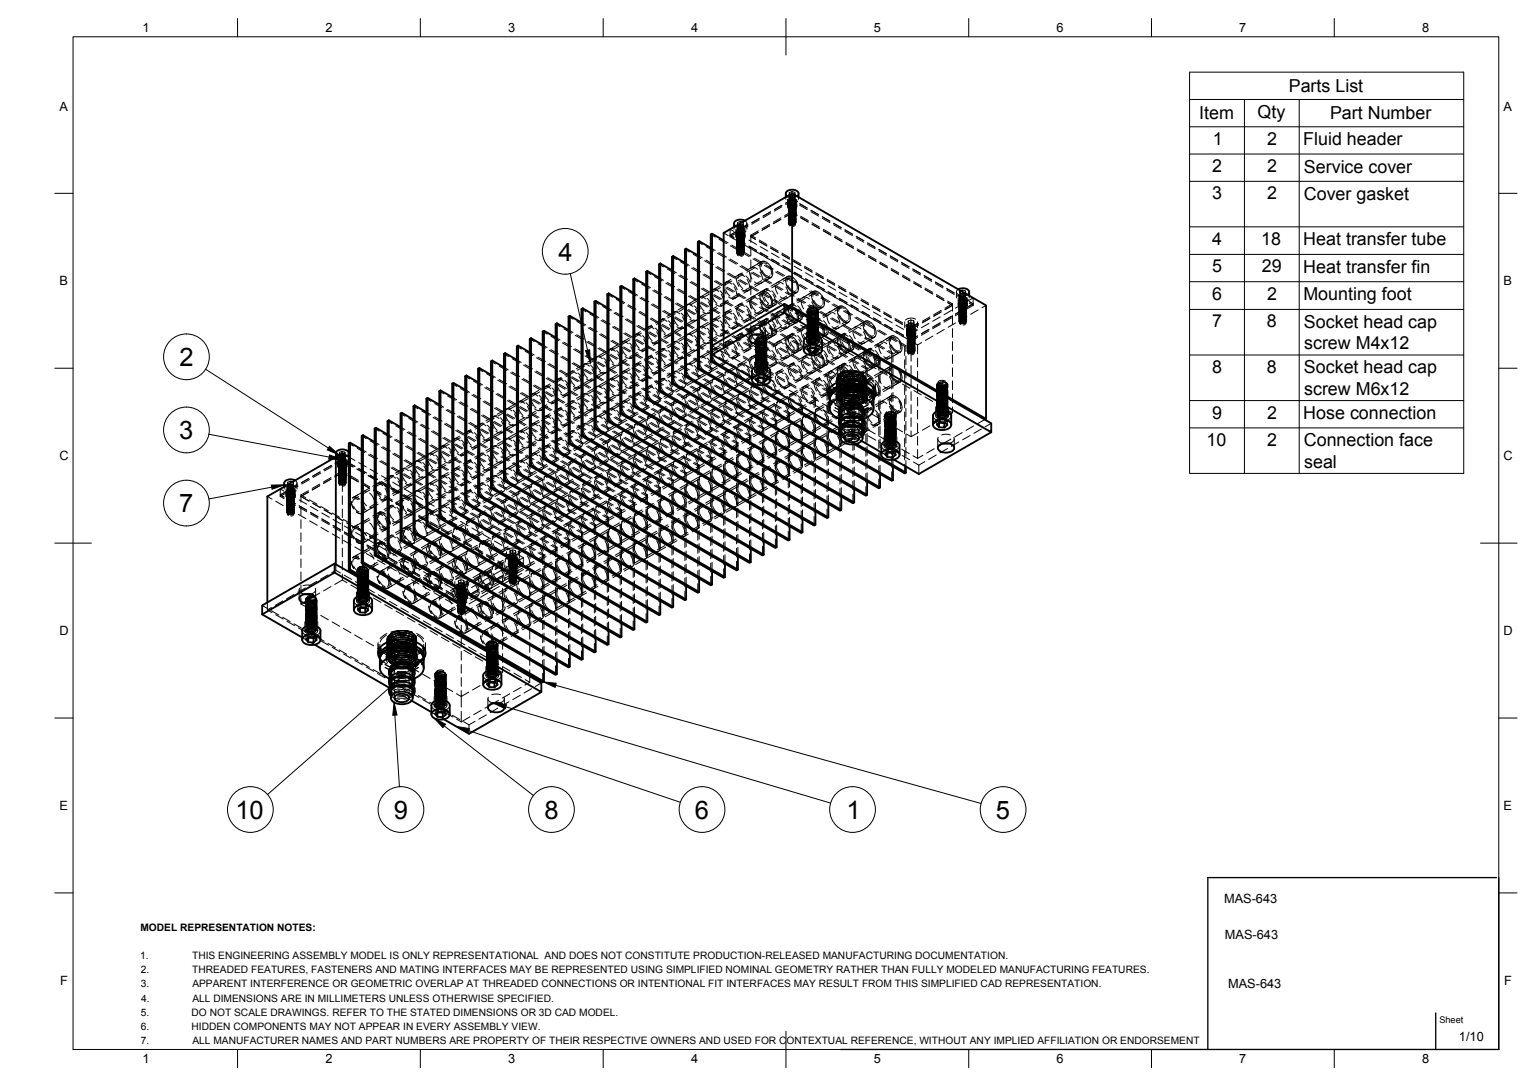
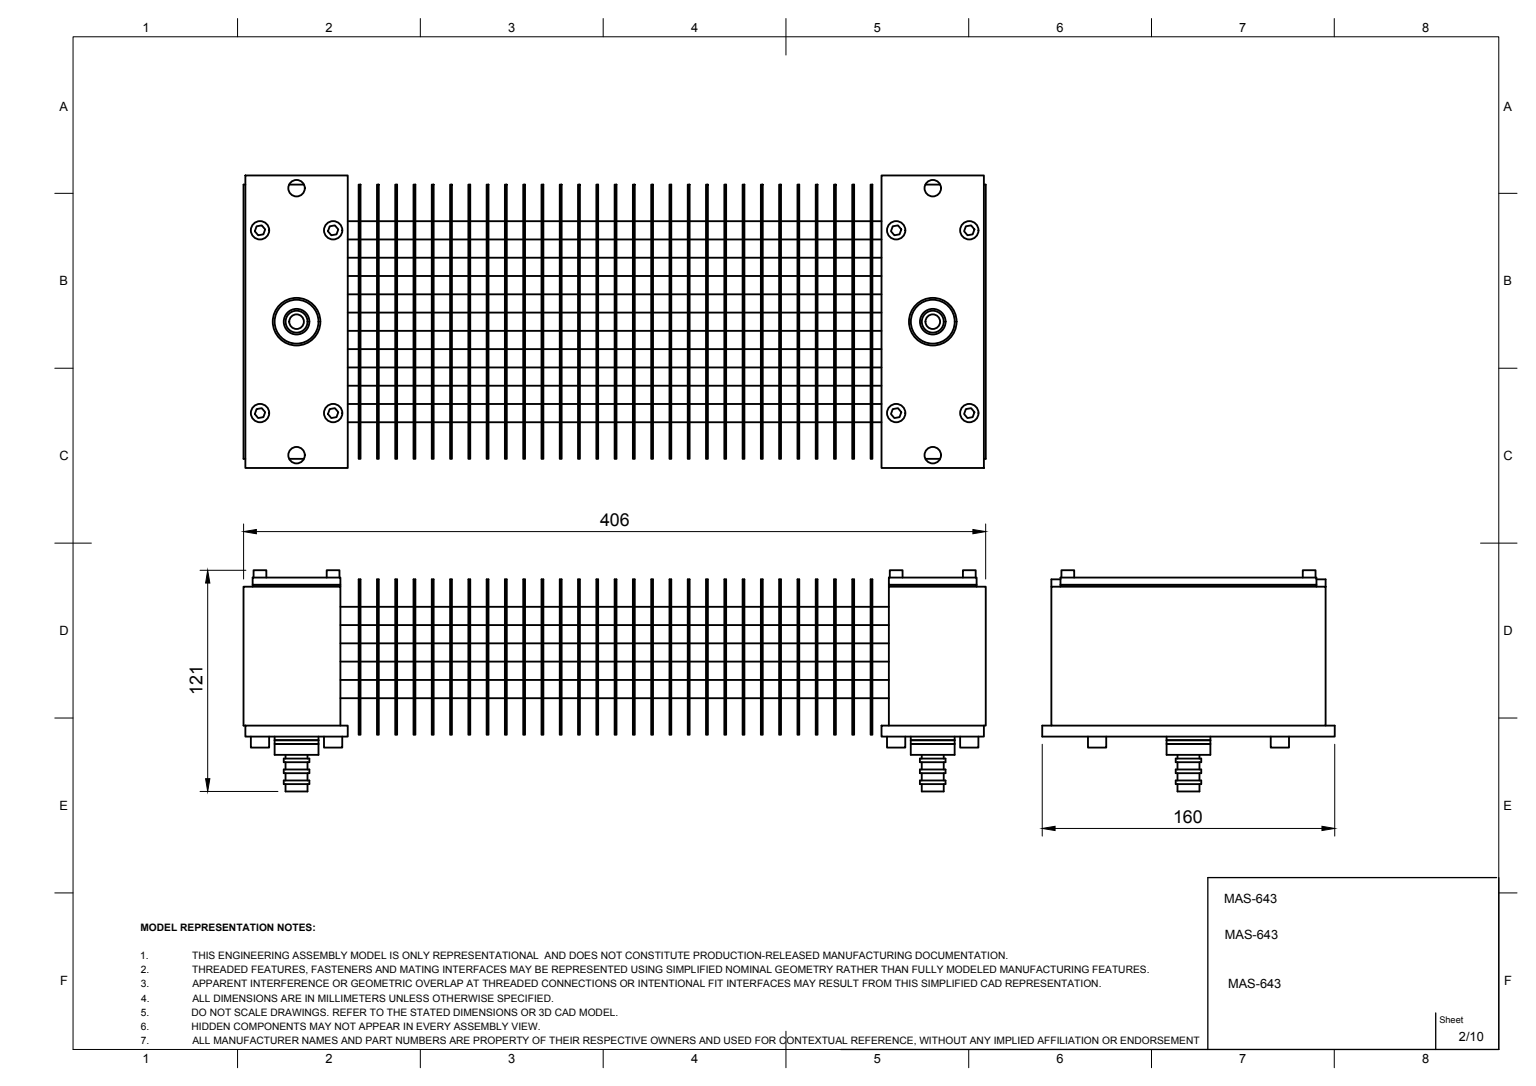
ISO-10303-21;
HEADER;
/* Generated by software containing ST-Developer
 * from STEP Tools, Inc. (www.steptools.com) 
 */

FILE_DESCRIPTION(
/* description */ ('Independent eighteen-tube parallel-flow evaporator geometry. Repeated
 machined headers and gasketed service covers, eighteen copper tubes, 
twenty-nine punched fins, threaded hose connections and bolted mountin
g feet. Native editable features and instanced parts. Braze details, w
orking fluid, pressure and thermal ratings require engineering selecti
on.'),
/* implementation_level */ '2;1');

FILE_NAME(
/* name */ 'MAS-643.step',
/* time_stamp */ '2026-11-08T20:53:59-08:00',
/* author */ (''),
/* organization */ (''),
/* preprocessor_version */ 'ST-DEVELOPER v20.2',
/* originating_system */ 'Autodesk Translation Framework v15.17.0.0',
/* authorisation */ '');

FILE_SCHEMA (('AUTOMOTIVE_DESIGN { 1 0 10303 214 3 1 1 }'));
ENDSEC;

DATA;
#10=MECHANICAL_DESIGN_GEOMETRIC_PRESENTATION_REPRESENTATION('',(#333,#334,
#335,#336,#337,#338,#339,#340,#341,#342),#42620);
#11=ITEM_DEFINED_TRANSFORMATION($,$,#10505,#11231);
#12=ITEM_DEFINED_TRANSFORMATION($,$,#10921,#11232);
#13=ITEM_DEFINED_TRANSFORMATION($,$,#10940,#11233);
#14=ITEM_DEFINED_TRANSFORMATION($,$,#10963,#11234);
#15=ITEM_DEFINED_TRANSFORMATION($,$,#10972,#11235);
#16=ITEM_DEFINED_TRANSFORMATION($,$,#11033,#11236);
#17=ITEM_DEFINED_TRANSFORMATION($,$,#11061,#11237);
#18=ITEM_DEFINED_TRANSFORMATION($,$,#11115,#11238);
#19=ITEM_DEFINED_TRANSFORMATION($,$,#11159,#11239);
#20=ITEM_DEFINED_TRANSFORMATION($,$,#11222,#11240);
#21=ITEM_DEFINED_TRANSFORMATION($,$,#10505,#11241);
#22=ITEM_DEFINED_TRANSFORMATION($,$,#10921,#11242);
#23=ITEM_DEFINED_TRANSFORMATION($,$,#10940,#11243);
#24=ITEM_DEFINED_TRANSFORMATION($,$,#10963,#11244);
#25=ITEM_DEFINED_TRANSFORMATION($,$,#10963,#11245);
#26=ITEM_DEFINED_TRANSFORMATION($,$,#10963,#11246);
#27=ITEM_DEFINED_TRANSFORMATION($,$,#10963,#11247);
#28=ITEM_DEFINED_TRANSFORMATION($,$,#10963,#11248);
#29=ITEM_DEFINED_TRANSFORMATION($,$,#10963,#11249);
#30=ITEM_DEFINED_TRANSFORMATION($,$,#10963,#11250);
#31=ITEM_DEFINED_TRANSFORMATION($,$,#10963,#11251);
#32=ITEM_DEFINED_TRANSFORMATION($,$,#10963,#11252);
#33=ITEM_DEFINED_TRANSFORMATION($,$,#10963,#11253);
#34=ITEM_DEFINED_TRANSFORMATION($,$,#10963,#11254);
#35=ITEM_DEFINED_TRANSFORMATION($,$,#10963,#11255);
#36=ITEM_DEFINED_TRANSFORMATION($,$,#10963,#11256);
#37=ITEM_DEFINED_TRANSFORMATION($,$,#10963,#11257);
#38=ITEM_DEFINED_TRANSFORMATION($,$,#10963,#11258);
#39=ITEM_DEFINED_TRANSFORMATION($,$,#10963,#11259);
#40=ITEM_DEFINED_TRANSFORMATION($,$,#10963,#11260);
#41=ITEM_DEFINED_TRANSFORMATION($,$,#10972,#11261);
#42=ITEM_DEFINED_TRANSFORMATION($,$,#10972,#11262);
#43=ITEM_DEFINED_TRANSFORMATION($,$,#10972,#11263);
#44=ITEM_DEFINED_TRANSFORMATION($,$,#10972,#11264);
#45=ITEM_DEFINED_TRANSFORMATION($,$,#10972,#11265);
#46=ITEM_DEFINED_TRANSFORMATION($,$,#10972,#11266);
#47=ITEM_DEFINED_TRANSFORMATION($,$,#10972,#11267);
#48=ITEM_DEFINED_TRANSFORMATION($,$,#10972,#11268);
#49=ITEM_DEFINED_TRANSFORMATION($,$,#10972,#11269);
#50=ITEM_DEFINED_TRANSFORMATION($,$,#10972,#11270);
#51=ITEM_DEFINED_TRANSFORMATION($,$,#10972,#11271);
#52=ITEM_DEFINED_TRANSFORMATION($,$,#10972,#11272);
#53=ITEM_DEFINED_TRANSFORMATION($,$,#10972,#11273);
#54=ITEM_DEFINED_TRANSFORMATION($,$,#10972,#11274);
#55=ITEM_DEFINED_TRANSFORMATION($,$,#10972,#11275);
#56=ITEM_DEFINED_TRANSFORMATION($,$,#10972,#11276);
#57=ITEM_DEFINED_TRANSFORMATION($,$,#10972,#11277);
#58=ITEM_DEFINED_TRANSFORMATION($,$,#10972,#11278);
#59=ITEM_DEFINED_TRANSFORMATION($,$,#10972,#11279);
#60=ITEM_DEFINED_TRANSFORMATION($,$,#10972,#11280);
#61=ITEM_DEFINED_TRANSFORMATION($,$,#10972,#11281);
#62=ITEM_DEFINED_TRANSFORMATION($,$,#10972,#11282);
#63=ITEM_DEFINED_TRANSFORMATION($,$,#10972,#11283);
#64=ITEM_DEFINED_TRANSFORMATION($,$,#10972,#11284);
#65=ITEM_DEFINED_TRANSFORMATION($,$,#10972,#11285);
#66=ITEM_DEFINED_TRANSFORMATION($,$,#10972,#11286);
#67=ITEM_DEFINED_TRANSFORMATION($,$,#10972,#11287);
#68=ITEM_DEFINED_TRANSFORMATION($,$,#10972,#11288);
#69=ITEM_DEFINED_TRANSFORMATION($,$,#11033,#11289);
#70=ITEM_DEFINED_TRANSFORMATION($,$,#11061,#11290);
#71=ITEM_DEFINED_TRANSFORMATION($,$,#11061,#11291);
#72=ITEM_DEFINED_TRANSFORMATION($,$,#11061,#11292);
#73=ITEM_DEFINED_TRANSFORMATION($,$,#11061,#11293);
#74=ITEM_DEFINED_TRANSFORMATION($,$,#11061,#11294);
#75=ITEM_DEFINED_TRANSFORMATION($,$,#11061,#11295);
#76=ITEM_DEFINED_TRANSFORMATION($,$,#11061,#11296);
#77=ITEM_DEFINED_TRANSFORMATION($,$,#11115,#11297);
#78=ITEM_DEFINED_TRANSFORMATION($,$,#11115,#11298);
#79=ITEM_DEFINED_TRANSFORMATION($,$,#11115,#11299);
#80=ITEM_DEFINED_TRANSFORMATION($,$,#11115,#11300);
#81=ITEM_DEFINED_TRANSFORMATION($,$,#11115,#11301);
#82=ITEM_DEFINED_TRANSFORMATION($,$,#11115,#11302);
#83=ITEM_DEFINED_TRANSFORMATION($,$,#11115,#11303);
#84=ITEM_DEFINED_TRANSFORMATION($,$,#11159,#11304);
#85=ITEM_DEFINED_TRANSFORMATION($,$,#11222,#11305);
#86=(
REPRESENTATION_RELATIONSHIP($,$,#42723,#42722)
REPRESENTATION_RELATIONSHIP_WITH_TRANSFORMATION(#11)
SHAPE_REPRESENTATION_RELATIONSHIP()
);
#87=(
REPRESENTATION_RELATIONSHIP($,$,#42724,#42722)
REPRESENTATION_RELATIONSHIP_WITH_TRANSFORMATION(#12)
SHAPE_REPRESENTATION_RELATIONSHIP()
);
#88=(
REPRESENTATION_RELATIONSHIP($,$,#42725,#42722)
REPRESENTATION_RELATIONSHIP_WITH_TRANSFORMATION(#13)
SHAPE_REPRESENTATION_RELATIONSHIP()
);
#89=(
REPRESENTATION_RELATIONSHIP($,$,#42726,#42722)
REPRESENTATION_RELATIONSHIP_WITH_TRANSFORMATION(#14)
SHAPE_REPRESENTATION_RELATIONSHIP()
);
#90=(
REPRESENTATION_RELATIONSHIP($,$,#42727,#42722)
REPRESENTATION_RELATIONSHIP_WITH_TRANSFORMATION(#15)
SHAPE_REPRESENTATION_RELATIONSHIP()
);
#91=(
REPRESENTATION_RELATIONSHIP($,$,#42728,#42722)
REPRESENTATION_RELATIONSHIP_WITH_TRANSFORMATION(#16)
SHAPE_REPRESENTATION_RELATIONSHIP()
);
#92=(
REPRESENTATION_RELATIONSHIP($,$,#42729,#42722)
REPRESENTATION_RELATIONSHIP_WITH_TRANSFORMATION(#17)
SHAPE_REPRESENTATION_RELATIONSHIP()
);
#93=(
REPRESENTATION_RELATIONSHIP($,$,#42730,#42722)
REPRESENTATION_RELATIONSHIP_WITH_TRANSFORMATION(#18)
SHAPE_REPRESENTATION_RELATIONSHIP()
);
#94=(
REPRESENTATION_RELATIONSHIP($,$,#42731,#42722)
REPRESENTATION_RELATIONSHIP_WITH_TRANSFORMATION(#19)
SHAPE_REPRESENTATION_RELATIONSHIP()
);
#95=(
REPRESENTATION_RELATIONSHIP($,$,#42732,#42722)
REPRESENTATION_RELATIONSHIP_WITH_TRANSFORMATION(#20)
SHAPE_REPRESENTATION_RELATIONSHIP()
);
#96=(
REPRESENTATION_RELATIONSHIP($,$,#42723,#42722)
REPRESENTATION_RELATIONSHIP_WITH_TRANSFORMATION(#21)
SHAPE_REPRESENTATION_RELATIONSHIP()
);
#97=(
REPRESENTATION_RELATIONSHIP($,$,#42724,#42722)
REPRESENTATION_RELATIONSHIP_WITH_TRANSFORMATION(#22)
SHAPE_REPRESENTATION_RELATIONSHIP()
);
#98=(
REPRESENTATION_RELATIONSHIP($,$,#42725,#42722)
REPRESENTATION_RELATIONSHIP_WITH_TRANSFORMATION(#23)
SHAPE_REPRESENTATION_RELATIONSHIP()
);
#99=(
REPRESENTATION_RELATIONSHIP($,$,#42726,#42722)
REPRESENTATION_RELATIONSHIP_WITH_TRANSFORMATION(#24)
SHAPE_REPRESENTATION_RELATIONSHIP()
);
#100=(
REPRESENTATION_RELATIONSHIP($,$,#42726,#42722)
REPRESENTATION_RELATIONSHIP_WITH_TRANSFORMATION(#25)
SHAPE_REPRESENTATION_RELATIONSHIP()
);
#101=(
REPRESENTATION_RELATIONSHIP($,$,#42726,#42722)
REPRESENTATION_RELATIONSHIP_WITH_TRANSFORMATION(#26)
SHAPE_REPRESENTATION_RELATIONSHIP()
);
#102=(
REPRESENTATION_RELATIONSHIP($,$,#42726,#42722)
REPRESENTATION_RELATIONSHIP_WITH_TRANSFORMATION(#27)
SHAPE_REPRESENTATION_RELATIONSHIP()
);
#103=(
REPRESENTATION_RELATIONSHIP($,$,#42726,#42722)
REPRESENTATION_RELATIONSHIP_WITH_TRANSFORMATION(#28)
SHAPE_REPRESENTATION_RELATIONSHIP()
);
#104=(
REPRESENTATION_RELATIONSHIP($,$,#42726,#42722)
REPRESENTATION_RELATIONSHIP_WITH_TRANSFORMATION(#29)
SHAPE_REPRESENTATION_RELATIONSHIP()
);
#105=(
REPRESENTATION_RELATIONSHIP($,$,#42726,#42722)
REPRESENTATION_RELATIONSHIP_WITH_TRANSFORMATION(#30)
SHAPE_REPRESENTATION_RELATIONSHIP()
);
#106=(
REPRESENTATION_RELATIONSHIP($,$,#42726,#42722)
REPRESENTATION_RELATIONSHIP_WITH_TRANSFORMATION(#31)
SHAPE_REPRESENTATION_RELATIONSHIP()
);
#107=(
REPRESENTATION_RELATIONSHIP($,$,#42726,#42722)
REPRESENTATION_RELATIONSHIP_WITH_TRANSFORMATION(#32)
SHAPE_REPRESENTATION_RELATIONSHIP()
);
#108=(
REPRESENTATION_RELATIONSHIP($,$,#42726,#42722)
REPRESENTATION_RELATIONSHIP_WITH_TRANSFORMATION(#33)
SHAPE_REPRESENTATION_RELATIONSHIP()
);
#109=(
REPRESENTATION_RELATIONSHIP($,$,#42726,#42722)
REPRESENTATION_RELATIONSHIP_WITH_TRANSFORMATION(#34)
SHAPE_REPRESENTATION_RELATIONSHIP()
);
#110=(
REPRESENTATION_RELATIONSHIP($,$,#42726,#42722)
REPRESENTATION_RELATIONSHIP_WITH_TRANSFORMATION(#35)
SHAPE_REPRESENTATION_RELATIONSHIP()
);
#111=(
REPRESENTATION_RELATIONSHIP($,$,#42726,#42722)
REPRESENTATION_RELATIONSHIP_WITH_TRANSFORMATION(#36)
SHAPE_REPRESENTATION_RELATIONSHIP()
);
#112=(
REPRESENTATION_RELATIONSHIP($,$,#42726,#42722)
REPRESENTATION_RELATIONSHIP_WITH_TRANSFORMATION(#37)
SHAPE_REPRESENTATION_RELATIONSHIP()
);
#113=(
REPRESENTATION_RELATIONSHIP($,$,#42726,#42722)
REPRESENTATION_RELATIONSHIP_WITH_TRANSFORMATION(#38)
SHAPE_REPRESENTATION_RELATIONSHIP()
);
#114=(
REPRESENTATION_RELATIONSHIP($,$,#42726,#42722)
REPRESENTATION_RELATIONSHIP_WITH_TRANSFORMATION(#39)
SHAPE_REPRESENTATION_RELATIONSHIP()
);
#115=(
REPRESENTATION_RELATIONSHIP($,$,#42726,#42722)
REPRESENTATION_RELATIONSHIP_WITH_TRANSFORMATION(#40)
SHAPE_REPRESENTATION_RELATIONSHIP()
);
#116=(
REPRESENTATION_RELATIONSHIP($,$,#42727,#42722)
REPRESENTATION_RELATIONSHIP_WITH_TRANSFORMATION(#41)
SHAPE_REPRESENTATION_RELATIONSHIP()
);
#117=(
REPRESENTATION_RELATIONSHIP($,$,#42727,#42722)
REPRESENTATION_RELATIONSHIP_WITH_TRANSFORMATION(#42)
SHAPE_REPRESENTATION_RELATIONSHIP()
);
#118=(
REPRESENTATION_RELATIONSHIP($,$,#42727,#42722)
REPRESENTATION_RELATIONSHIP_WITH_TRANSFORMATION(#43)
SHAPE_REPRESENTATION_RELATIONSHIP()
);
#119=(
REPRESENTATION_RELATIONSHIP($,$,#42727,#42722)
REPRESENTATION_RELATIONSHIP_WITH_TRANSFORMATION(#44)
SHAPE_REPRESENTATION_RELATIONSHIP()
);
#120=(
REPRESENTATION_RELATIONSHIP($,$,#42727,#42722)
REPRESENTATION_RELATIONSHIP_WITH_TRANSFORMATION(#45)
SHAPE_REPRESENTATION_RELATIONSHIP()
);
#121=(
REPRESENTATION_RELATIONSHIP($,$,#42727,#42722)
REPRESENTATION_RELATIONSHIP_WITH_TRANSFORMATION(#46)
SHAPE_REPRESENTATION_RELATIONSHIP()
);
#122=(
REPRESENTATION_RELATIONSHIP($,$,#42727,#42722)
REPRESENTATION_RELATIONSHIP_WITH_TRANSFORMATION(#47)
SHAPE_REPRESENTATION_RELATIONSHIP()
);
#123=(
REPRESENTATION_RELATIONSHIP($,$,#42727,#42722)
REPRESENTATION_RELATIONSHIP_WITH_TRANSFORMATION(#48)
SHAPE_REPRESENTATION_RELATIONSHIP()
);
#124=(
REPRESENTATION_RELATIONSHIP($,$,#42727,#42722)
REPRESENTATION_RELATIONSHIP_WITH_TRANSFORMATION(#49)
SHAPE_REPRESENTATION_RELATIONSHIP()
);
#125=(
REPRESENTATION_RELATIONSHIP($,$,#42727,#42722)
REPRESENTATION_RELATIONSHIP_WITH_TRANSFORMATION(#50)
SHAPE_REPRESENTATION_RELATIONSHIP()
);
#126=(
REPRESENTATION_RELATIONSHIP($,$,#42727,#42722)
REPRESENTATION_RELATIONSHIP_WITH_TRANSFORMATION(#51)
SHAPE_REPRESENTATION_RELATIONSHIP()
);
#127=(
REPRESENTATION_RELATIONSHIP($,$,#42727,#42722)
REPRESENTATION_RELATIONSHIP_WITH_TRANSFORMATION(#52)
SHAPE_REPRESENTATION_RELATIONSHIP()
);
#128=(
REPRESENTATION_RELATIONSHIP($,$,#42727,#42722)
REPRESENTATION_RELATIONSHIP_WITH_TRANSFORMATION(#53)
SHAPE_REPRESENTATION_RELATIONSHIP()
);
#129=(
REPRESENTATION_RELATIONSHIP($,$,#42727,#42722)
REPRESENTATION_RELATIONSHIP_WITH_TRANSFORMATION(#54)
SHAPE_REPRESENTATION_RELATIONSHIP()
);
#130=(
REPRESENTATION_RELATIONSHIP($,$,#42727,#42722)
REPRESENTATION_RELATIONSHIP_WITH_TRANSFORMATION(#55)
SHAPE_REPRESENTATION_RELATIONSHIP()
);
#131=(
REPRESENTATION_RELATIONSHIP($,$,#42727,#42722)
REPRESENTATION_RELATIONSHIP_WITH_TRANSFORMATION(#56)
SHAPE_REPRESENTATION_RELATIONSHIP()
);
#132=(
REPRESENTATION_RELATIONSHIP($,$,#42727,#42722)
REPRESENTATION_RELATIONSHIP_WITH_TRANSFORMATION(#57)
SHAPE_REPRESENTATION_RELATIONSHIP()
);
#133=(
REPRESENTATION_RELATIONSHIP($,$,#42727,#42722)
REPRESENTATION_RELATIONSHIP_WITH_TRANSFORMATION(#58)
SHAPE_REPRESENTATION_RELATIONSHIP()
);
#134=(
REPRESENTATION_RELATIONSHIP($,$,#42727,#42722)
REPRESENTATION_RELATIONSHIP_WITH_TRANSFORMATION(#59)
SHAPE_REPRESENTATION_RELATIONSHIP()
);
#135=(
REPRESENTATION_RELATIONSHIP($,$,#42727,#42722)
REPRESENTATION_RELATIONSHIP_WITH_TRANSFORMATION(#60)
SHAPE_REPRESENTATION_RELATIONSHIP()
);
#136=(
REPRESENTATION_RELATIONSHIP($,$,#42727,#42722)
REPRESENTATION_RELATIONSHIP_WITH_TRANSFORMATION(#61)
SHAPE_REPRESENTATION_RELATIONSHIP()
);
#137=(
REPRESENTATION_RELATIONSHIP($,$,#42727,#42722)
REPRESENTATION_RELATIONSHIP_WITH_TRANSFORMATION(#62)
SHAPE_REPRESENTATION_RELATIONSHIP()
);
#138=(
REPRESENTATION_RELATIONSHIP($,$,#42727,#42722)
REPRESENTATION_RELATIONSHIP_WITH_TRANSFORMATION(#63)
SHAPE_REPRESENTATION_RELATIONSHIP()
);
#139=(
REPRESENTATION_RELATIONSHIP($,$,#42727,#42722)
REPRESENTATION_RELATIONSHIP_WITH_TRANSFORMATION(#64)
SHAPE_REPRESENTATION_RELATIONSHIP()
);
#140=(
REPRESENTATION_RELATIONSHIP($,$,#42727,#42722)
REPRESENTATION_RELATIONSHIP_WITH_TRANSFORMATION(#65)
SHAPE_REPRESENTATION_RELATIONSHIP()
);
#141=(
REPRESENTATION_RELATIONSHIP($,$,#42727,#42722)
REPRESENTATION_RELATIONSHIP_WITH_TRANSFORMATION(#66)
SHAPE_REPRESENTATION_RELATIONSHIP()
);
#142=(
REPRESENTATION_RELATIONSHIP($,$,#42727,#42722)
REPRESENTATION_RELATIONSHIP_WITH_TRANSFORMATION(#67)
SHAPE_REPRESENTATION_RELATIONSHIP()
);
#143=(
REPRESENTATION_RELATIONSHIP($,$,#42727,#42722)
REPRESENTATION_RELATIONSHIP_WITH_TRANSFORMATION(#68)
SHAPE_REPRESENTATION_RELATIONSHIP()
);
#144=(
REPRESENTATION_RELATIONSHIP($,$,#42728,#42722)
REPRESENTATION_RELATIONSHIP_WITH_TRANSFORMATION(#69)
SHAPE_REPRESENTATION_RELATIONSHIP()
);
#145=(
REPRESENTATION_RELATIONSHIP($,$,#42729,#42722)
REPRESENTATION_RELATIONSHIP_WITH_TRANSFORMATION(#70)
SHAPE_REPRESENTATION_RELATIONSHIP()
);
#146=(
REPRESENTATION_RELATIONSHIP($,$,#42729,#42722)
REPRESENTATION_RELATIONSHIP_WITH_TRANSFORMATION(#71)
SHAPE_REPRESENTATION_RELATIONSHIP()
);
#147=(
REPRESENTATION_RELATIONSHIP($,$,#42729,#42722)
REPRESENTATION_RELATIONSHIP_WITH_TRANSFORMATION(#72)
SHAPE_REPRESENTATION_RELATIONSHIP()
);
#148=(
REPRESENTATION_RELATIONSHIP($,$,#42729,#42722)
REPRESENTATION_RELATIONSHIP_WITH_TRANSFORMATION(#73)
SHAPE_REPRESENTATION_RELATIONSHIP()
);
#149=(
REPRESENTATION_RELATIONSHIP($,$,#42729,#42722)
REPRESENTATION_RELATIONSHIP_WITH_TRANSFORMATION(#74)
SHAPE_REPRESENTATION_RELATIONSHIP()
);
#150=(
REPRESENTATION_RELATIONSHIP($,$,#42729,#42722)
REPRESENTATION_RELATIONSHIP_WITH_TRANSFORMATION(#75)
SHAPE_REPRESENTATION_RELATIONSHIP()
);
#151=(
REPRESENTATION_RELATIONSHIP($,$,#42729,#42722)
REPRESENTATION_RELATIONSHIP_WITH_TRANSFORMATION(#76)
SHAPE_REPRESENTATION_RELATIONSHIP()
);
#152=(
REPRESENTATION_RELATIONSHIP($,$,#42730,#42722)
REPRESENTATION_RELATIONSHIP_WITH_TRANSFORMATION(#77)
SHAPE_REPRESENTATION_RELATIONSHIP()
);
#153=(
REPRESENTATION_RELATIONSHIP($,$,#42730,#42722)
REPRESENTATION_RELATIONSHIP_WITH_TRANSFORMATION(#78)
SHAPE_REPRESENTATION_RELATIONSHIP()
);
#154=(
REPRESENTATION_RELATIONSHIP($,$,#42730,#42722)
REPRESENTATION_RELATIONSHIP_WITH_TRANSFORMATION(#79)
SHAPE_REPRESENTATION_RELATIONSHIP()
);
#155=(
REPRESENTATION_RELATIONSHIP($,$,#42730,#42722)
REPRESENTATION_RELATIONSHIP_WITH_TRANSFORMATION(#80)
SHAPE_REPRESENTATION_RELATIONSHIP()
);
#156=(
REPRESENTATION_RELATIONSHIP($,$,#42730,#42722)
REPRESENTATION_RELATIONSHIP_WITH_TRANSFORMATION(#81)
SHAPE_REPRESENTATION_RELATIONSHIP()
);
#157=(
REPRESENTATION_RELATIONSHIP($,$,#42730,#42722)
REPRESENTATION_RELATIONSHIP_WITH_TRANSFORMATION(#82)
SHAPE_REPRESENTATION_RELATIONSHIP()
);
#158=(
REPRESENTATION_RELATIONSHIP($,$,#42730,#42722)
REPRESENTATION_RELATIONSHIP_WITH_TRANSFORMATION(#83)
SHAPE_REPRESENTATION_RELATIONSHIP()
);
#159=(
REPRESENTATION_RELATIONSHIP($,$,#42731,#42722)
REPRESENTATION_RELATIONSHIP_WITH_TRANSFORMATION(#84)
SHAPE_REPRESENTATION_RELATIONSHIP()
);
#160=(
REPRESENTATION_RELATIONSHIP($,$,#42732,#42722)
REPRESENTATION_RELATIONSHIP_WITH_TRANSFORMATION(#85)
SHAPE_REPRESENTATION_RELATIONSHIP()
);
#161=CONTEXT_DEPENDENT_SHAPE_REPRESENTATION(#86,#42647);
#162=CONTEXT_DEPENDENT_SHAPE_REPRESENTATION(#87,#42648);
#163=CONTEXT_DEPENDENT_SHAPE_REPRESENTATION(#88,#42649);
#164=CONTEXT_DEPENDENT_SHAPE_REPRESENTATION(#89,#42650);
#165=CONTEXT_DEPENDENT_SHAPE_REPRESENTATION(#90,#42651);
#166=CONTEXT_DEPENDENT_SHAPE_REPRESENTATION(#91,#42652);
#167=CONTEXT_DEPENDENT_SHAPE_REPRESENTATION(#92,#42653);
#168=CONTEXT_DEPENDENT_SHAPE_REPRESENTATION(#93,#42654);
#169=CONTEXT_DEPENDENT_SHAPE_REPRESENTATION(#94,#42655);
#170=CONTEXT_DEPENDENT_SHAPE_REPRESENTATION(#95,#42656);
#171=CONTEXT_DEPENDENT_SHAPE_REPRESENTATION(#96,#42657);
#172=CONTEXT_DEPENDENT_SHAPE_REPRESENTATION(#97,#42658);
#173=CONTEXT_DEPENDENT_SHAPE_REPRESENTATION(#98,#42659);
#174=CONTEXT_DEPENDENT_SHAPE_REPRESENTATION(#99,#42660);
#175=CONTEXT_DEPENDENT_SHAPE_REPRESENTATION(#100,#42661);
#176=CONTEXT_DEPENDENT_SHAPE_REPRESENTATION(#101,#42662);
#177=CONTEXT_DEPENDENT_SHAPE_REPRESENTATION(#102,#42663);
#178=CONTEXT_DEPENDENT_SHAPE_REPRESENTATION(#103,#42664);
#179=CONTEXT_DEPENDENT_SHAPE_REPRESENTATION(#104,#42665);
#180=CONTEXT_DEPENDENT_SHAPE_REPRESENTATION(#105,#42666);
#181=CONTEXT_DEPENDENT_SHAPE_REPRESENTATION(#106,#42667);
#182=CONTEXT_DEPENDENT_SHAPE_REPRESENTATION(#107,#42668);
#183=CONTEXT_DEPENDENT_SHAPE_REPRESENTATION(#108,#42669);
#184=CONTEXT_DEPENDENT_SHAPE_REPRESENTATION(#109,#42670);
#185=CONTEXT_DEPENDENT_SHAPE_REPRESENTATION(#110,#42671);
#186=CONTEXT_DEPENDENT_SHAPE_REPRESENTATION(#111,#42672);
#187=CONTEXT_DEPENDENT_SHAPE_REPRESENTATION(#112,#42673);
#188=CONTEXT_DEPENDENT_SHAPE_REPRESENTATION(#113,#42674);
#189=CONTEXT_DEPENDENT_SHAPE_REPRESENTATION(#114,#42675);
#190=CONTEXT_DEPENDENT_SHAPE_REPRESENTATION(#115,#42676);
#191=CONTEXT_DEPENDENT_SHAPE_REPRESENTATION(#116,#42677);
#192=CONTEXT_DEPENDENT_SHAPE_REPRESENTATION(#117,#42678);
#193=CONTEXT_DEPENDENT_SHAPE_REPRESENTATION(#118,#42679);
#194=CONTEXT_DEPENDENT_SHAPE_REPRESENTATION(#119,#42680);
#195=CONTEXT_DEPENDENT_SHAPE_REPRESENTATION(#120,#42681);
#196=CONTEXT_DEPENDENT_SHAPE_REPRESENTATION(#121,#42682);
#197=CONTEXT_DEPENDENT_SHAPE_REPRESENTATION(#122,#42683);
#198=CONTEXT_DEPENDENT_SHAPE_REPRESENTATION(#123,#42684);
#199=CONTEXT_DEPENDENT_SHAPE_REPRESENTATION(#124,#42685);
#200=CONTEXT_DEPENDENT_SHAPE_REPRESENTATION(#125,#42686);
#201=CONTEXT_DEPENDENT_SHAPE_REPRESENTATION(#126,#42687);
#202=CONTEXT_DEPENDENT_SHAPE_REPRESENTATION(#127,#42688);
#203=CONTEXT_DEPENDENT_SHAPE_REPRESENTATION(#128,#42689);
#204=CONTEXT_DEPENDENT_SHAPE_REPRESENTATION(#129,#42690);
#205=CONTEXT_DEPENDENT_SHAPE_REPRESENTATION(#130,#42691);
#206=CONTEXT_DEPENDENT_SHAPE_REPRESENTATION(#131,#42692);
#207=CONTEXT_DEPENDENT_SHAPE_REPRESENTATION(#132,#42693);
#208=CONTEXT_DEPENDENT_SHAPE_REPRESENTATION(#133,#42694);
#209=CONTEXT_DEPENDENT_SHAPE_REPRESENTATION(#134,#42695);
#210=CONTEXT_DEPENDENT_SHAPE_REPRESENTATION(#135,#42696);
#211=CONTEXT_DEPENDENT_SHAPE_REPRESENTATION(#136,#42697);
#212=CONTEXT_DEPENDENT_SHAPE_REPRESENTATION(#137,#42698);
#213=CONTEXT_DEPENDENT_SHAPE_REPRESENTATION(#138,#42699);
#214=CONTEXT_DEPENDENT_SHAPE_REPRESENTATION(#139,#42700);
#215=CONTEXT_DEPENDENT_SHAPE_REPRESENTATION(#140,#42701);
#216=CONTEXT_DEPENDENT_SHAPE_REPRESENTATION(#141,#42702);
#217=CONTEXT_DEPENDENT_SHAPE_REPRESENTATION(#142,#42703);
#218=CONTEXT_DEPENDENT_SHAPE_REPRESENTATION(#143,#42704);
#219=CONTEXT_DEPENDENT_SHAPE_REPRESENTATION(#144,#42705);
#220=CONTEXT_DEPENDENT_SHAPE_REPRESENTATION(#145,#42706);
#221=CONTEXT_DEPENDENT_SHAPE_REPRESENTATION(#146,#42707);
#222=CONTEXT_DEPENDENT_SHAPE_REPRESENTATION(#147,#42708);
#223=CONTEXT_DEPENDENT_SHAPE_REPRESENTATION(#148,#42709);
#224=CONTEXT_DEPENDENT_SHAPE_REPRESENTATION(#149,#42710);
#225=CONTEXT_DEPENDENT_SHAPE_REPRESENTATION(#150,#42711);
#226=CONTEXT_DEPENDENT_SHAPE_REPRESENTATION(#151,#42712);
#227=CONTEXT_DEPENDENT_SHAPE_REPRESENTATION(#152,#42713);
#228=CONTEXT_DEPENDENT_SHAPE_REPRESENTATION(#153,#42714);
#229=CONTEXT_DEPENDENT_SHAPE_REPRESENTATION(#154,#42715);
#230=CONTEXT_DEPENDENT_SHAPE_REPRESENTATION(#155,#42716);
#231=CONTEXT_DEPENDENT_SHAPE_REPRESENTATION(#156,#42717);
#232=CONTEXT_DEPENDENT_SHAPE_REPRESENTATION(#157,#42718);
#233=CONTEXT_DEPENDENT_SHAPE_REPRESENTATION(#158,#42719);
#234=CONTEXT_DEPENDENT_SHAPE_REPRESENTATION(#159,#42720);
#235=CONTEXT_DEPENDENT_SHAPE_REPRESENTATION(#160,#42721);
#236=NEXT_ASSEMBLY_USAGE_OCCURRENCE('Fluid header:1','Fluid header:1',
'Fluid header:1',#42734,#42735,'Fluid header:1');
#237=NEXT_ASSEMBLY_USAGE_OCCURRENCE('Service cover:1','Service cover:1',
'Service cover:1',#42734,#42736,'Service cover:1');
#238=NEXT_ASSEMBLY_USAGE_OCCURRENCE('Cover gasket:1','Cover gasket:1',
'Cover gasket:1',#42734,#42737,'Cover gasket:1');
#239=NEXT_ASSEMBLY_USAGE_OCCURRENCE('Heat transfer tube:1',
'Heat transfer tube:1','Heat transfer tube:1',#42734,#42738,
'Heat transfer tube:1');
#240=NEXT_ASSEMBLY_USAGE_OCCURRENCE('Heat transfer fin:1',
'Heat transfer fin:1','Heat transfer fin:1',#42734,#42739,
'Heat transfer fin:1');
#241=NEXT_ASSEMBLY_USAGE_OCCURRENCE('Mounting foot:1','Mounting foot:1',
'Mounting foot:1',#42734,#42740,'Mounting foot:1');
#242=NEXT_ASSEMBLY_USAGE_OCCURRENCE('Socket head cap screw M4x12:1',
'Socket head cap screw M4x12:1','Socket head cap screw M4x12:1',#42734,
#42741,'Socket head cap screw M4x12:1');
#243=NEXT_ASSEMBLY_USAGE_OCCURRENCE('Socket head cap screw M6x12:1',
'Socket head cap screw M6x12:1','Socket head cap screw M6x12:1',#42734,
#42742,'Socket head cap screw M6x12:1');
#244=NEXT_ASSEMBLY_USAGE_OCCURRENCE('Hose connection:1',
'Hose connection:1','Hose connection:1',#42734,#42743,
'Hose connection:1');
#245=NEXT_ASSEMBLY_USAGE_OCCURRENCE('Connection face seal:1',
'Connection face seal:1','Connection face seal:1',#42734,#42744,
'Connection face seal:1');
#246=NEXT_ASSEMBLY_USAGE_OCCURRENCE('Fluid header:2','Fluid header:2',
'Fluid header:2',#42734,#42735,'Fluid header:2');
#247=NEXT_ASSEMBLY_USAGE_OCCURRENCE('Service cover:2','Service cover:2',
'Service cover:2',#42734,#42736,'Service cover:2');
#248=NEXT_ASSEMBLY_USAGE_OCCURRENCE('Cover gasket:2','Cover gasket:2',
'Cover gasket:2',#42734,#42737,'Cover gasket:2');
#249=NEXT_ASSEMBLY_USAGE_OCCURRENCE('Heat transfer tube:2',
'Heat transfer tube:2','Heat transfer tube:2',#42734,#42738,
'Heat transfer tube:2');
#250=NEXT_ASSEMBLY_USAGE_OCCURRENCE('Heat transfer tube:3',
'Heat transfer tube:3','Heat transfer tube:3',#42734,#42738,
'Heat transfer tube:3');
#251=NEXT_ASSEMBLY_USAGE_OCCURRENCE('Heat transfer tube:4',
'Heat transfer tube:4','Heat transfer tube:4',#42734,#42738,
'Heat transfer tube:4');
#252=NEXT_ASSEMBLY_USAGE_OCCURRENCE('Heat transfer tube:5',
'Heat transfer tube:5','Heat transfer tube:5',#42734,#42738,
'Heat transfer tube:5');
#253=NEXT_ASSEMBLY_USAGE_OCCURRENCE('Heat transfer tube:6',
'Heat transfer tube:6','Heat transfer tube:6',#42734,#42738,
'Heat transfer tube:6');
#254=NEXT_ASSEMBLY_USAGE_OCCURRENCE('Heat transfer tube:7',
'Heat transfer tube:7','Heat transfer tube:7',#42734,#42738,
'Heat transfer tube:7');
#255=NEXT_ASSEMBLY_USAGE_OCCURRENCE('Heat transfer tube:8',
'Heat transfer tube:8','Heat transfer tube:8',#42734,#42738,
'Heat transfer tube:8');
#256=NEXT_ASSEMBLY_USAGE_OCCURRENCE('Heat transfer tube:9',
'Heat transfer tube:9','Heat transfer tube:9',#42734,#42738,
'Heat transfer tube:9');
#257=NEXT_ASSEMBLY_USAGE_OCCURRENCE('Heat transfer tube:10',
'Heat transfer tube:10','Heat transfer tube:10',#42734,#42738,
'Heat transfer tube:10');
#258=NEXT_ASSEMBLY_USAGE_OCCURRENCE('Heat transfer tube:11',
'Heat transfer tube:11','Heat transfer tube:11',#42734,#42738,
'Heat transfer tube:11');
#259=NEXT_ASSEMBLY_USAGE_OCCURRENCE('Heat transfer tube:12',
'Heat transfer tube:12','Heat transfer tube:12',#42734,#42738,
'Heat transfer tube:12');
#260=NEXT_ASSEMBLY_USAGE_OCCURRENCE('Heat transfer tube:13',
'Heat transfer tube:13','Heat transfer tube:13',#42734,#42738,
'Heat transfer tube:13');
#261=NEXT_ASSEMBLY_USAGE_OCCURRENCE('Heat transfer tube:14',
'Heat transfer tube:14','Heat transfer tube:14',#42734,#42738,
'Heat transfer tube:14');
#262=NEXT_ASSEMBLY_USAGE_OCCURRENCE('Heat transfer tube:15',
'Heat transfer tube:15','Heat transfer tube:15',#42734,#42738,
'Heat transfer tube:15');
#263=NEXT_ASSEMBLY_USAGE_OCCURRENCE('Heat transfer tube:16',
'Heat transfer tube:16','Heat transfer tube:16',#42734,#42738,
'Heat transfer tube:16');
#264=NEXT_ASSEMBLY_USAGE_OCCURRENCE('Heat transfer tube:17',
'Heat transfer tube:17','Heat transfer tube:17',#42734,#42738,
'Heat transfer tube:17');
#265=NEXT_ASSEMBLY_USAGE_OCCURRENCE('Heat transfer tube:18',
'Heat transfer tube:18','Heat transfer tube:18',#42734,#42738,
'Heat transfer tube:18');
#266=NEXT_ASSEMBLY_USAGE_OCCURRENCE('Heat transfer fin:2',
'Heat transfer fin:2','Heat transfer fin:2',#42734,#42739,
'Heat transfer fin:2');
#267=NEXT_ASSEMBLY_USAGE_OCCURRENCE('Heat transfer fin:3',
'Heat transfer fin:3','Heat transfer fin:3',#42734,#42739,
'Heat transfer fin:3');
#268=NEXT_ASSEMBLY_USAGE_OCCURRENCE('Heat transfer fin:4',
'Heat transfer fin:4','Heat transfer fin:4',#42734,#42739,
'Heat transfer fin:4');
#269=NEXT_ASSEMBLY_USAGE_OCCURRENCE('Heat transfer fin:5',
'Heat transfer fin:5','Heat transfer fin:5',#42734,#42739,
'Heat transfer fin:5');
#270=NEXT_ASSEMBLY_USAGE_OCCURRENCE('Heat transfer fin:6',
'Heat transfer fin:6','Heat transfer fin:6',#42734,#42739,
'Heat transfer fin:6');
#271=NEXT_ASSEMBLY_USAGE_OCCURRENCE('Heat transfer fin:7',
'Heat transfer fin:7','Heat transfer fin:7',#42734,#42739,
'Heat transfer fin:7');
#272=NEXT_ASSEMBLY_USAGE_OCCURRENCE('Heat transfer fin:8',
'Heat transfer fin:8','Heat transfer fin:8',#42734,#42739,
'Heat transfer fin:8');
#273=NEXT_ASSEMBLY_USAGE_OCCURRENCE('Heat transfer fin:9',
'Heat transfer fin:9','Heat transfer fin:9',#42734,#42739,
'Heat transfer fin:9');
#274=NEXT_ASSEMBLY_USAGE_OCCURRENCE('Heat transfer fin:10',
'Heat transfer fin:10','Heat transfer fin:10',#42734,#42739,
'Heat transfer fin:10');
#275=NEXT_ASSEMBLY_USAGE_OCCURRENCE('Heat transfer fin:11',
'Heat transfer fin:11','Heat transfer fin:11',#42734,#42739,
'Heat transfer fin:11');
#276=NEXT_ASSEMBLY_USAGE_OCCURRENCE('Heat transfer fin:12',
'Heat transfer fin:12','Heat transfer fin:12',#42734,#42739,
'Heat transfer fin:12');
#277=NEXT_ASSEMBLY_USAGE_OCCURRENCE('Heat transfer fin:13',
'Heat transfer fin:13','Heat transfer fin:13',#42734,#42739,
'Heat transfer fin:13');
#278=NEXT_ASSEMBLY_USAGE_OCCURRENCE('Heat transfer fin:14',
'Heat transfer fin:14','Heat transfer fin:14',#42734,#42739,
'Heat transfer fin:14');
#279=NEXT_ASSEMBLY_USAGE_OCCURRENCE('Heat transfer fin:15',
'Heat transfer fin:15','Heat transfer fin:15',#42734,#42739,
'Heat transfer fin:15');
#280=NEXT_ASSEMBLY_USAGE_OCCURRENCE('Heat transfer fin:16',
'Heat transfer fin:16','Heat transfer fin:16',#42734,#42739,
'Heat transfer fin:16');
#281=NEXT_ASSEMBLY_USAGE_OCCURRENCE('Heat transfer fin:17',
'Heat transfer fin:17','Heat transfer fin:17',#42734,#42739,
'Heat transfer fin:17');
#282=NEXT_ASSEMBLY_USAGE_OCCURRENCE('Heat transfer fin:18',
'Heat transfer fin:18','Heat transfer fin:18',#42734,#42739,
'Heat transfer fin:18');
#283=NEXT_ASSEMBLY_USAGE_OCCURRENCE('Heat transfer fin:19',
'Heat transfer fin:19','Heat transfer fin:19',#42734,#42739,
'Heat transfer fin:19');
#284=NEXT_ASSEMBLY_USAGE_OCCURRENCE('Heat transfer fin:20',
'Heat transfer fin:20','Heat transfer fin:20',#42734,#42739,
'Heat transfer fin:20');
#285=NEXT_ASSEMBLY_USAGE_OCCURRENCE('Heat transfer fin:21',
'Heat transfer fin:21','Heat transfer fin:21',#42734,#42739,
'Heat transfer fin:21');
#286=NEXT_ASSEMBLY_USAGE_OCCURRENCE('Heat transfer fin:22',
'Heat transfer fin:22','Heat transfer fin:22',#42734,#42739,
'Heat transfer fin:22');
#287=NEXT_ASSEMBLY_USAGE_OCCURRENCE('Heat transfer fin:23',
'Heat transfer fin:23','Heat transfer fin:23',#42734,#42739,
'Heat transfer fin:23');
#288=NEXT_ASSEMBLY_USAGE_OCCURRENCE('Heat transfer fin:24',
'Heat transfer fin:24','Heat transfer fin:24',#42734,#42739,
'Heat transfer fin:24');
#289=NEXT_ASSEMBLY_USAGE_OCCURRENCE('Heat transfer fin:25',
'Heat transfer fin:25','Heat transfer fin:25',#42734,#42739,
'Heat transfer fin:25');
#290=NEXT_ASSEMBLY_USAGE_OCCURRENCE('Heat transfer fin:26',
'Heat transfer fin:26','Heat transfer fin:26',#42734,#42739,
'Heat transfer fin:26');
#291=NEXT_ASSEMBLY_USAGE_OCCURRENCE('Heat transfer fin:27',
'Heat transfer fin:27','Heat transfer fin:27',#42734,#42739,
'Heat transfer fin:27');
#292=NEXT_ASSEMBLY_USAGE_OCCURRENCE('Heat transfer fin:28',
'Heat transfer fin:28','Heat transfer fin:28',#42734,#42739,
'Heat transfer fin:28');
#293=NEXT_ASSEMBLY_USAGE_OCCURRENCE('Heat transfer fin:29',
'Heat transfer fin:29','Heat transfer fin:29',#42734,#42739,
'Heat transfer fin:29');
#294=NEXT_ASSEMBLY_USAGE_OCCURRENCE('Mounting foot:2','Mounting foot:2',
'Mounting foot:2',#42734,#42740,'Mounting foot:2');
#295=NEXT_ASSEMBLY_USAGE_OCCURRENCE('Socket head cap screw M4x12:2',
'Socket head cap screw M4x12:2','Socket head cap screw M4x12:2',#42734,
#42741,'Socket head cap screw M4x12:2');
#296=NEXT_ASSEMBLY_USAGE_OCCURRENCE('Socket head cap screw M4x12:3',
'Socket head cap screw M4x12:3','Socket head cap screw M4x12:3',#42734,
#42741,'Socket head cap screw M4x12:3');
#297=NEXT_ASSEMBLY_USAGE_OCCURRENCE('Socket head cap screw M4x12:4',
'Socket head cap screw M4x12:4','Socket head cap screw M4x12:4',#42734,
#42741,'Socket head cap screw M4x12:4');
#298=NEXT_ASSEMBLY_USAGE_OCCURRENCE('Socket head cap screw M4x12:5',
'Socket head cap screw M4x12:5','Socket head cap screw M4x12:5',#42734,
#42741,'Socket head cap screw M4x12:5');
#299=NEXT_ASSEMBLY_USAGE_OCCURRENCE('Socket head cap screw M4x12:6',
'Socket head cap screw M4x12:6','Socket head cap screw M4x12:6',#42734,
#42741,'Socket head cap screw M4x12:6');
#300=NEXT_ASSEMBLY_USAGE_OCCURRENCE('Socket head cap screw M4x12:7',
'Socket head cap screw M4x12:7','Socket head cap screw M4x12:7',#42734,
#42741,'Socket head cap screw M4x12:7');
#301=NEXT_ASSEMBLY_USAGE_OCCURRENCE('Socket head cap screw M4x12:8',
'Socket head cap screw M4x12:8','Socket head cap screw M4x12:8',#42734,
#42741,'Socket head cap screw M4x12:8');
#302=NEXT_ASSEMBLY_USAGE_OCCURRENCE('Socket head cap screw M6x12:2',
'Socket head cap screw M6x12:2','Socket head cap screw M6x12:2',#42734,
#42742,'Socket head cap screw M6x12:2');
#303=NEXT_ASSEMBLY_USAGE_OCCURRENCE('Socket head cap screw M6x12:3',
'Socket head cap screw M6x12:3','Socket head cap screw M6x12:3',#42734,
#42742,'Socket head cap screw M6x12:3');
#304=NEXT_ASSEMBLY_USAGE_OCCURRENCE('Socket head cap screw M6x12:4',
'Socket head cap screw M6x12:4','Socket head cap screw M6x12:4',#42734,
#42742,'Socket head cap screw M6x12:4');
#305=NEXT_ASSEMBLY_USAGE_OCCURRENCE('Socket head cap screw M6x12:5',
'Socket head cap screw M6x12:5','Socket head cap screw M6x12:5',#42734,
#42742,'Socket head cap screw M6x12:5');
#306=NEXT_ASSEMBLY_USAGE_OCCURRENCE('Socket head cap screw M6x12:6',
'Socket head cap screw M6x12:6','Socket head cap screw M6x12:6',#42734,
#42742,'Socket head cap screw M6x12:6');
#307=NEXT_ASSEMBLY_USAGE_OCCURRENCE('Socket head cap screw M6x12:7',
'Socket head cap screw M6x12:7','Socket head cap screw M6x12:7',#42734,
#42742,'Socket head cap screw M6x12:7');
#308=NEXT_ASSEMBLY_USAGE_OCCURRENCE('Socket head cap screw M6x12:8',
'Socket head cap screw M6x12:8','Socket head cap screw M6x12:8',#42734,
#42742,'Socket head cap screw M6x12:8');
#309=NEXT_ASSEMBLY_USAGE_OCCURRENCE('Hose connection:2',
'Hose connection:2','Hose connection:2',#42734,#42743,
'Hose connection:2');
#310=NEXT_ASSEMBLY_USAGE_OCCURRENCE('Connection face seal:2',
'Connection face seal:2','Connection face seal:2',#42734,#42744,
'Connection face seal:2');
#311=CONICAL_SURFACE('',#11096,1.5,0.785398163397449);
#312=CONICAL_SURFACE('',#11140,2.5,0.785398163397449);
#313=SHAPE_REPRESENTATION_RELATIONSHIP('SRR','None',#42723,#323);
#314=SHAPE_REPRESENTATION_RELATIONSHIP('SRR','None',#42724,#324);
#315=SHAPE_REPRESENTATION_RELATIONSHIP('SRR','None',#42725,#325);
#316=SHAPE_REPRESENTATION_RELATIONSHIP('SRR','None',#42726,#326);
#317=SHAPE_REPRESENTATION_RELATIONSHIP('SRR','None',#42727,#327);
#318=SHAPE_REPRESENTATION_RELATIONSHIP('SRR','None',#42728,#328);
#319=SHAPE_REPRESENTATION_RELATIONSHIP('SRR','None',#42729,#329);
#320=SHAPE_REPRESENTATION_RELATIONSHIP('SRR','None',#42730,#330);
#321=SHAPE_REPRESENTATION_RELATIONSHIP('SRR','None',#42731,#331);
#322=SHAPE_REPRESENTATION_RELATIONSHIP('SRR','None',#42732,#332);
#323=ADVANCED_BREP_SHAPE_REPRESENTATION('',(#343),#42610);
#324=ADVANCED_BREP_SHAPE_REPRESENTATION('',(#344),#42611);
#325=ADVANCED_BREP_SHAPE_REPRESENTATION('',(#345),#42612);
#326=ADVANCED_BREP_SHAPE_REPRESENTATION('',(#346),#42613);
#327=ADVANCED_BREP_SHAPE_REPRESENTATION('',(#347),#42614);
#328=ADVANCED_BREP_SHAPE_REPRESENTATION('',(#348),#42615);
#329=ADVANCED_BREP_SHAPE_REPRESENTATION('',(#349),#42616);
#330=ADVANCED_BREP_SHAPE_REPRESENTATION('',(#350),#42617);
#331=ADVANCED_BREP_SHAPE_REPRESENTATION('',(#351),#42618);
#332=ADVANCED_BREP_SHAPE_REPRESENTATION('',(#352),#42619);
#333=STYLED_ITEM('',(#42782),#343);
#334=STYLED_ITEM('',(#42783),#344);
#335=STYLED_ITEM('',(#42784),#345);
#336=STYLED_ITEM('',(#42785),#346);
#337=STYLED_ITEM('',(#42786),#347);
#338=STYLED_ITEM('',(#42787),#348);
#339=STYLED_ITEM('',(#42784),#349);
#340=STYLED_ITEM('',(#42784),#350);
#341=STYLED_ITEM('',(#42787),#351);
#342=STYLED_ITEM('',(#42788),#352);
#343=MANIFOLD_SOLID_BREP('Body1',#10383);
#344=MANIFOLD_SOLID_BREP('Body1',#10384);
#345=MANIFOLD_SOLID_BREP('Body1',#10385);
#346=MANIFOLD_SOLID_BREP('Body1',#10386);
#347=MANIFOLD_SOLID_BREP('Body1',#10387);
#348=MANIFOLD_SOLID_BREP('Body1',#10388);
#349=MANIFOLD_SOLID_BREP('Body1',#10389);
#350=MANIFOLD_SOLID_BREP('Body1',#10390);
#351=MANIFOLD_SOLID_BREP('Body1',#10391);
#352=MANIFOLD_SOLID_BREP('Body1',#10392);
#353=FACE_BOUND('',#1411,.T.);
#354=FACE_BOUND('',#1415,.T.);
#355=FACE_BOUND('',#1416,.T.);
#356=FACE_BOUND('',#1417,.T.);
#357=FACE_BOUND('',#1418,.T.);
#358=FACE_BOUND('',#1419,.T.);
#359=FACE_BOUND('',#1492,.T.);
#360=FACE_BOUND('',#1493,.T.);
#361=FACE_BOUND('',#1494,.T.);
#362=FACE_BOUND('',#1495,.T.);
#363=FACE_BOUND('',#1496,.T.);
#364=FACE_BOUND('',#1497,.T.);
#365=FACE_BOUND('',#1498,.T.);
#366=FACE_BOUND('',#1499,.T.);
#367=FACE_BOUND('',#1500,.T.);
#368=FACE_BOUND('',#1501,.T.);
#369=FACE_BOUND('',#1502,.T.);
#370=FACE_BOUND('',#1503,.T.);
#371=FACE_BOUND('',#1504,.T.);
#372=FACE_BOUND('',#1505,.T.);
#373=FACE_BOUND('',#1506,.T.);
#374=FACE_BOUND('',#1507,.T.);
#375=FACE_BOUND('',#1508,.T.);
#376=FACE_BOUND('',#1509,.T.);
#377=FACE_BOUND('',#1513,.T.);
#378=FACE_BOUND('',#1516,.T.);
#379=FACE_BOUND('',#1517,.T.);
#380=FACE_BOUND('',#1518,.T.);
#381=FACE_BOUND('',#1519,.T.);
#382=FACE_BOUND('',#1520,.T.);
#383=FACE_BOUND('',#1521,.T.);
#384=FACE_BOUND('',#1522,.T.);
#385=FACE_BOUND('',#1523,.T.);
#386=FACE_BOUND('',#1524,.T.);
#387=FACE_BOUND('',#1525,.T.);
#388=FACE_BOUND('',#1526,.T.);
#389=FACE_BOUND('',#1527,.T.);
#390=FACE_BOUND('',#1528,.T.);
#391=FACE_BOUND('',#1529,.T.);
#392=FACE_BOUND('',#1530,.T.);
#393=FACE_BOUND('',#1531,.T.);
#394=FACE_BOUND('',#1532,.T.);
#395=FACE_BOUND('',#1533,.T.);
#396=FACE_BOUND('',#1537,.T.);
#397=FACE_BOUND('',#1538,.T.);
#398=FACE_BOUND('',#1539,.T.);
#399=FACE_BOUND('',#1540,.T.);
#400=FACE_BOUND('',#1541,.T.);
#401=FACE_BOUND('',#1551,.T.);
#402=FACE_BOUND('',#1552,.T.);
#403=FACE_BOUND('',#1553,.T.);
#404=FACE_BOUND('',#1554,.T.);
#405=FACE_BOUND('',#1556,.T.);
#406=FACE_BOUND('',#1557,.T.);
#407=FACE_BOUND('',#1558,.T.);
#408=FACE_BOUND('',#1559,.T.);
#409=FACE_BOUND('',#1573,.T.);
#410=FACE_BOUND('',#1574,.T.);
#411=FACE_BOUND('',#1575,.T.);
#412=FACE_BOUND('',#1576,.T.);
#413=FACE_BOUND('',#1577,.T.);
#414=FACE_BOUND('',#1579,.T.);
#415=FACE_BOUND('',#1580,.T.);
#416=FACE_BOUND('',#1581,.T.);
#417=FACE_BOUND('',#1582,.T.);
#418=FACE_BOUND('',#1583,.T.);
#419=FACE_BOUND('',#1587,.T.);
#420=FACE_BOUND('',#1589,.T.);
#421=FACE_BOUND('',#1613,.T.);
#422=FACE_BOUND('',#1614,.T.);
#423=FACE_BOUND('',#1615,.T.);
#424=FACE_BOUND('',#1616,.T.);
#425=FACE_BOUND('',#1617,.T.);
#426=FACE_BOUND('',#1618,.T.);
#427=FACE_BOUND('',#1619,.T.);
#428=FACE_BOUND('',#1620,.T.);
#429=FACE_BOUND('',#1621,.T.);
#430=FACE_BOUND('',#1622,.T.);
#431=FACE_BOUND('',#1623,.T.);
#432=FACE_BOUND('',#1624,.T.);
#433=FACE_BOUND('',#1625,.T.);
#434=FACE_BOUND('',#1626,.T.);
#435=FACE_BOUND('',#1627,.T.);
#436=FACE_BOUND('',#1628,.T.);
#437=FACE_BOUND('',#1629,.T.);
#438=FACE_BOUND('',#1630,.T.);
#439=FACE_BOUND('',#1632,.T.);
#440=FACE_BOUND('',#1633,.T.);
#441=FACE_BOUND('',#1634,.T.);
#442=FACE_BOUND('',#1635,.T.);
#443=FACE_BOUND('',#1636,.T.);
#444=FACE_BOUND('',#1637,.T.);
#445=FACE_BOUND('',#1638,.T.);
#446=FACE_BOUND('',#1639,.T.);
#447=FACE_BOUND('',#1640,.T.);
#448=FACE_BOUND('',#1641,.T.);
#449=FACE_BOUND('',#1642,.T.);
#450=FACE_BOUND('',#1643,.T.);
#451=FACE_BOUND('',#1644,.T.);
#452=FACE_BOUND('',#1645,.T.);
#453=FACE_BOUND('',#1646,.T.);
#454=FACE_BOUND('',#1647,.T.);
#455=FACE_BOUND('',#1648,.T.);
#456=FACE_BOUND('',#1649,.T.);
#457=FACE_BOUND('',#1662,.T.);
#458=FACE_BOUND('',#1663,.T.);
#459=FACE_BOUND('',#1664,.T.);
#460=FACE_BOUND('',#1665,.T.);
#461=FACE_BOUND('',#1666,.T.);
#462=FACE_BOUND('',#1667,.T.);
#463=FACE_BOUND('',#1668,.T.);
#464=FACE_BOUND('',#1670,.T.);
#465=FACE_BOUND('',#1671,.T.);
#466=FACE_BOUND('',#1672,.T.);
#467=FACE_BOUND('',#1673,.T.);
#468=FACE_BOUND('',#1674,.T.);
#469=FACE_BOUND('',#1675,.T.);
#470=FACE_BOUND('',#1676,.T.);
#471=FACE_BOUND('',#1722,.T.);
#472=FACE_BOUND('',#1725,.T.);
#473=FACE_BOUND('',#1762,.T.);
#474=FACE_BOUND('',#1765,.T.);
#475=FACE_BOUND('',#1791,.T.);
#476=FACE_BOUND('',#1793,.T.);
#477=FACE_BOUND('',#1797,.T.);
#478=FACE_BOUND('',#1799,.T.);
#479=FACE_BOUND('',#1803,.T.);
#480=FACE_BOUND('',#1805,.T.);
#481=FACE_BOUND('',#1810,.T.);
#482=FACE_BOUND('',#1812,.T.);
#483=FACE_BOUND('',#1815,.T.);
#484=FACE_BOUND('',#1818,.T.);
#485=FACE_BOUND('',#1822,.T.);
#486=FACE_BOUND('',#1824,.T.);
#487=PLANE('',#10813);
#488=PLANE('',#10818);
#489=PLANE('',#10819);
#490=PLANE('',#10822);
#491=PLANE('',#10825);
#492=PLANE('',#10826);
#493=PLANE('',#10828);
#494=PLANE('',#10831);
#495=PLANE('',#10832);
#496=PLANE('',#10834);
#497=PLANE('',#10838);
#498=PLANE('',#10839);
#499=PLANE('',#10841);
#500=PLANE('',#10844);
#501=PLANE('',#10847);
#502=PLANE('',#10850);
#503=PLANE('',#10853);
#504=PLANE('',#10854);
#505=PLANE('',#10855);
#506=PLANE('',#10856);
#507=PLANE('',#10911);
#508=PLANE('',#10912);
#509=PLANE('',#10913);
#510=PLANE('',#10914);
#511=PLANE('',#10915);
#512=PLANE('',#10916);
#513=PLANE('',#10917);
#514=PLANE('',#10918);
#515=PLANE('',#10919);
#516=PLANE('',#10920);
#517=PLANE('',#10934);
#518=PLANE('',#10935);
#519=PLANE('',#10936);
#520=PLANE('',#10937);
#521=PLANE('',#10938);
#522=PLANE('',#10939);
#523=PLANE('',#10953);
#524=PLANE('',#10954);
#525=PLANE('',#10955);
#526=PLANE('',#10956);
#527=PLANE('',#10957);
#528=PLANE('',#10958);
#529=PLANE('',#10959);
#530=PLANE('',#10960);
#531=PLANE('',#10961);
#532=PLANE('',#10962);
#533=PLANE('',#10970);
#534=PLANE('',#10971);
#535=PLANE('',#11027);
#536=PLANE('',#11028);
#537=PLANE('',#11029);
#538=PLANE('',#11030);
#539=PLANE('',#11031);
#540=PLANE('',#11032);
#541=PLANE('',#11055);
#542=PLANE('',#11056);
#543=PLANE('',#11057);
#544=PLANE('',#11058);
#545=PLANE('',#11059);
#546=PLANE('',#11060);
#547=PLANE('',#11102);
#548=PLANE('',#11103);
#549=PLANE('',#11104);
#550=PLANE('',#11105);
#551=PLANE('',#11106);
#552=PLANE('',#11107);
#553=PLANE('',#11108);
#554=PLANE('',#11109);
#555=PLANE('',#11113);
#556=PLANE('',#11114);
#557=PLANE('',#11146);
#558=PLANE('',#11147);
#559=PLANE('',#11148);
#560=PLANE('',#11149);
#561=PLANE('',#11150);
#562=PLANE('',#11151);
#563=PLANE('',#11152);
#564=PLANE('',#11153);
#565=PLANE('',#11157);
#566=PLANE('',#11158);
#567=PLANE('',#11185);
#568=PLANE('',#11188);
#569=PLANE('',#11194);
#570=PLANE('',#11196);
#571=PLANE('',#11202);
#572=PLANE('',#11204);
#573=PLANE('',#11212);
#574=PLANE('',#11214);
#575=PLANE('',#11218);
#576=PLANE('',#11221);
#577=PLANE('',#11229);
#578=PLANE('',#11230);
#579=B_SPLINE_SURFACE_WITH_KNOTS('',3,3,((#23222,#23223,#23224,#23225,#23226,
#23227,#23228,#23229,#23230,#23231,#23232,#23233,#23234,#23235,#23236,#23237,
#23238,#23239,#23240,#23241,#23242,#23243,#23244,#23245,#23246,#23247,#23248,
#23249,#23250,#23251,#23252,#23253,#23254,#23255,#23256,#23257,#23258,#23259,
#23260,#23261,#23262,#23263,#23264,#23265,#23266,#23267,#23268,#23269,#23270,
#23271,#23272,#23273,#23274,#23275,#23276,#23277,#23278,#23279,#23280,#23281,
#23282,#23283,#23284,#23285,#23286,#23287,#23288,#23289,#23290,#23291,#23292,
#23293,#23294,#23295,#23296,#23297,#23298,#23299,#23300,#23301,#23302,#23303,
#23304,#23305,#23306,#23307,#23308,#23309,#23310,#23311,#23312,#23313,#23314,
#23315,#23316,#23317,#23318,#23319,#23320,#23321,#23322,#23323,#23324,#23325,
#23326,#23327,#23328,#23329,#23330),(#23331,#23332,#23333,#23334,#23335,
#23336,#23337,#23338,#23339,#23340,#23341,#23342,#23343,#23344,#23345,#23346,
#23347,#23348,#23349,#23350,#23351,#23352,#23353,#23354,#23355,#23356,#23357,
#23358,#23359,#23360,#23361,#23362,#23363,#23364,#23365,#23366,#23367,#23368,
#23369,#23370,#23371,#23372,#23373,#23374,#23375,#23376,#23377,#23378,#23379,
#23380,#23381,#23382,#23383,#23384,#23385,#23386,#23387,#23388,#23389,#23390,
#23391,#23392,#23393,#23394,#23395,#23396,#23397,#23398,#23399,#23400,#23401,
#23402,#23403,#23404,#23405,#23406,#23407,#23408,#23409,#23410,#23411,#23412,
#23413,#23414,#23415,#23416,#23417,#23418,#23419,#23420,#23421,#23422,#23423,
#23424,#23425,#23426,#23427,#23428,#23429,#23430,#23431,#23432,#23433,#23434,
#23435,#23436,#23437,#23438,#23439),(#23440,#23441,#23442,#23443,#23444,
#23445,#23446,#23447,#23448,#23449,#23450,#23451,#23452,#23453,#23454,#23455,
#23456,#23457,#23458,#23459,#23460,#23461,#23462,#23463,#23464,#23465,#23466,
#23467,#23468,#23469,#23470,#23471,#23472,#23473,#23474,#23475,#23476,#23477,
#23478,#23479,#23480,#23481,#23482,#23483,#23484,#23485,#23486,#23487,#23488,
#23489,#23490,#23491,#23492,#23493,#23494,#23495,#23496,#23497,#23498,#23499,
#23500,#23501,#23502,#23503,#23504,#23505,#23506,#23507,#23508,#23509,#23510,
#23511,#23512,#23513,#23514,#23515,#23516,#23517,#23518,#23519,#23520,#23521,
#23522,#23523,#23524,#23525,#23526,#23527,#23528,#23529,#23530,#23531,#23532,
#23533,#23534,#23535,#23536,#23537,#23538,#23539,#23540,#23541,#23542,#23543,
#23544,#23545,#23546,#23547,#23548),(#23549,#23550,#23551,#23552,#23553,
#23554,#23555,#23556,#23557,#23558,#23559,#23560,#23561,#23562,#23563,#23564,
#23565,#23566,#23567,#23568,#23569,#23570,#23571,#23572,#23573,#23574,#23575,
#23576,#23577,#23578,#23579,#23580,#23581,#23582,#23583,#23584,#23585,#23586,
#23587,#23588,#23589,#23590,#23591,#23592,#23593,#23594,#23595,#23596,#23597,
#23598,#23599,#23600,#23601,#23602,#23603,#23604,#23605,#23606,#23607,#23608,
#23609,#23610,#23611,#23612,#23613,#23614,#23615,#23616,#23617,#23618,#23619,
#23620,#23621,#23622,#23623,#23624,#23625,#23626,#23627,#23628,#23629,#23630,
#23631,#23632,#23633,#23634,#23635,#23636,#23637,#23638,#23639,#23640,#23641,
#23642,#23643,#23644,#23645,#23646,#23647,#23648,#23649,#23650,#23651,#23652,
#23653,#23654,#23655,#23656,#23657)),.UNSPECIFIED.,.F.,.F.,.F.,(4,4),(4,
1,1,1,1,1,1,1,1,1,1,1,1,1,1,1,1,1,1,1,1,1,1,1,1,1,1,1,1,1,1,1,1,1,1,1,1,
1,1,1,1,1,1,1,1,1,1,1,1,1,1,1,1,1,1,1,1,1,1,1,1,1,1,1,1,1,1,1,1,1,1,1,1,
1,1,1,1,1,1,1,1,1,1,1,1,1,1,1,1,1,1,1,1,1,1,1,1,1,1,1,1,1,1,1,1,1,4),(0.,
0.0968216401431001),(11.8468968665462,12.3402299811373,12.8335630957283,
13.3268962103193,13.8202293249104,14.3135624395014,14.8068955540925,15.3002286686835,
15.7935617832746,16.2868948978656,16.7802280124566,17.2735611270477,17.7668942416387,
18.2602273562298,18.7535604708208,19.2468935854119,19.7402267000029,20.2335598145939,
20.726892929185,21.220226043776,21.7135591583671,22.2068922729581,22.7002253875492,
23.1935585021402,23.6868916167312,24.1802247313223,24.6735578459133,25.1668909605044,
25.6602240750954,26.1535571896865,26.6468903042775,27.1402234188686,27.6335565334596,
28.1268896480506,28.6202227626417,29.1135558772327,29.6068889918238,30.1002221064148,
30.5935552210059,31.0868883355969,31.5802214501879,32.073554564779,32.56688767937,
33.0602207939611,33.5535539085521,34.0468870231432,34.5402201377342,35.0335532523252,
35.5268863669163,36.0202194815073,36.5135525960984,37.0068857106894,37.5002188252805,
37.9935519398715,38.4868850544625,38.9802181690536,39.4735512836446,39.9668843982357,
40.4602175128267,40.9535506274178,41.4468837420088,41.9402168565998,42.4335499711909,
42.9268830857819,43.420216200373,43.913549314964,44.4068824295551,44.9002155441461,
45.3935486587371,45.8868817733282,46.3802148879192,46.8735480025103,47.3668811171013,
47.8602142316924,48.3535473462834,48.8468804608745,49.3402135754655,49.8335466900565,
50.3268798046476,50.8202129192386,51.3135460338297,51.8068791484207,52.3002122630117,
52.7935453776028,53.2868784921938,53.7802116067849,54.2735447213759,54.766877835967,
55.260210950558,55.7535440651491,56.2468771797401,56.7402102943311,57.2335434089222,
57.7268765235132,58.2202096381043,58.7135427526953,59.2068758672864,59.7002089818774,
60.1935420964684,60.6868752110595,61.1802083256505,61.6735414402416,62.1668745548326,
62.6602076694237,63.1535407840147,63.6468738986057,64.1402070131968),
 .UNSPECIFIED.);
#580=B_SPLINE_SURFACE_WITH_KNOTS('',3,3,((#23931,#23932,#23933,#23934,#23935,
#23936,#23937,#23938,#23939,#23940,#23941,#23942,#23943,#23944,#23945,#23946,
#23947,#23948,#23949,#23950,#23951,#23952,#23953,#23954,#23955,#23956,#23957,
#23958,#23959,#23960,#23961,#23962,#23963,#23964,#23965,#23966,#23967,#23968,
#23969,#23970,#23971,#23972,#23973,#23974,#23975,#23976,#23977,#23978,#23979,
#23980,#23981,#23982,#23983,#23984,#23985,#23986,#23987,#23988,#23989,#23990,
#23991,#23992,#23993,#23994,#23995,#23996,#23997,#23998,#23999,#24000,#24001,
#24002,#24003,#24004,#24005,#24006,#24007,#24008,#24009,#24010,#24011,#24012,
#24013,#24014,#24015,#24016,#24017,#24018,#24019,#24020,#24021,#24022,#24023,
#24024,#24025,#24026,#24027,#24028,#24029,#24030,#24031,#24032,#24033,#24034,
#24035,#24036,#24037,#24038,#24039),(#24040,#24041,#24042,#24043,#24044,
#24045,#24046,#24047,#24048,#24049,#24050,#24051,#24052,#24053,#24054,#24055,
#24056,#24057,#24058,#24059,#24060,#24061,#24062,#24063,#24064,#24065,#24066,
#24067,#24068,#24069,#24070,#24071,#24072,#24073,#24074,#24075,#24076,#24077,
#24078,#24079,#24080,#24081,#24082,#24083,#24084,#24085,#24086,#24087,#24088,
#24089,#24090,#24091,#24092,#24093,#24094,#24095,#24096,#24097,#24098,#24099,
#24100,#24101,#24102,#24103,#24104,#24105,#24106,#24107,#24108,#24109,#24110,
#24111,#24112,#24113,#24114,#24115,#24116,#24117,#24118,#24119,#24120,#24121,
#24122,#24123,#24124,#24125,#24126,#24127,#24128,#24129,#24130,#24131,#24132,
#24133,#24134,#24135,#24136,#24137,#24138,#24139,#24140,#24141,#24142,#24143,
#24144,#24145,#24146,#24147,#24148),(#24149,#24150,#24151,#24152,#24153,
#24154,#24155,#24156,#24157,#24158,#24159,#24160,#24161,#24162,#24163,#24164,
#24165,#24166,#24167,#24168,#24169,#24170,#24171,#24172,#24173,#24174,#24175,
#24176,#24177,#24178,#24179,#24180,#24181,#24182,#24183,#24184,#24185,#24186,
#24187,#24188,#24189,#24190,#24191,#24192,#24193,#24194,#24195,#24196,#24197,
#24198,#24199,#24200,#24201,#24202,#24203,#24204,#24205,#24206,#24207,#24208,
#24209,#24210,#24211,#24212,#24213,#24214,#24215,#24216,#24217,#24218,#24219,
#24220,#24221,#24222,#24223,#24224,#24225,#24226,#24227,#24228,#24229,#24230,
#24231,#24232,#24233,#24234,#24235,#24236,#24237,#24238,#24239,#24240,#24241,
#24242,#24243,#24244,#24245,#24246,#24247,#24248,#24249,#24250,#24251,#24252,
#24253,#24254,#24255,#24256,#24257),(#24258,#24259,#24260,#24261,#24262,
#24263,#24264,#24265,#24266,#24267,#24268,#24269,#24270,#24271,#24272,#24273,
#24274,#24275,#24276,#24277,#24278,#24279,#24280,#24281,#24282,#24283,#24284,
#24285,#24286,#24287,#24288,#24289,#24290,#24291,#24292,#24293,#24294,#24295,
#24296,#24297,#24298,#24299,#24300,#24301,#24302,#24303,#24304,#24305,#24306,
#24307,#24308,#24309,#24310,#24311,#24312,#24313,#24314,#24315,#24316,#24317,
#24318,#24319,#24320,#24321,#24322,#24323,#24324,#24325,#24326,#24327,#24328,
#24329,#24330,#24331,#24332,#24333,#24334,#24335,#24336,#24337,#24338,#24339,
#24340,#24341,#24342,#24343,#24344,#24345,#24346,#24347,#24348,#24349,#24350,
#24351,#24352,#24353,#24354,#24355,#24356,#24357,#24358,#24359,#24360,#24361,
#24362,#24363,#24364,#24365,#24366)),.UNSPECIFIED.,.F.,.F.,.F.,(4,4),(4,
1,1,1,1,1,1,1,1,1,1,1,1,1,1,1,1,1,1,1,1,1,1,1,1,1,1,1,1,1,1,1,1,1,1,1,1,
1,1,1,1,1,1,1,1,1,1,1,1,1,1,1,1,1,1,1,1,1,1,1,1,1,1,1,1,1,1,1,1,1,1,1,1,
1,1,1,1,1,1,1,1,1,1,1,1,1,1,1,1,1,1,1,1,1,1,1,1,1,1,1,1,1,1,1,1,1,4),(0.,
0.0968216401431001),(14.399609326548,14.892942441139,15.3862755557301,15.8796086703211,
16.3729417849122,16.8662748995032,17.3596080140942,17.8529411286853,18.3462742432763,
18.8396073578674,19.3329404724584,19.8262735870495,20.3196067016405,20.8129398162316,
21.3062729308226,21.7996060454136,22.2929391600047,22.7862722745957,23.2796053891868,
23.7729385037778,24.2662716183689,24.7596047329599,25.2529378475509,25.746270962142,
26.239604076733,26.7329371913241,27.2262703059151,27.7196034205062,28.2129365350972,
28.7062696496882,29.1996027642793,29.6929358788703,30.1862689934614,30.6796021080524,
31.1729352226435,31.6662683372345,32.1596014518255,32.6529345664166,33.1462676810076,
33.6396007955987,34.1329339101897,34.6262670247808,35.1196001393718,35.6129332539629,
36.1062663685539,36.5995994831449,37.092932597736,37.586265712327,38.0795988269181,
38.5729319415091,39.0662650561001,39.5595981706912,40.0529312852822,40.5462643998733,
41.0395975144643,41.5329306290554,42.0262637436464,42.5195968582374,43.0129299728285,
43.5062630874195,43.9995962020106,44.4929293166016,44.9862624311927,45.4795955457837,
45.9729286603748,46.4662617749658,46.9595948895568,47.4529280041479,47.9462611187389,
48.43959423333,48.932927347921,49.4262604625121,49.9195935771031,50.4129266916941,
50.9062598062852,51.3995929208762,51.8929260354673,52.3862591500583,52.8795922646494,
53.3729253792404,53.8662584938314,54.3595916084225,54.8529247230135,55.3462578376046,
55.8395909521956,56.3329240667867,56.8262571813777,57.3195902959688,57.8129234105598,
58.3062565251508,58.7995896397419,59.2929227543329,59.786255868924,60.279588983515,
60.7729220981061,61.2662552126971,61.7595883272881,62.2529214418792,62.7462545564702,
63.2395876710613,63.7329207856523,64.2262539002434,64.7195870148344,65.2129201294254,
65.7062532440165,66.1995863586075,66.6929194731986),.UNSPECIFIED.);
#581=B_SPLINE_SURFACE_WITH_KNOTS('',3,3,((#25611,#25612,#25613,#25614,#25615,
#25616,#25617,#25618,#25619,#25620,#25621,#25622,#25623,#25624,#25625,#25626,
#25627,#25628,#25629,#25630,#25631,#25632,#25633,#25634,#25635,#25636,#25637,
#25638,#25639,#25640,#25641,#25642,#25643,#25644,#25645,#25646,#25647,#25648,
#25649,#25650,#25651,#25652,#25653,#25654,#25655,#25656,#25657,#25658,#25659,
#25660,#25661,#25662,#25663,#25664,#25665,#25666,#25667,#25668,#25669,#25670,
#25671,#25672,#25673,#25674,#25675,#25676,#25677,#25678,#25679,#25680,#25681,
#25682,#25683,#25684,#25685,#25686,#25687,#25688,#25689,#25690,#25691,#25692,
#25693,#25694,#25695,#25696,#25697,#25698,#25699,#25700,#25701,#25702,#25703,
#25704,#25705,#25706,#25707,#25708,#25709,#25710),(#25711,#25712,#25713,
#25714,#25715,#25716,#25717,#25718,#25719,#25720,#25721,#25722,#25723,#25724,
#25725,#25726,#25727,#25728,#25729,#25730,#25731,#25732,#25733,#25734,#25735,
#25736,#25737,#25738,#25739,#25740,#25741,#25742,#25743,#25744,#25745,#25746,
#25747,#25748,#25749,#25750,#25751,#25752,#25753,#25754,#25755,#25756,#25757,
#25758,#25759,#25760,#25761,#25762,#25763,#25764,#25765,#25766,#25767,#25768,
#25769,#25770,#25771,#25772,#25773,#25774,#25775,#25776,#25777,#25778,#25779,
#25780,#25781,#25782,#25783,#25784,#25785,#25786,#25787,#25788,#25789,#25790,
#25791,#25792,#25793,#25794,#25795,#25796,#25797,#25798,#25799,#25800,#25801,
#25802,#25803,#25804,#25805,#25806,#25807,#25808,#25809,#25810),(#25811,
#25812,#25813,#25814,#25815,#25816,#25817,#25818,#25819,#25820,#25821,#25822,
#25823,#25824,#25825,#25826,#25827,#25828,#25829,#25830,#25831,#25832,#25833,
#25834,#25835,#25836,#25837,#25838,#25839,#25840,#25841,#25842,#25843,#25844,
#25845,#25846,#25847,#25848,#25849,#25850,#25851,#25852,#25853,#25854,#25855,
#25856,#25857,#25858,#25859,#25860,#25861,#25862,#25863,#25864,#25865,#25866,
#25867,#25868,#25869,#25870,#25871,#25872,#25873,#25874,#25875,#25876,#25877,
#25878,#25879,#25880,#25881,#25882,#25883,#25884,#25885,#25886,#25887,#25888,
#25889,#25890,#25891,#25892,#25893,#25894,#25895,#25896,#25897,#25898,#25899,
#25900,#25901,#25902,#25903,#25904,#25905,#25906,#25907,#25908,#25909,#25910),
(#25911,#25912,#25913,#25914,#25915,#25916,#25917,#25918,#25919,#25920,
#25921,#25922,#25923,#25924,#25925,#25926,#25927,#25928,#25929,#25930,#25931,
#25932,#25933,#25934,#25935,#25936,#25937,#25938,#25939,#25940,#25941,#25942,
#25943,#25944,#25945,#25946,#25947,#25948,#25949,#25950,#25951,#25952,#25953,
#25954,#25955,#25956,#25957,#25958,#25959,#25960,#25961,#25962,#25963,#25964,
#25965,#25966,#25967,#25968,#25969,#25970,#25971,#25972,#25973,#25974,#25975,
#25976,#25977,#25978,#25979,#25980,#25981,#25982,#25983,#25984,#25985,#25986,
#25987,#25988,#25989,#25990,#25991,#25992,#25993,#25994,#25995,#25996,#25997,
#25998,#25999,#26000,#26001,#26002,#26003,#26004,#26005,#26006,#26007,#26008,
#26009,#26010)),.UNSPECIFIED.,.F.,.F.,.F.,(4,4),(4,1,1,1,1,1,1,1,1,1,1,
1,1,1,1,1,1,1,1,1,1,1,1,1,1,1,1,1,1,1,1,1,1,1,1,1,1,1,1,1,1,1,1,1,1,1,1,
1,1,1,1,1,1,1,1,1,1,1,1,1,1,1,1,1,1,1,1,1,1,1,1,1,1,1,1,1,1,1,1,1,1,1,1,
1,1,1,1,1,1,1,1,1,1,1,1,1,1,4),(0.,0.0642013499338866),(11.8589888623077,
12.8514087025214,13.843828542735,14.8362483829486,15.8286682231623,16.8210880633759,
17.8135079035895,18.8059277438032,19.7983475840168,20.7907674242304,21.7831872644441,
22.7756071046577,23.7680269448713,24.7604467850849,25.7528666252986,26.7452864655122,
27.7377063057258,28.7301261459395,29.7225459861531,30.7149658263667,31.7073856665804,
32.699805506794,33.6922253470076,34.6846451872213,35.6770650274349,36.6694848676485,
37.6619047078622,38.6543245480758,39.6467443882894,40.639164228503,41.6315840687167,
42.6240039089303,43.6164237491439,44.6088435893576,45.6012634295712,46.5936832697848,
47.5861031099985,48.5785229502121,49.5709427904257,50.5633626306394,51.555782470853,
52.5482023110666,53.5406221512803,54.5330419914939,55.5254618317075,56.5178816719212,
57.5103015121348,58.5027213523484,59.4951411925621,60.4875610327757,61.4799808729893,
62.4724007132029,63.4648205534166,64.4572403936302,65.4496602338438,66.4420800740575,
67.4344999142711,68.4269197544847,69.4193395946984,70.411759434912,71.4041792751256,
72.3965991153393,73.3890189555529,74.3814387957665,75.3738586359802,76.3662784761938,
77.3586983164074,78.3511181566211,79.3435379968347,80.3359578370483,81.328377677262,
82.3207975174756,83.3132173576892,84.3056371979029,85.2980570381165,86.2904768783301,
87.2828967185437,88.2753165587574,89.267736398971,90.2601562391846,91.2525760793983,
92.2449959196119,93.2374157598255,94.2298356000392,95.2222554402528,96.2146752804664,
97.2070951206801,98.1995149608937,99.1919348011073,100.184354641321,101.176774481535,
102.169194321748,103.161614161962,104.154034002175,105.146453842389,106.138873682603,
107.131293522816,108.12371336303),.UNSPECIFIED.);
#582=B_SPLINE_SURFACE_WITH_KNOTS('',3,3,((#26036,#26037,#26038,#26039,#26040,
#26041,#26042,#26043,#26044,#26045,#26046,#26047,#26048,#26049,#26050,#26051,
#26052,#26053,#26054,#26055,#26056,#26057,#26058,#26059,#26060,#26061,#26062,
#26063,#26064,#26065,#26066,#26067,#26068,#26069,#26070,#26071,#26072,#26073,
#26074,#26075,#26076,#26077,#26078,#26079,#26080,#26081,#26082,#26083,#26084,
#26085,#26086,#26087,#26088,#26089,#26090,#26091,#26092,#26093,#26094,#26095,
#26096,#26097,#26098,#26099,#26100,#26101,#26102,#26103,#26104,#26105,#26106,
#26107,#26108,#26109,#26110,#26111,#26112,#26113,#26114,#26115,#26116,#26117,
#26118,#26119,#26120,#26121,#26122,#26123,#26124,#26125,#26126,#26127,#26128,
#26129,#26130,#26131,#26132,#26133,#26134,#26135),(#26136,#26137,#26138,
#26139,#26140,#26141,#26142,#26143,#26144,#26145,#26146,#26147,#26148,#26149,
#26150,#26151,#26152,#26153,#26154,#26155,#26156,#26157,#26158,#26159,#26160,
#26161,#26162,#26163,#26164,#26165,#26166,#26167,#26168,#26169,#26170,#26171,
#26172,#26173,#26174,#26175,#26176,#26177,#26178,#26179,#26180,#26181,#26182,
#26183,#26184,#26185,#26186,#26187,#26188,#26189,#26190,#26191,#26192,#26193,
#26194,#26195,#26196,#26197,#26198,#26199,#26200,#26201,#26202,#26203,#26204,
#26205,#26206,#26207,#26208,#26209,#26210,#26211,#26212,#26213,#26214,#26215,
#26216,#26217,#26218,#26219,#26220,#26221,#26222,#26223,#26224,#26225,#26226,
#26227,#26228,#26229,#26230,#26231,#26232,#26233,#26234,#26235),(#26236,
#26237,#26238,#26239,#26240,#26241,#26242,#26243,#26244,#26245,#26246,#26247,
#26248,#26249,#26250,#26251,#26252,#26253,#26254,#26255,#26256,#26257,#26258,
#26259,#26260,#26261,#26262,#26263,#26264,#26265,#26266,#26267,#26268,#26269,
#26270,#26271,#26272,#26273,#26274,#26275,#26276,#26277,#26278,#26279,#26280,
#26281,#26282,#26283,#26284,#26285,#26286,#26287,#26288,#26289,#26290,#26291,
#26292,#26293,#26294,#26295,#26296,#26297,#26298,#26299,#26300,#26301,#26302,
#26303,#26304,#26305,#26306,#26307,#26308,#26309,#26310,#26311,#26312,#26313,
#26314,#26315,#26316,#26317,#26318,#26319,#26320,#26321,#26322,#26323,#26324,
#26325,#26326,#26327,#26328,#26329,#26330,#26331,#26332,#26333,#26334,#26335),
(#26336,#26337,#26338,#26339,#26340,#26341,#26342,#26343,#26344,#26345,
#26346,#26347,#26348,#26349,#26350,#26351,#26352,#26353,#26354,#26355,#26356,
#26357,#26358,#26359,#26360,#26361,#26362,#26363,#26364,#26365,#26366,#26367,
#26368,#26369,#26370,#26371,#26372,#26373,#26374,#26375,#26376,#26377,#26378,
#26379,#26380,#26381,#26382,#26383,#26384,#26385,#26386,#26387,#26388,#26389,
#26390,#26391,#26392,#26393,#26394,#26395,#26396,#26397,#26398,#26399,#26400,
#26401,#26402,#26403,#26404,#26405,#26406,#26407,#26408,#26409,#26410,#26411,
#26412,#26413,#26414,#26415,#26416,#26417,#26418,#26419,#26420,#26421,#26422,
#26423,#26424,#26425,#26426,#26427,#26428,#26429,#26430,#26431,#26432,#26433,
#26434,#26435)),.UNSPECIFIED.,.F.,.F.,.F.,(4,4),(4,1,1,1,1,1,1,1,1,1,1,
1,1,1,1,1,1,1,1,1,1,1,1,1,1,1,1,1,1,1,1,1,1,1,1,1,1,1,1,1,1,1,1,1,1,1,1,
1,1,1,1,1,1,1,1,1,1,1,1,1,1,1,1,1,1,1,1,1,1,1,1,1,1,1,1,1,1,1,1,1,1,1,1,
1,1,1,1,1,1,1,1,1,1,1,1,1,1,4),(0.,0.0642013499338862),(14.3984001269718,
15.3908199671854,16.383239807399,17.3756596476127,18.3680794878263,19.3604993280399,
20.3529191682536,21.3453390084672,22.3377588486808,23.3301786888945,24.3225985291081,
25.3150183693217,26.3074382095353,27.299858049749,28.2922778899626,29.2846977301762,
30.2771175703899,31.2695374106035,32.2619572508171,33.2543770910308,34.2467969312444,
35.239216771458,36.2316366116717,37.2240564518853,38.2164762920989,39.2088961323126,
40.2013159725262,41.1937358127398,42.1861556529534,43.1785754931671,44.1709953333807,
45.1634151735943,46.155835013808,47.1482548540216,48.1406746942352,49.1330945344489,
50.1255143746625,51.1179342148761,52.1103540550898,53.1027738953034,54.095193735517,
55.0876135757306,56.0800334159443,57.0724532561579,58.0648730963715,59.0572929365852,
60.0497127767988,61.0421326170124,62.0345524572261,63.0269722974397,64.0193921376533,
65.011811977867,66.0042318180806,66.9966516582942,67.9890714985079,68.9814913387215,
69.9739111789351,70.9663310191488,71.9587508593624,72.951170699576,73.9435905397896,
74.9360103800033,75.9284302202169,76.9208500604305,77.9132699006442,78.9056897408578,
79.8981095810714,80.8905294212851,81.8829492614987,82.8753691017123,83.867788941926,
84.8602087821396,85.8526286223532,86.8450484625669,87.8374683027805,88.8298881429941,
89.8223079832078,90.8147278234214,91.807147663635,92.7995675038486,93.7919873440623,
94.7844071842759,95.7768270244895,96.7692468647032,97.7616667049168,98.7540865451304,
99.7465063853441,100.738926225558,101.731346065771,102.723765905985,103.716185746199,
104.708605586412,105.701025426626,106.693445266839,107.685865107053,108.678284947267,
109.67070478748,110.663124627694),.UNSPECIFIED.);
#583=B_SPLINE_SURFACE_WITH_KNOTS('',3,3,((#26670,#26671,#26672,#26673,#26674,
#26675,#26676,#26677,#26678,#26679,#26680,#26681,#26682,#26683,#26684,#26685,
#26686,#26687,#26688,#26689,#26690,#26691,#26692,#26693,#26694,#26695,#26696,
#26697,#26698,#26699,#26700,#26701,#26702,#26703,#26704,#26705,#26706,#26707,
#26708,#26709,#26710,#26711,#26712,#26713,#26714,#26715,#26716,#26717,#26718,
#26719,#26720,#26721,#26722,#26723,#26724,#26725,#26726,#26727,#26728,#26729,
#26730,#26731,#26732,#26733,#26734,#26735,#26736,#26737,#26738,#26739,#26740,
#26741,#26742,#26743,#26744,#26745,#26746,#26747,#26748,#26749,#26750,#26751,
#26752,#26753,#26754,#26755,#26756,#26757,#26758,#26759,#26760,#26761,#26762,
#26763,#26764,#26765,#26766,#26767,#26768,#26769),(#26770,#26771,#26772,
#26773,#26774,#26775,#26776,#26777,#26778,#26779,#26780,#26781,#26782,#26783,
#26784,#26785,#26786,#26787,#26788,#26789,#26790,#26791,#26792,#26793,#26794,
#26795,#26796,#26797,#26798,#26799,#26800,#26801,#26802,#26803,#26804,#26805,
#26806,#26807,#26808,#26809,#26810,#26811,#26812,#26813,#26814,#26815,#26816,
#26817,#26818,#26819,#26820,#26821,#26822,#26823,#26824,#26825,#26826,#26827,
#26828,#26829,#26830,#26831,#26832,#26833,#26834,#26835,#26836,#26837,#26838,
#26839,#26840,#26841,#26842,#26843,#26844,#26845,#26846,#26847,#26848,#26849,
#26850,#26851,#26852,#26853,#26854,#26855,#26856,#26857,#26858,#26859,#26860,
#26861,#26862,#26863,#26864,#26865,#26866,#26867,#26868,#26869),(#26870,
#26871,#26872,#26873,#26874,#26875,#26876,#26877,#26878,#26879,#26880,#26881,
#26882,#26883,#26884,#26885,#26886,#26887,#26888,#26889,#26890,#26891,#26892,
#26893,#26894,#26895,#26896,#26897,#26898,#26899,#26900,#26901,#26902,#26903,
#26904,#26905,#26906,#26907,#26908,#26909,#26910,#26911,#26912,#26913,#26914,
#26915,#26916,#26917,#26918,#26919,#26920,#26921,#26922,#26923,#26924,#26925,
#26926,#26927,#26928,#26929,#26930,#26931,#26932,#26933,#26934,#26935,#26936,
#26937,#26938,#26939,#26940,#26941,#26942,#26943,#26944,#26945,#26946,#26947,
#26948,#26949,#26950,#26951,#26952,#26953,#26954,#26955,#26956,#26957,#26958,
#26959,#26960,#26961,#26962,#26963,#26964,#26965,#26966,#26967,#26968,#26969),
(#26970,#26971,#26972,#26973,#26974,#26975,#26976,#26977,#26978,#26979,
#26980,#26981,#26982,#26983,#26984,#26985,#26986,#26987,#26988,#26989,#26990,
#26991,#26992,#26993,#26994,#26995,#26996,#26997,#26998,#26999,#27000,#27001,
#27002,#27003,#27004,#27005,#27006,#27007,#27008,#27009,#27010,#27011,#27012,
#27013,#27014,#27015,#27016,#27017,#27018,#27019,#27020,#27021,#27022,#27023,
#27024,#27025,#27026,#27027,#27028,#27029,#27030,#27031,#27032,#27033,#27034,
#27035,#27036,#27037,#27038,#27039,#27040,#27041,#27042,#27043,#27044,#27045,
#27046,#27047,#27048,#27049,#27050,#27051,#27052,#27053,#27054,#27055,#27056,
#27057,#27058,#27059,#27060,#27061,#27062,#27063,#27064,#27065,#27066,#27067,
#27068,#27069)),.UNSPECIFIED.,.F.,.F.,.F.,(4,4),(4,1,1,1,1,1,1,1,1,1,1,
1,1,1,1,1,1,1,1,1,1,1,1,1,1,1,1,1,1,1,1,1,1,1,1,1,1,1,1,1,1,1,1,1,1,1,1,
1,1,1,1,1,1,1,1,1,1,1,1,1,1,1,1,1,1,1,1,1,1,1,1,1,1,1,1,1,1,1,1,1,1,1,1,
1,1,1,1,1,1,1,1,1,1,1,1,1,1,4),(0.,0.0642013499338866),(11.8589888623077,
12.8514087025214,13.843828542735,14.8362483829486,15.8286682231623,16.8210880633759,
17.8135079035895,18.8059277438032,19.7983475840168,20.7907674242304,21.7831872644441,
22.7756071046577,23.7680269448713,24.7604467850849,25.7528666252986,26.7452864655122,
27.7377063057258,28.7301261459395,29.7225459861531,30.7149658263667,31.7073856665804,
32.699805506794,33.6922253470076,34.6846451872213,35.6770650274349,36.6694848676485,
37.6619047078622,38.6543245480758,39.6467443882894,40.639164228503,41.6315840687167,
42.6240039089303,43.6164237491439,44.6088435893576,45.6012634295712,46.5936832697848,
47.5861031099985,48.5785229502121,49.5709427904257,50.5633626306394,51.555782470853,
52.5482023110666,53.5406221512803,54.5330419914939,55.5254618317075,56.5178816719212,
57.5103015121348,58.5027213523484,59.4951411925621,60.4875610327757,61.4799808729893,
62.4724007132029,63.4648205534166,64.4572403936302,65.4496602338438,66.4420800740575,
67.4344999142711,68.4269197544847,69.4193395946984,70.411759434912,71.4041792751256,
72.3965991153393,73.3890189555529,74.3814387957665,75.3738586359802,76.3662784761938,
77.3586983164074,78.3511181566211,79.3435379968347,80.3359578370483,81.328377677262,
82.3207975174756,83.3132173576892,84.3056371979029,85.2980570381165,86.2904768783301,
87.2828967185437,88.2753165587574,89.267736398971,90.2601562391846,91.2525760793983,
92.2449959196119,93.2374157598255,94.2298356000392,95.2222554402528,96.2146752804664,
97.2070951206801,98.1995149608937,99.1919348011073,100.184354641321,101.176774481535,
102.169194321748,103.161614161962,104.154034002175,105.146453842389,106.138873682603,
107.131293522816,108.12371336303),.UNSPECIFIED.);
#584=B_SPLINE_SURFACE_WITH_KNOTS('',3,3,((#27095,#27096,#27097,#27098,#27099,
#27100,#27101,#27102,#27103,#27104,#27105,#27106,#27107,#27108,#27109,#27110,
#27111,#27112,#27113,#27114,#27115,#27116,#27117,#27118,#27119,#27120,#27121,
#27122,#27123,#27124,#27125,#27126,#27127,#27128,#27129,#27130,#27131,#27132,
#27133,#27134,#27135,#27136,#27137,#27138,#27139,#27140,#27141,#27142,#27143,
#27144,#27145,#27146,#27147,#27148,#27149,#27150,#27151,#27152,#27153,#27154,
#27155,#27156,#27157,#27158,#27159,#27160,#27161,#27162,#27163,#27164,#27165,
#27166,#27167,#27168,#27169,#27170,#27171,#27172,#27173,#27174,#27175,#27176,
#27177,#27178,#27179,#27180,#27181,#27182,#27183,#27184,#27185,#27186,#27187,
#27188,#27189,#27190,#27191,#27192,#27193,#27194),(#27195,#27196,#27197,
#27198,#27199,#27200,#27201,#27202,#27203,#27204,#27205,#27206,#27207,#27208,
#27209,#27210,#27211,#27212,#27213,#27214,#27215,#27216,#27217,#27218,#27219,
#27220,#27221,#27222,#27223,#27224,#27225,#27226,#27227,#27228,#27229,#27230,
#27231,#27232,#27233,#27234,#27235,#27236,#27237,#27238,#27239,#27240,#27241,
#27242,#27243,#27244,#27245,#27246,#27247,#27248,#27249,#27250,#27251,#27252,
#27253,#27254,#27255,#27256,#27257,#27258,#27259,#27260,#27261,#27262,#27263,
#27264,#27265,#27266,#27267,#27268,#27269,#27270,#27271,#27272,#27273,#27274,
#27275,#27276,#27277,#27278,#27279,#27280,#27281,#27282,#27283,#27284,#27285,
#27286,#27287,#27288,#27289,#27290,#27291,#27292,#27293,#27294),(#27295,
#27296,#27297,#27298,#27299,#27300,#27301,#27302,#27303,#27304,#27305,#27306,
#27307,#27308,#27309,#27310,#27311,#27312,#27313,#27314,#27315,#27316,#27317,
#27318,#27319,#27320,#27321,#27322,#27323,#27324,#27325,#27326,#27327,#27328,
#27329,#27330,#27331,#27332,#27333,#27334,#27335,#27336,#27337,#27338,#27339,
#27340,#27341,#27342,#27343,#27344,#27345,#27346,#27347,#27348,#27349,#27350,
#27351,#27352,#27353,#27354,#27355,#27356,#27357,#27358,#27359,#27360,#27361,
#27362,#27363,#27364,#27365,#27366,#27367,#27368,#27369,#27370,#27371,#27372,
#27373,#27374,#27375,#27376,#27377,#27378,#27379,#27380,#27381,#27382,#27383,
#27384,#27385,#27386,#27387,#27388,#27389,#27390,#27391,#27392,#27393,#27394),
(#27395,#27396,#27397,#27398,#27399,#27400,#27401,#27402,#27403,#27404,
#27405,#27406,#27407,#27408,#27409,#27410,#27411,#27412,#27413,#27414,#27415,
#27416,#27417,#27418,#27419,#27420,#27421,#27422,#27423,#27424,#27425,#27426,
#27427,#27428,#27429,#27430,#27431,#27432,#27433,#27434,#27435,#27436,#27437,
#27438,#27439,#27440,#27441,#27442,#27443,#27444,#27445,#27446,#27447,#27448,
#27449,#27450,#27451,#27452,#27453,#27454,#27455,#27456,#27457,#27458,#27459,
#27460,#27461,#27462,#27463,#27464,#27465,#27466,#27467,#27468,#27469,#27470,
#27471,#27472,#27473,#27474,#27475,#27476,#27477,#27478,#27479,#27480,#27481,
#27482,#27483,#27484,#27485,#27486,#27487,#27488,#27489,#27490,#27491,#27492,
#27493,#27494)),.UNSPECIFIED.,.F.,.F.,.F.,(4,4),(4,1,1,1,1,1,1,1,1,1,1,
1,1,1,1,1,1,1,1,1,1,1,1,1,1,1,1,1,1,1,1,1,1,1,1,1,1,1,1,1,1,1,1,1,1,1,1,
1,1,1,1,1,1,1,1,1,1,1,1,1,1,1,1,1,1,1,1,1,1,1,1,1,1,1,1,1,1,1,1,1,1,1,1,
1,1,1,1,1,1,1,1,1,1,1,1,1,1,4),(0.,0.0642013499338862),(14.3984001269718,
15.3908199671854,16.383239807399,17.3756596476127,18.3680794878263,19.3604993280399,
20.3529191682536,21.3453390084672,22.3377588486808,23.3301786888945,24.3225985291081,
25.3150183693217,26.3074382095353,27.299858049749,28.2922778899626,29.2846977301762,
30.2771175703899,31.2695374106035,32.2619572508171,33.2543770910308,34.2467969312444,
35.239216771458,36.2316366116717,37.2240564518853,38.2164762920989,39.2088961323126,
40.2013159725262,41.1937358127398,42.1861556529534,43.1785754931671,44.1709953333807,
45.1634151735943,46.155835013808,47.1482548540216,48.1406746942352,49.1330945344489,
50.1255143746625,51.1179342148761,52.1103540550898,53.1027738953034,54.095193735517,
55.0876135757306,56.0800334159443,57.0724532561579,58.0648730963715,59.0572929365852,
60.0497127767988,61.0421326170124,62.0345524572261,63.0269722974397,64.0193921376533,
65.011811977867,66.0042318180806,66.9966516582942,67.9890714985079,68.9814913387215,
69.9739111789351,70.9663310191488,71.9587508593624,72.951170699576,73.9435905397896,
74.9360103800033,75.9284302202169,76.9208500604305,77.9132699006442,78.9056897408578,
79.8981095810714,80.8905294212851,81.8829492614987,82.8753691017123,83.867788941926,
84.8602087821396,85.8526286223532,86.8450484625669,87.8374683027805,88.8298881429941,
89.8223079832078,90.8147278234214,91.807147663635,92.7995675038486,93.7919873440623,
94.7844071842759,95.7768270244895,96.7692468647032,97.7616667049168,98.7540865451304,
99.7465063853441,100.738926225558,101.731346065771,102.723765905985,103.716185746199,
104.708605586412,105.701025426626,106.693445266839,107.685865107053,108.678284947267,
109.67070478748,110.663124627694),.UNSPECIFIED.);
#585=B_SPLINE_SURFACE_WITH_KNOTS('',3,3,((#27743,#27744,#27745,#27746,#27747,
#27748,#27749,#27750,#27751,#27752,#27753,#27754,#27755,#27756,#27757,#27758,
#27759,#27760,#27761,#27762,#27763,#27764,#27765,#27766,#27767,#27768,#27769,
#27770,#27771,#27772,#27773,#27774,#27775,#27776,#27777,#27778,#27779,#27780,
#27781,#27782,#27783,#27784,#27785,#27786,#27787,#27788,#27789,#27790,#27791,
#27792,#27793,#27794,#27795,#27796,#27797,#27798,#27799,#27800,#27801,#27802,
#27803,#27804,#27805,#27806,#27807,#27808,#27809,#27810,#27811,#27812,#27813,
#27814,#27815,#27816,#27817,#27818,#27819,#27820,#27821,#27822,#27823,#27824,
#27825,#27826,#27827,#27828,#27829,#27830,#27831,#27832,#27833,#27834,#27835,
#27836,#27837,#27838,#27839,#27840,#27841,#27842),(#27843,#27844,#27845,
#27846,#27847,#27848,#27849,#27850,#27851,#27852,#27853,#27854,#27855,#27856,
#27857,#27858,#27859,#27860,#27861,#27862,#27863,#27864,#27865,#27866,#27867,
#27868,#27869,#27870,#27871,#27872,#27873,#27874,#27875,#27876,#27877,#27878,
#27879,#27880,#27881,#27882,#27883,#27884,#27885,#27886,#27887,#27888,#27889,
#27890,#27891,#27892,#27893,#27894,#27895,#27896,#27897,#27898,#27899,#27900,
#27901,#27902,#27903,#27904,#27905,#27906,#27907,#27908,#27909,#27910,#27911,
#27912,#27913,#27914,#27915,#27916,#27917,#27918,#27919,#27920,#27921,#27922,
#27923,#27924,#27925,#27926,#27927,#27928,#27929,#27930,#27931,#27932,#27933,
#27934,#27935,#27936,#27937,#27938,#27939,#27940,#27941,#27942),(#27943,
#27944,#27945,#27946,#27947,#27948,#27949,#27950,#27951,#27952,#27953,#27954,
#27955,#27956,#27957,#27958,#27959,#27960,#27961,#27962,#27963,#27964,#27965,
#27966,#27967,#27968,#27969,#27970,#27971,#27972,#27973,#27974,#27975,#27976,
#27977,#27978,#27979,#27980,#27981,#27982,#27983,#27984,#27985,#27986,#27987,
#27988,#27989,#27990,#27991,#27992,#27993,#27994,#27995,#27996,#27997,#27998,
#27999,#28000,#28001,#28002,#28003,#28004,#28005,#28006,#28007,#28008,#28009,
#28010,#28011,#28012,#28013,#28014,#28015,#28016,#28017,#28018,#28019,#28020,
#28021,#28022,#28023,#28024,#28025,#28026,#28027,#28028,#28029,#28030,#28031,
#28032,#28033,#28034,#28035,#28036,#28037,#28038,#28039,#28040,#28041,#28042),
(#28043,#28044,#28045,#28046,#28047,#28048,#28049,#28050,#28051,#28052,
#28053,#28054,#28055,#28056,#28057,#28058,#28059,#28060,#28061,#28062,#28063,
#28064,#28065,#28066,#28067,#28068,#28069,#28070,#28071,#28072,#28073,#28074,
#28075,#28076,#28077,#28078,#28079,#28080,#28081,#28082,#28083,#28084,#28085,
#28086,#28087,#28088,#28089,#28090,#28091,#28092,#28093,#28094,#28095,#28096,
#28097,#28098,#28099,#28100,#28101,#28102,#28103,#28104,#28105,#28106,#28107,
#28108,#28109,#28110,#28111,#28112,#28113,#28114,#28115,#28116,#28117,#28118,
#28119,#28120,#28121,#28122,#28123,#28124,#28125,#28126,#28127,#28128,#28129,
#28130,#28131,#28132,#28133,#28134,#28135,#28136,#28137,#28138,#28139,#28140,
#28141,#28142)),.UNSPECIFIED.,.F.,.F.,.F.,(4,4),(4,1,1,1,1,1,1,1,1,1,1,
1,1,1,1,1,1,1,1,1,1,1,1,1,1,1,1,1,1,1,1,1,1,1,1,1,1,1,1,1,1,1,1,1,1,1,1,
1,1,1,1,1,1,1,1,1,1,1,1,1,1,1,1,1,1,1,1,1,1,1,1,1,1,1,1,1,1,1,1,1,1,1,1,
1,1,1,1,1,1,1,1,1,1,1,1,1,1,4),(0.,0.0642013499338866),(11.8589888623077,
12.8514087025214,13.843828542735,14.8362483829486,15.8286682231623,16.8210880633759,
17.8135079035895,18.8059277438032,19.7983475840168,20.7907674242304,21.7831872644441,
22.7756071046577,23.7680269448713,24.7604467850849,25.7528666252986,26.7452864655122,
27.7377063057258,28.7301261459395,29.7225459861531,30.7149658263667,31.7073856665804,
32.699805506794,33.6922253470076,34.6846451872213,35.6770650274349,36.6694848676485,
37.6619047078622,38.6543245480758,39.6467443882894,40.639164228503,41.6315840687167,
42.6240039089303,43.6164237491439,44.6088435893576,45.6012634295712,46.5936832697848,
47.5861031099985,48.5785229502121,49.5709427904257,50.5633626306394,51.555782470853,
52.5482023110666,53.5406221512803,54.5330419914939,55.5254618317075,56.5178816719212,
57.5103015121348,58.5027213523484,59.4951411925621,60.4875610327757,61.4799808729893,
62.4724007132029,63.4648205534166,64.4572403936302,65.4496602338438,66.4420800740575,
67.4344999142711,68.4269197544847,69.4193395946984,70.411759434912,71.4041792751256,
72.3965991153393,73.3890189555529,74.3814387957665,75.3738586359802,76.3662784761938,
77.3586983164074,78.3511181566211,79.3435379968347,80.3359578370483,81.328377677262,
82.3207975174756,83.3132173576892,84.3056371979029,85.2980570381165,86.2904768783301,
87.2828967185437,88.2753165587574,89.267736398971,90.2601562391846,91.2525760793983,
92.2449959196119,93.2374157598255,94.2298356000392,95.2222554402528,96.2146752804664,
97.2070951206801,98.1995149608937,99.1919348011073,100.184354641321,101.176774481535,
102.169194321748,103.161614161962,104.154034002175,105.146453842389,106.138873682603,
107.131293522816,108.12371336303),.UNSPECIFIED.);
#586=B_SPLINE_SURFACE_WITH_KNOTS('',3,3,((#28168,#28169,#28170,#28171,#28172,
#28173,#28174,#28175,#28176,#28177,#28178,#28179,#28180,#28181,#28182,#28183,
#28184,#28185,#28186,#28187,#28188,#28189,#28190,#28191,#28192,#28193,#28194,
#28195,#28196,#28197,#28198,#28199,#28200,#28201,#28202,#28203,#28204,#28205,
#28206,#28207,#28208,#28209,#28210,#28211,#28212,#28213,#28214,#28215,#28216,
#28217,#28218,#28219,#28220,#28221,#28222,#28223,#28224,#28225,#28226,#28227,
#28228,#28229,#28230,#28231,#28232,#28233,#28234,#28235,#28236,#28237,#28238,
#28239,#28240,#28241,#28242,#28243,#28244,#28245,#28246,#28247,#28248,#28249,
#28250,#28251,#28252,#28253,#28254,#28255,#28256,#28257,#28258,#28259,#28260,
#28261,#28262,#28263,#28264,#28265,#28266,#28267),(#28268,#28269,#28270,
#28271,#28272,#28273,#28274,#28275,#28276,#28277,#28278,#28279,#28280,#28281,
#28282,#28283,#28284,#28285,#28286,#28287,#28288,#28289,#28290,#28291,#28292,
#28293,#28294,#28295,#28296,#28297,#28298,#28299,#28300,#28301,#28302,#28303,
#28304,#28305,#28306,#28307,#28308,#28309,#28310,#28311,#28312,#28313,#28314,
#28315,#28316,#28317,#28318,#28319,#28320,#28321,#28322,#28323,#28324,#28325,
#28326,#28327,#28328,#28329,#28330,#28331,#28332,#28333,#28334,#28335,#28336,
#28337,#28338,#28339,#28340,#28341,#28342,#28343,#28344,#28345,#28346,#28347,
#28348,#28349,#28350,#28351,#28352,#28353,#28354,#28355,#28356,#28357,#28358,
#28359,#28360,#28361,#28362,#28363,#28364,#28365,#28366,#28367),(#28368,
#28369,#28370,#28371,#28372,#28373,#28374,#28375,#28376,#28377,#28378,#28379,
#28380,#28381,#28382,#28383,#28384,#28385,#28386,#28387,#28388,#28389,#28390,
#28391,#28392,#28393,#28394,#28395,#28396,#28397,#28398,#28399,#28400,#28401,
#28402,#28403,#28404,#28405,#28406,#28407,#28408,#28409,#28410,#28411,#28412,
#28413,#28414,#28415,#28416,#28417,#28418,#28419,#28420,#28421,#28422,#28423,
#28424,#28425,#28426,#28427,#28428,#28429,#28430,#28431,#28432,#28433,#28434,
#28435,#28436,#28437,#28438,#28439,#28440,#28441,#28442,#28443,#28444,#28445,
#28446,#28447,#28448,#28449,#28450,#28451,#28452,#28453,#28454,#28455,#28456,
#28457,#28458,#28459,#28460,#28461,#28462,#28463,#28464,#28465,#28466,#28467),
(#28468,#28469,#28470,#28471,#28472,#28473,#28474,#28475,#28476,#28477,
#28478,#28479,#28480,#28481,#28482,#28483,#28484,#28485,#28486,#28487,#28488,
#28489,#28490,#28491,#28492,#28493,#28494,#28495,#28496,#28497,#28498,#28499,
#28500,#28501,#28502,#28503,#28504,#28505,#28506,#28507,#28508,#28509,#28510,
#28511,#28512,#28513,#28514,#28515,#28516,#28517,#28518,#28519,#28520,#28521,
#28522,#28523,#28524,#28525,#28526,#28527,#28528,#28529,#28530,#28531,#28532,
#28533,#28534,#28535,#28536,#28537,#28538,#28539,#28540,#28541,#28542,#28543,
#28544,#28545,#28546,#28547,#28548,#28549,#28550,#28551,#28552,#28553,#28554,
#28555,#28556,#28557,#28558,#28559,#28560,#28561,#28562,#28563,#28564,#28565,
#28566,#28567)),.UNSPECIFIED.,.F.,.F.,.F.,(4,4),(4,1,1,1,1,1,1,1,1,1,1,
1,1,1,1,1,1,1,1,1,1,1,1,1,1,1,1,1,1,1,1,1,1,1,1,1,1,1,1,1,1,1,1,1,1,1,1,
1,1,1,1,1,1,1,1,1,1,1,1,1,1,1,1,1,1,1,1,1,1,1,1,1,1,1,1,1,1,1,1,1,1,1,1,
1,1,1,1,1,1,1,1,1,1,1,1,1,1,4),(0.,0.0642013499338862),(14.3984001269718,
15.3908199671854,16.383239807399,17.3756596476127,18.3680794878263,19.3604993280399,
20.3529191682536,21.3453390084672,22.3377588486808,23.3301786888945,24.3225985291081,
25.3150183693217,26.3074382095353,27.299858049749,28.2922778899626,29.2846977301762,
30.2771175703899,31.2695374106035,32.2619572508171,33.2543770910308,34.2467969312444,
35.239216771458,36.2316366116717,37.2240564518853,38.2164762920989,39.2088961323126,
40.2013159725262,41.1937358127398,42.1861556529534,43.1785754931671,44.1709953333807,
45.1634151735943,46.155835013808,47.1482548540216,48.1406746942352,49.1330945344489,
50.1255143746625,51.1179342148761,52.1103540550898,53.1027738953034,54.095193735517,
55.0876135757306,56.0800334159443,57.0724532561579,58.0648730963715,59.0572929365852,
60.0497127767988,61.0421326170124,62.0345524572261,63.0269722974397,64.0193921376533,
65.011811977867,66.0042318180806,66.9966516582942,67.9890714985079,68.9814913387215,
69.9739111789351,70.9663310191488,71.9587508593624,72.951170699576,73.9435905397896,
74.9360103800033,75.9284302202169,76.9208500604305,77.9132699006442,78.9056897408578,
79.8981095810714,80.8905294212851,81.8829492614987,82.8753691017123,83.867788941926,
84.8602087821396,85.8526286223532,86.8450484625669,87.8374683027805,88.8298881429941,
89.8223079832078,90.8147278234214,91.807147663635,92.7995675038486,93.7919873440623,
94.7844071842759,95.7768270244895,96.7692468647032,97.7616667049168,98.7540865451304,
99.7465063853441,100.738926225558,101.731346065771,102.723765905985,103.716185746199,
104.708605586412,105.701025426626,106.693445266839,107.685865107053,108.678284947267,
109.67070478748,110.663124627694),.UNSPECIFIED.);
#587=B_SPLINE_SURFACE_WITH_KNOTS('',3,3,((#28837,#28838,#28839,#28840,#28841,
#28842,#28843,#28844,#28845,#28846,#28847,#28848,#28849,#28850,#28851,#28852,
#28853,#28854,#28855,#28856,#28857,#28858,#28859,#28860,#28861,#28862,#28863,
#28864,#28865,#28866,#28867,#28868,#28869,#28870,#28871,#28872,#28873,#28874,
#28875,#28876,#28877,#28878,#28879,#28880,#28881,#28882,#28883,#28884,#28885,
#28886,#28887,#28888,#28889,#28890,#28891,#28892,#28893,#28894,#28895,#28896,
#28897,#28898,#28899,#28900,#28901,#28902,#28903,#28904,#28905,#28906,#28907,
#28908,#28909,#28910,#28911,#28912,#28913,#28914,#28915,#28916,#28917,#28918,
#28919,#28920,#28921,#28922,#28923,#28924,#28925,#28926,#28927,#28928,#28929,
#28930,#28931,#28932,#28933,#28934,#28935,#28936),(#28937,#28938,#28939,
#28940,#28941,#28942,#28943,#28944,#28945,#28946,#28947,#28948,#28949,#28950,
#28951,#28952,#28953,#28954,#28955,#28956,#28957,#28958,#28959,#28960,#28961,
#28962,#28963,#28964,#28965,#28966,#28967,#28968,#28969,#28970,#28971,#28972,
#28973,#28974,#28975,#28976,#28977,#28978,#28979,#28980,#28981,#28982,#28983,
#28984,#28985,#28986,#28987,#28988,#28989,#28990,#28991,#28992,#28993,#28994,
#28995,#28996,#28997,#28998,#28999,#29000,#29001,#29002,#29003,#29004,#29005,
#29006,#29007,#29008,#29009,#29010,#29011,#29012,#29013,#29014,#29015,#29016,
#29017,#29018,#29019,#29020,#29021,#29022,#29023,#29024,#29025,#29026,#29027,
#29028,#29029,#29030,#29031,#29032,#29033,#29034,#29035,#29036),(#29037,
#29038,#29039,#29040,#29041,#29042,#29043,#29044,#29045,#29046,#29047,#29048,
#29049,#29050,#29051,#29052,#29053,#29054,#29055,#29056,#29057,#29058,#29059,
#29060,#29061,#29062,#29063,#29064,#29065,#29066,#29067,#29068,#29069,#29070,
#29071,#29072,#29073,#29074,#29075,#29076,#29077,#29078,#29079,#29080,#29081,
#29082,#29083,#29084,#29085,#29086,#29087,#29088,#29089,#29090,#29091,#29092,
#29093,#29094,#29095,#29096,#29097,#29098,#29099,#29100,#29101,#29102,#29103,
#29104,#29105,#29106,#29107,#29108,#29109,#29110,#29111,#29112,#29113,#29114,
#29115,#29116,#29117,#29118,#29119,#29120,#29121,#29122,#29123,#29124,#29125,
#29126,#29127,#29128,#29129,#29130,#29131,#29132,#29133,#29134,#29135,#29136),
(#29137,#29138,#29139,#29140,#29141,#29142,#29143,#29144,#29145,#29146,
#29147,#29148,#29149,#29150,#29151,#29152,#29153,#29154,#29155,#29156,#29157,
#29158,#29159,#29160,#29161,#29162,#29163,#29164,#29165,#29166,#29167,#29168,
#29169,#29170,#29171,#29172,#29173,#29174,#29175,#29176,#29177,#29178,#29179,
#29180,#29181,#29182,#29183,#29184,#29185,#29186,#29187,#29188,#29189,#29190,
#29191,#29192,#29193,#29194,#29195,#29196,#29197,#29198,#29199,#29200,#29201,
#29202,#29203,#29204,#29205,#29206,#29207,#29208,#29209,#29210,#29211,#29212,
#29213,#29214,#29215,#29216,#29217,#29218,#29219,#29220,#29221,#29222,#29223,
#29224,#29225,#29226,#29227,#29228,#29229,#29230,#29231,#29232,#29233,#29234,
#29235,#29236)),.UNSPECIFIED.,.F.,.F.,.F.,(4,4),(4,1,1,1,1,1,1,1,1,1,1,
1,1,1,1,1,1,1,1,1,1,1,1,1,1,1,1,1,1,1,1,1,1,1,1,1,1,1,1,1,1,1,1,1,1,1,1,
1,1,1,1,1,1,1,1,1,1,1,1,1,1,1,1,1,1,1,1,1,1,1,1,1,1,1,1,1,1,1,1,1,1,1,1,
1,1,1,1,1,1,1,1,1,1,1,1,1,1,4),(0.,0.0642013499338866),(11.8589888623077,
12.8514087025214,13.843828542735,14.8362483829486,15.8286682231623,16.8210880633759,
17.8135079035895,18.8059277438032,19.7983475840168,20.7907674242304,21.7831872644441,
22.7756071046577,23.7680269448713,24.7604467850849,25.7528666252986,26.7452864655122,
27.7377063057258,28.7301261459395,29.7225459861531,30.7149658263667,31.7073856665804,
32.699805506794,33.6922253470076,34.6846451872213,35.6770650274349,36.6694848676485,
37.6619047078622,38.6543245480758,39.6467443882894,40.639164228503,41.6315840687167,
42.6240039089303,43.6164237491439,44.6088435893576,45.6012634295712,46.5936832697848,
47.5861031099985,48.5785229502121,49.5709427904257,50.5633626306394,51.555782470853,
52.5482023110666,53.5406221512803,54.5330419914939,55.5254618317075,56.5178816719212,
57.5103015121348,58.5027213523484,59.4951411925621,60.4875610327757,61.4799808729893,
62.4724007132029,63.4648205534166,64.4572403936302,65.4496602338438,66.4420800740575,
67.4344999142711,68.4269197544847,69.4193395946984,70.411759434912,71.4041792751256,
72.3965991153393,73.3890189555529,74.3814387957665,75.3738586359802,76.3662784761938,
77.3586983164074,78.3511181566211,79.3435379968347,80.3359578370483,81.328377677262,
82.3207975174756,83.3132173576892,84.3056371979029,85.2980570381165,86.2904768783301,
87.2828967185437,88.2753165587574,89.267736398971,90.2601562391846,91.2525760793983,
92.2449959196119,93.2374157598255,94.2298356000392,95.2222554402528,96.2146752804664,
97.2070951206801,98.1995149608937,99.1919348011073,100.184354641321,101.176774481535,
102.169194321748,103.161614161962,104.154034002175,105.146453842389,106.138873682603,
107.131293522816,108.12371336303),.UNSPECIFIED.);
#588=B_SPLINE_SURFACE_WITH_KNOTS('',3,3,((#29262,#29263,#29264,#29265,#29266,
#29267,#29268,#29269,#29270,#29271,#29272,#29273,#29274,#29275,#29276,#29277,
#29278,#29279,#29280,#29281,#29282,#29283,#29284,#29285,#29286,#29287,#29288,
#29289,#29290,#29291,#29292,#29293,#29294,#29295,#29296,#29297,#29298,#29299,
#29300,#29301,#29302,#29303,#29304,#29305,#29306,#29307,#29308,#29309,#29310,
#29311,#29312,#29313,#29314,#29315,#29316,#29317,#29318,#29319,#29320,#29321,
#29322,#29323,#29324,#29325,#29326,#29327,#29328,#29329,#29330,#29331,#29332,
#29333,#29334,#29335,#29336,#29337,#29338,#29339,#29340,#29341,#29342,#29343,
#29344,#29345,#29346,#29347,#29348,#29349,#29350,#29351,#29352,#29353,#29354,
#29355,#29356,#29357,#29358,#29359,#29360,#29361),(#29362,#29363,#29364,
#29365,#29366,#29367,#29368,#29369,#29370,#29371,#29372,#29373,#29374,#29375,
#29376,#29377,#29378,#29379,#29380,#29381,#29382,#29383,#29384,#29385,#29386,
#29387,#29388,#29389,#29390,#29391,#29392,#29393,#29394,#29395,#29396,#29397,
#29398,#29399,#29400,#29401,#29402,#29403,#29404,#29405,#29406,#29407,#29408,
#29409,#29410,#29411,#29412,#29413,#29414,#29415,#29416,#29417,#29418,#29419,
#29420,#29421,#29422,#29423,#29424,#29425,#29426,#29427,#29428,#29429,#29430,
#29431,#29432,#29433,#29434,#29435,#29436,#29437,#29438,#29439,#29440,#29441,
#29442,#29443,#29444,#29445,#29446,#29447,#29448,#29449,#29450,#29451,#29452,
#29453,#29454,#29455,#29456,#29457,#29458,#29459,#29460,#29461),(#29462,
#29463,#29464,#29465,#29466,#29467,#29468,#29469,#29470,#29471,#29472,#29473,
#29474,#29475,#29476,#29477,#29478,#29479,#29480,#29481,#29482,#29483,#29484,
#29485,#29486,#29487,#29488,#29489,#29490,#29491,#29492,#29493,#29494,#29495,
#29496,#29497,#29498,#29499,#29500,#29501,#29502,#29503,#29504,#29505,#29506,
#29507,#29508,#29509,#29510,#29511,#29512,#29513,#29514,#29515,#29516,#29517,
#29518,#29519,#29520,#29521,#29522,#29523,#29524,#29525,#29526,#29527,#29528,
#29529,#29530,#29531,#29532,#29533,#29534,#29535,#29536,#29537,#29538,#29539,
#29540,#29541,#29542,#29543,#29544,#29545,#29546,#29547,#29548,#29549,#29550,
#29551,#29552,#29553,#29554,#29555,#29556,#29557,#29558,#29559,#29560,#29561),
(#29562,#29563,#29564,#29565,#29566,#29567,#29568,#29569,#29570,#29571,
#29572,#29573,#29574,#29575,#29576,#29577,#29578,#29579,#29580,#29581,#29582,
#29583,#29584,#29585,#29586,#29587,#29588,#29589,#29590,#29591,#29592,#29593,
#29594,#29595,#29596,#29597,#29598,#29599,#29600,#29601,#29602,#29603,#29604,
#29605,#29606,#29607,#29608,#29609,#29610,#29611,#29612,#29613,#29614,#29615,
#29616,#29617,#29618,#29619,#29620,#29621,#29622,#29623,#29624,#29625,#29626,
#29627,#29628,#29629,#29630,#29631,#29632,#29633,#29634,#29635,#29636,#29637,
#29638,#29639,#29640,#29641,#29642,#29643,#29644,#29645,#29646,#29647,#29648,
#29649,#29650,#29651,#29652,#29653,#29654,#29655,#29656,#29657,#29658,#29659,
#29660,#29661)),.UNSPECIFIED.,.F.,.F.,.F.,(4,4),(4,1,1,1,1,1,1,1,1,1,1,
1,1,1,1,1,1,1,1,1,1,1,1,1,1,1,1,1,1,1,1,1,1,1,1,1,1,1,1,1,1,1,1,1,1,1,1,
1,1,1,1,1,1,1,1,1,1,1,1,1,1,1,1,1,1,1,1,1,1,1,1,1,1,1,1,1,1,1,1,1,1,1,1,
1,1,1,1,1,1,1,1,1,1,1,1,1,1,4),(0.,0.0642013499338862),(14.3984001269718,
15.3908199671854,16.383239807399,17.3756596476127,18.3680794878263,19.3604993280399,
20.3529191682536,21.3453390084672,22.3377588486808,23.3301786888945,24.3225985291081,
25.3150183693217,26.3074382095353,27.299858049749,28.2922778899626,29.2846977301762,
30.2771175703899,31.2695374106035,32.2619572508171,33.2543770910308,34.2467969312444,
35.239216771458,36.2316366116717,37.2240564518853,38.2164762920989,39.2088961323126,
40.2013159725262,41.1937358127398,42.1861556529534,43.1785754931671,44.1709953333807,
45.1634151735943,46.155835013808,47.1482548540216,48.1406746942352,49.1330945344489,
50.1255143746625,51.1179342148761,52.1103540550898,53.1027738953034,54.095193735517,
55.0876135757306,56.0800334159443,57.0724532561579,58.0648730963715,59.0572929365852,
60.0497127767988,61.0421326170124,62.0345524572261,63.0269722974397,64.0193921376533,
65.011811977867,66.0042318180806,66.9966516582942,67.9890714985079,68.9814913387215,
69.9739111789351,70.9663310191488,71.9587508593624,72.951170699576,73.9435905397896,
74.9360103800033,75.9284302202169,76.9208500604305,77.9132699006442,78.9056897408578,
79.8981095810714,80.8905294212851,81.8829492614987,82.8753691017123,83.867788941926,
84.8602087821396,85.8526286223532,86.8450484625669,87.8374683027805,88.8298881429941,
89.8223079832078,90.8147278234214,91.807147663635,92.7995675038486,93.7919873440623,
94.7844071842759,95.7768270244895,96.7692468647032,97.7616667049168,98.7540865451304,
99.7465063853441,100.738926225558,101.731346065771,102.723765905985,103.716185746199,
104.708605586412,105.701025426626,106.693445266839,107.685865107053,108.678284947267,
109.67070478748,110.663124627694),.UNSPECIFIED.);
#589=B_SPLINE_SURFACE_WITH_KNOTS('',3,3,((#29906,#29907,#29908,#29909,#29910,
#29911,#29912,#29913,#29914,#29915,#29916,#29917,#29918,#29919,#29920,#29921,
#29922,#29923,#29924,#29925,#29926,#29927,#29928,#29929,#29930,#29931,#29932,
#29933,#29934,#29935,#29936,#29937,#29938,#29939,#29940,#29941,#29942,#29943,
#29944,#29945,#29946,#29947,#29948,#29949,#29950,#29951,#29952,#29953,#29954,
#29955,#29956,#29957,#29958,#29959,#29960,#29961,#29962,#29963,#29964,#29965,
#29966,#29967,#29968,#29969,#29970,#29971,#29972,#29973,#29974,#29975,#29976,
#29977,#29978,#29979,#29980,#29981,#29982,#29983,#29984,#29985,#29986,#29987,
#29988,#29989,#29990,#29991,#29992,#29993,#29994,#29995,#29996,#29997,#29998,
#29999,#30000,#30001,#30002,#30003,#30004,#30005,#30006,#30007,#30008,#30009),
(#30010,#30011,#30012,#30013,#30014,#30015,#30016,#30017,#30018,#30019,
#30020,#30021,#30022,#30023,#30024,#30025,#30026,#30027,#30028,#30029,#30030,
#30031,#30032,#30033,#30034,#30035,#30036,#30037,#30038,#30039,#30040,#30041,
#30042,#30043,#30044,#30045,#30046,#30047,#30048,#30049,#30050,#30051,#30052,
#30053,#30054,#30055,#30056,#30057,#30058,#30059,#30060,#30061,#30062,#30063,
#30064,#30065,#30066,#30067,#30068,#30069,#30070,#30071,#30072,#30073,#30074,
#30075,#30076,#30077,#30078,#30079,#30080,#30081,#30082,#30083,#30084,#30085,
#30086,#30087,#30088,#30089,#30090,#30091,#30092,#30093,#30094,#30095,#30096,
#30097,#30098,#30099,#30100,#30101,#30102,#30103,#30104,#30105,#30106,#30107,
#30108,#30109,#30110,#30111,#30112,#30113),(#30114,#30115,#30116,#30117,
#30118,#30119,#30120,#30121,#30122,#30123,#30124,#30125,#30126,#30127,#30128,
#30129,#30130,#30131,#30132,#30133,#30134,#30135,#30136,#30137,#30138,#30139,
#30140,#30141,#30142,#30143,#30144,#30145,#30146,#30147,#30148,#30149,#30150,
#30151,#30152,#30153,#30154,#30155,#30156,#30157,#30158,#30159,#30160,#30161,
#30162,#30163,#30164,#30165,#30166,#30167,#30168,#30169,#30170,#30171,#30172,
#30173,#30174,#30175,#30176,#30177,#30178,#30179,#30180,#30181,#30182,#30183,
#30184,#30185,#30186,#30187,#30188,#30189,#30190,#30191,#30192,#30193,#30194,
#30195,#30196,#30197,#30198,#30199,#30200,#30201,#30202,#30203,#30204,#30205,
#30206,#30207,#30208,#30209,#30210,#30211,#30212,#30213,#30214,#30215,#30216,
#30217),(#30218,#30219,#30220,#30221,#30222,#30223,#30224,#30225,#30226,
#30227,#30228,#30229,#30230,#30231,#30232,#30233,#30234,#30235,#30236,#30237,
#30238,#30239,#30240,#30241,#30242,#30243,#30244,#30245,#30246,#30247,#30248,
#30249,#30250,#30251,#30252,#30253,#30254,#30255,#30256,#30257,#30258,#30259,
#30260,#30261,#30262,#30263,#30264,#30265,#30266,#30267,#30268,#30269,#30270,
#30271,#30272,#30273,#30274,#30275,#30276,#30277,#30278,#30279,#30280,#30281,
#30282,#30283,#30284,#30285,#30286,#30287,#30288,#30289,#30290,#30291,#30292,
#30293,#30294,#30295,#30296,#30297,#30298,#30299,#30300,#30301,#30302,#30303,
#30304,#30305,#30306,#30307,#30308,#30309,#30310,#30311,#30312,#30313,#30314,
#30315,#30316,#30317,#30318,#30319,#30320,#30321)),.UNSPECIFIED.,.F.,.F.,
 .F.,(4,4),(4,1,1,1,1,1,1,1,1,1,1,1,1,1,1,1,1,1,1,1,1,1,1,1,1,1,1,1,1,1,
1,1,1,1,1,1,1,1,1,1,1,1,1,1,1,1,1,1,1,1,1,1,1,1,1,1,1,1,1,1,1,1,1,1,1,1,
1,1,1,1,1,1,1,1,1,1,1,1,1,1,1,1,1,1,1,1,1,1,1,1,1,1,1,1,1,1,1,1,1,1,1,4),
(0.,0.0448889834294935),(11.8615800042566,12.8591085386932,13.8566370731298,
14.8541656075664,15.851694142003,16.8492226764396,17.8467512108762,18.8442797453128,
19.8418082797494,20.839336814186,21.8368653486226,22.8343938830591,23.8319224174958,
24.8294509519324,25.8269794863689,26.8245080208056,27.8220365552421,28.8195650896787,
29.8170936241154,30.8146221585519,31.8121506929885,32.8096792274251,33.8072077618617,
34.8047362962984,35.8022648307349,36.7997933651715,37.7973218996081,38.7948504340447,
39.7923789684813,40.7899075029179,41.7874360373545,42.7849645717911,43.7824931062277,
44.7800216406643,45.7775501751009,46.7750787095375,47.7726072439741,48.7701357784107,
49.7676643128473,50.7651928472839,51.7627213817205,52.7602499161571,53.7577784505937,
54.7553069850303,55.7528355194669,56.7503640539035,57.7478925883401,58.7454211227767,
59.7429496572133,60.7404781916499,61.7380067260865,62.7355352605231,63.7330637949597,
64.7305923293963,65.7281208638329,66.7256493982695,67.7231779327061,68.7207064671427,
69.7182350015793,70.7157635360159,71.7132920704525,72.7108206048891,73.7083491393257,
74.7058776737623,75.7034062081989,76.7009347426355,77.6984632770721,78.6959918115087,
79.6935203459453,80.6910488803819,81.6885774148185,82.6861059492551,83.6836344836917,
84.6811630181283,85.6786915525649,86.6762200870015,87.6737486214381,88.6712771558747,
89.6688056903113,90.6663342247479,91.6638627591845,92.6613912936211,93.6589198280577,
94.6564483624943,95.6539768969309,96.6515054313675,97.6490339658041,98.6465625002407,
99.6440910346773,100.641619569114,101.639148103551,102.636676637987,103.634205172424,
104.63173370686,105.629262241297,106.626790775734,107.62431931017,108.621847844607,
109.619376379043,110.61690491348,111.614433447917,112.611961982353),
 .UNSPECIFIED.);
#590=B_SPLINE_SURFACE_WITH_KNOTS('',3,3,((#30429,#30430,#30431,#30432,#30433,
#30434,#30435,#30436,#30437,#30438,#30439,#30440,#30441,#30442,#30443,#30444,
#30445,#30446,#30447,#30448,#30449,#30450,#30451,#30452,#30453,#30454,#30455,
#30456,#30457,#30458,#30459,#30460,#30461,#30462,#30463,#30464,#30465,#30466,
#30467,#30468,#30469,#30470,#30471,#30472,#30473,#30474,#30475,#30476,#30477,
#30478,#30479,#30480,#30481,#30482,#30483,#30484,#30485,#30486,#30487,#30488,
#30489,#30490,#30491,#30492,#30493,#30494,#30495,#30496,#30497,#30498,#30499,
#30500,#30501,#30502,#30503,#30504,#30505,#30506,#30507,#30508,#30509,#30510,
#30511,#30512,#30513,#30514,#30515,#30516,#30517,#30518,#30519,#30520,#30521,
#30522,#30523,#30524,#30525,#30526,#30527,#30528,#30529,#30530,#30531,#30532),
(#30533,#30534,#30535,#30536,#30537,#30538,#30539,#30540,#30541,#30542,
#30543,#30544,#30545,#30546,#30547,#30548,#30549,#30550,#30551,#30552,#30553,
#30554,#30555,#30556,#30557,#30558,#30559,#30560,#30561,#30562,#30563,#30564,
#30565,#30566,#30567,#30568,#30569,#30570,#30571,#30572,#30573,#30574,#30575,
#30576,#30577,#30578,#30579,#30580,#30581,#30582,#30583,#30584,#30585,#30586,
#30587,#30588,#30589,#30590,#30591,#30592,#30593,#30594,#30595,#30596,#30597,
#30598,#30599,#30600,#30601,#30602,#30603,#30604,#30605,#30606,#30607,#30608,
#30609,#30610,#30611,#30612,#30613,#30614,#30615,#30616,#30617,#30618,#30619,
#30620,#30621,#30622,#30623,#30624,#30625,#30626,#30627,#30628,#30629,#30630,
#30631,#30632,#30633,#30634,#30635,#30636),(#30637,#30638,#30639,#30640,
#30641,#30642,#30643,#30644,#30645,#30646,#30647,#30648,#30649,#30650,#30651,
#30652,#30653,#30654,#30655,#30656,#30657,#30658,#30659,#30660,#30661,#30662,
#30663,#30664,#30665,#30666,#30667,#30668,#30669,#30670,#30671,#30672,#30673,
#30674,#30675,#30676,#30677,#30678,#30679,#30680,#30681,#30682,#30683,#30684,
#30685,#30686,#30687,#30688,#30689,#30690,#30691,#30692,#30693,#30694,#30695,
#30696,#30697,#30698,#30699,#30700,#30701,#30702,#30703,#30704,#30705,#30706,
#30707,#30708,#30709,#30710,#30711,#30712,#30713,#30714,#30715,#30716,#30717,
#30718,#30719,#30720,#30721,#30722,#30723,#30724,#30725,#30726,#30727,#30728,
#30729,#30730,#30731,#30732,#30733,#30734,#30735,#30736,#30737,#30738,#30739,
#30740),(#30741,#30742,#30743,#30744,#30745,#30746,#30747,#30748,#30749,
#30750,#30751,#30752,#30753,#30754,#30755,#30756,#30757,#30758,#30759,#30760,
#30761,#30762,#30763,#30764,#30765,#30766,#30767,#30768,#30769,#30770,#30771,
#30772,#30773,#30774,#30775,#30776,#30777,#30778,#30779,#30780,#30781,#30782,
#30783,#30784,#30785,#30786,#30787,#30788,#30789,#30790,#30791,#30792,#30793,
#30794,#30795,#30796,#30797,#30798,#30799,#30800,#30801,#30802,#30803,#30804,
#30805,#30806,#30807,#30808,#30809,#30810,#30811,#30812,#30813,#30814,#30815,
#30816,#30817,#30818,#30819,#30820,#30821,#30822,#30823,#30824,#30825,#30826,
#30827,#30828,#30829,#30830,#30831,#30832,#30833,#30834,#30835,#30836,#30837,
#30838,#30839,#30840,#30841,#30842,#30843,#30844)),.UNSPECIFIED.,.F.,.F.,
 .F.,(4,4),(4,1,1,1,1,1,1,1,1,1,1,1,1,1,1,1,1,1,1,1,1,1,1,1,1,1,1,1,1,1,
1,1,1,1,1,1,1,1,1,1,1,1,1,1,1,1,1,1,1,1,1,1,1,1,1,1,1,1,1,1,1,1,1,1,1,1,
1,1,1,1,1,1,1,1,1,1,1,1,1,1,1,1,1,1,1,1,1,1,1,1,1,1,1,1,1,1,1,1,1,1,1,4),
(0.,0.0448889834294935),(14.3981410127768,15.3956695472134,16.39319808165,
17.3907266160866,18.3882551505232,19.3857836849598,20.3833122193964,21.380840753833,
22.3783692882696,23.3758978227062,24.3734263571428,25.3709548915794,26.368483426016,
27.3660119604526,28.3635404948892,29.3610690293258,30.3585975637624,31.356126098199,
32.3536546326356,33.3511831670722,34.3487117015088,35.3462402359454,36.343768770382,
37.3412973048186,38.3388258392552,39.3363543736918,40.3338829081284,41.331411442565,
42.3289399770016,43.3264685114382,44.3239970458748,45.3215255803114,46.319054114748,
47.3165826491846,48.3141111836212,49.3116397180578,50.3091682524944,51.306696786931,
52.3042253213676,53.3017538558042,54.2992823902408,55.2968109246774,56.294339459114,
57.2918679935506,58.2893965279872,59.2869250624238,60.2844535968604,61.281982131297,
62.2795106657336,63.2770392001702,64.2745677346068,65.2720962690434,66.26962480348,
67.2671533379166,68.2646818723532,69.2622104067898,70.2597389412264,71.257267475663,
72.2547960100996,73.2523245445362,74.2498530789728,75.2473816134094,76.244910147846,
77.2424386822826,78.2399672167192,79.2374957511558,80.2350242855924,81.232552820029,
82.2300813544656,83.2276098889022,84.2251384233388,85.2226669577754,86.220195492212,
87.2177240266486,88.2152525610852,89.2127810955218,90.2103096299584,91.207838164395,
92.2053666988316,93.2028952332682,94.2004237677048,95.1979523021414,96.195480836578,
97.1930093710146,98.1905379054512,99.1880664398878,100.185594974324,101.183123508761,
102.180652043198,103.178180577634,104.175709112071,105.173237646507,106.170766180944,
107.168294715381,108.165823249817,109.163351784254,110.16088031869,111.158408853127,
112.155937387564,113.153465922,114.150994456437,115.148522990873),
 .UNSPECIFIED.);
#591=B_SPLINE_SURFACE_WITH_KNOTS('',3,3,((#31149,#31150,#31151,#31152,#31153,
#31154,#31155,#31156,#31157,#31158,#31159,#31160,#31161,#31162,#31163,#31164,
#31165,#31166,#31167,#31168,#31169,#31170,#31171,#31172,#31173,#31174,#31175,
#31176,#31177,#31178,#31179,#31180,#31181,#31182,#31183,#31184,#31185,#31186,
#31187,#31188,#31189,#31190,#31191,#31192,#31193,#31194,#31195,#31196,#31197,
#31198,#31199,#31200,#31201,#31202,#31203,#31204,#31205,#31206,#31207,#31208,
#31209,#31210,#31211,#31212,#31213,#31214,#31215,#31216,#31217,#31218,#31219,
#31220,#31221,#31222,#31223,#31224,#31225,#31226,#31227,#31228,#31229,#31230,
#31231,#31232,#31233,#31234,#31235,#31236,#31237,#31238,#31239,#31240,#31241,
#31242,#31243,#31244,#31245,#31246,#31247,#31248,#31249,#31250,#31251,#31252),
(#31253,#31254,#31255,#31256,#31257,#31258,#31259,#31260,#31261,#31262,
#31263,#31264,#31265,#31266,#31267,#31268,#31269,#31270,#31271,#31272,#31273,
#31274,#31275,#31276,#31277,#31278,#31279,#31280,#31281,#31282,#31283,#31284,
#31285,#31286,#31287,#31288,#31289,#31290,#31291,#31292,#31293,#31294,#31295,
#31296,#31297,#31298,#31299,#31300,#31301,#31302,#31303,#31304,#31305,#31306,
#31307,#31308,#31309,#31310,#31311,#31312,#31313,#31314,#31315,#31316,#31317,
#31318,#31319,#31320,#31321,#31322,#31323,#31324,#31325,#31326,#31327,#31328,
#31329,#31330,#31331,#31332,#31333,#31334,#31335,#31336,#31337,#31338,#31339,
#31340,#31341,#31342,#31343,#31344,#31345,#31346,#31347,#31348,#31349,#31350,
#31351,#31352,#31353,#31354,#31355,#31356),(#31357,#31358,#31359,#31360,
#31361,#31362,#31363,#31364,#31365,#31366,#31367,#31368,#31369,#31370,#31371,
#31372,#31373,#31374,#31375,#31376,#31377,#31378,#31379,#31380,#31381,#31382,
#31383,#31384,#31385,#31386,#31387,#31388,#31389,#31390,#31391,#31392,#31393,
#31394,#31395,#31396,#31397,#31398,#31399,#31400,#31401,#31402,#31403,#31404,
#31405,#31406,#31407,#31408,#31409,#31410,#31411,#31412,#31413,#31414,#31415,
#31416,#31417,#31418,#31419,#31420,#31421,#31422,#31423,#31424,#31425,#31426,
#31427,#31428,#31429,#31430,#31431,#31432,#31433,#31434,#31435,#31436,#31437,
#31438,#31439,#31440,#31441,#31442,#31443,#31444,#31445,#31446,#31447,#31448,
#31449,#31450,#31451,#31452,#31453,#31454,#31455,#31456,#31457,#31458,#31459,
#31460),(#31461,#31462,#31463,#31464,#31465,#31466,#31467,#31468,#31469,
#31470,#31471,#31472,#31473,#31474,#31475,#31476,#31477,#31478,#31479,#31480,
#31481,#31482,#31483,#31484,#31485,#31486,#31487,#31488,#31489,#31490,#31491,
#31492,#31493,#31494,#31495,#31496,#31497,#31498,#31499,#31500,#31501,#31502,
#31503,#31504,#31505,#31506,#31507,#31508,#31509,#31510,#31511,#31512,#31513,
#31514,#31515,#31516,#31517,#31518,#31519,#31520,#31521,#31522,#31523,#31524,
#31525,#31526,#31527,#31528,#31529,#31530,#31531,#31532,#31533,#31534,#31535,
#31536,#31537,#31538,#31539,#31540,#31541,#31542,#31543,#31544,#31545,#31546,
#31547,#31548,#31549,#31550,#31551,#31552,#31553,#31554,#31555,#31556,#31557,
#31558,#31559,#31560,#31561,#31562,#31563,#31564)),.UNSPECIFIED.,.F.,.F.,
 .F.,(4,4),(4,1,1,1,1,1,1,1,1,1,1,1,1,1,1,1,1,1,1,1,1,1,1,1,1,1,1,1,1,1,
1,1,1,1,1,1,1,1,1,1,1,1,1,1,1,1,1,1,1,1,1,1,1,1,1,1,1,1,1,1,1,1,1,1,1,1,
1,1,1,1,1,1,1,1,1,1,1,1,1,1,1,1,1,1,1,1,1,1,1,1,1,1,1,1,1,1,1,1,1,1,1,4),
(0.,0.0448889834294935),(11.8615800042566,12.8591085386932,13.8566370731298,
14.8541656075664,15.851694142003,16.8492226764396,17.8467512108762,18.8442797453128,
19.8418082797494,20.839336814186,21.8368653486226,22.8343938830592,23.8319224174958,
24.8294509519324,25.826979486369,26.8245080208056,27.8220365552422,28.8195650896788,
29.8170936241154,30.814622158552,31.8121506929886,32.8096792274252,33.8072077618618,
34.8047362962984,35.802264830735,36.7997933651716,37.7973218996082,38.7948504340448,
39.7923789684814,40.789907502918,41.7874360373546,42.7849645717912,43.7824931062278,
44.7800216406644,45.777550175101,46.7750787095376,47.7726072439742,48.7701357784108,
49.7676643128474,50.765192847284,51.7627213817206,52.7602499161572,53.7577784505938,
54.7553069850304,55.752835519467,56.7503640539036,57.7478925883402,58.7454211227768,
59.7429496572134,60.74047819165,61.7380067260866,62.7355352605232,63.7330637949598,
64.7305923293964,65.728120863833,66.7256493982696,67.7231779327062,68.7207064671428,
69.7182350015794,70.715763536016,71.7132920704526,72.7108206048892,73.7083491393258,
74.7058776737624,75.703406208199,76.7009347426356,77.6984632770722,78.6959918115088,
79.6935203459454,80.691048880382,81.6885774148186,82.6861059492552,83.6836344836918,
84.6811630181284,85.678691552565,86.6762200870016,87.6737486214382,88.6712771558748,
89.6688056903114,90.666334224748,91.6638627591846,92.6613912936212,93.6589198280578,
94.6564483624944,95.653976896931,96.6515054313676,97.6490339658042,98.6465625002408,
99.6440910346774,100.641619569114,101.639148103551,102.636676637987,103.634205172424,
104.63173370686,105.629262241297,106.626790775734,107.62431931017,108.621847844607,
109.619376379043,110.61690491348,111.614433447917,112.611961982353),
 .UNSPECIFIED.);
#592=B_SPLINE_SURFACE_WITH_KNOTS('',3,3,((#31672,#31673,#31674,#31675,#31676,
#31677,#31678,#31679,#31680,#31681,#31682,#31683,#31684,#31685,#31686,#31687,
#31688,#31689,#31690,#31691,#31692,#31693,#31694,#31695,#31696,#31697,#31698,
#31699,#31700,#31701,#31702,#31703,#31704,#31705,#31706,#31707,#31708,#31709,
#31710,#31711,#31712,#31713,#31714,#31715,#31716,#31717,#31718,#31719,#31720,
#31721,#31722,#31723,#31724,#31725,#31726,#31727,#31728,#31729,#31730,#31731,
#31732,#31733,#31734,#31735,#31736,#31737,#31738,#31739,#31740,#31741,#31742,
#31743,#31744,#31745,#31746,#31747,#31748,#31749,#31750,#31751,#31752,#31753,
#31754,#31755,#31756,#31757,#31758,#31759,#31760,#31761,#31762,#31763,#31764,
#31765,#31766,#31767,#31768,#31769,#31770,#31771,#31772,#31773,#31774,#31775),
(#31776,#31777,#31778,#31779,#31780,#31781,#31782,#31783,#31784,#31785,
#31786,#31787,#31788,#31789,#31790,#31791,#31792,#31793,#31794,#31795,#31796,
#31797,#31798,#31799,#31800,#31801,#31802,#31803,#31804,#31805,#31806,#31807,
#31808,#31809,#31810,#31811,#31812,#31813,#31814,#31815,#31816,#31817,#31818,
#31819,#31820,#31821,#31822,#31823,#31824,#31825,#31826,#31827,#31828,#31829,
#31830,#31831,#31832,#31833,#31834,#31835,#31836,#31837,#31838,#31839,#31840,
#31841,#31842,#31843,#31844,#31845,#31846,#31847,#31848,#31849,#31850,#31851,
#31852,#31853,#31854,#31855,#31856,#31857,#31858,#31859,#31860,#31861,#31862,
#31863,#31864,#31865,#31866,#31867,#31868,#31869,#31870,#31871,#31872,#31873,
#31874,#31875,#31876,#31877,#31878,#31879),(#31880,#31881,#31882,#31883,
#31884,#31885,#31886,#31887,#31888,#31889,#31890,#31891,#31892,#31893,#31894,
#31895,#31896,#31897,#31898,#31899,#31900,#31901,#31902,#31903,#31904,#31905,
#31906,#31907,#31908,#31909,#31910,#31911,#31912,#31913,#31914,#31915,#31916,
#31917,#31918,#31919,#31920,#31921,#31922,#31923,#31924,#31925,#31926,#31927,
#31928,#31929,#31930,#31931,#31932,#31933,#31934,#31935,#31936,#31937,#31938,
#31939,#31940,#31941,#31942,#31943,#31944,#31945,#31946,#31947,#31948,#31949,
#31950,#31951,#31952,#31953,#31954,#31955,#31956,#31957,#31958,#31959,#31960,
#31961,#31962,#31963,#31964,#31965,#31966,#31967,#31968,#31969,#31970,#31971,
#31972,#31973,#31974,#31975,#31976,#31977,#31978,#31979,#31980,#31981,#31982,
#31983),(#31984,#31985,#31986,#31987,#31988,#31989,#31990,#31991,#31992,
#31993,#31994,#31995,#31996,#31997,#31998,#31999,#32000,#32001,#32002,#32003,
#32004,#32005,#32006,#32007,#32008,#32009,#32010,#32011,#32012,#32013,#32014,
#32015,#32016,#32017,#32018,#32019,#32020,#32021,#32022,#32023,#32024,#32025,
#32026,#32027,#32028,#32029,#32030,#32031,#32032,#32033,#32034,#32035,#32036,
#32037,#32038,#32039,#32040,#32041,#32042,#32043,#32044,#32045,#32046,#32047,
#32048,#32049,#32050,#32051,#32052,#32053,#32054,#32055,#32056,#32057,#32058,
#32059,#32060,#32061,#32062,#32063,#32064,#32065,#32066,#32067,#32068,#32069,
#32070,#32071,#32072,#32073,#32074,#32075,#32076,#32077,#32078,#32079,#32080,
#32081,#32082,#32083,#32084,#32085,#32086,#32087)),.UNSPECIFIED.,.F.,.F.,
 .F.,(4,4),(4,1,1,1,1,1,1,1,1,1,1,1,1,1,1,1,1,1,1,1,1,1,1,1,1,1,1,1,1,1,
1,1,1,1,1,1,1,1,1,1,1,1,1,1,1,1,1,1,1,1,1,1,1,1,1,1,1,1,1,1,1,1,1,1,1,1,
1,1,1,1,1,1,1,1,1,1,1,1,1,1,1,1,1,1,1,1,1,1,1,1,1,1,1,1,1,1,1,1,1,1,1,4),
(0.,0.0448889834294935),(14.3981410127769,15.3956695472135,16.3931980816501,
17.3907266160867,18.3882551505233,19.3857836849599,20.3833122193965,21.3808407538331,
22.3783692882697,23.3758978227063,24.3734263571429,25.3709548915795,26.3684834260161,
27.3660119604527,28.3635404948893,29.3610690293259,30.3585975637625,31.3561260981991,
32.3536546326357,33.3511831670723,34.3487117015089,35.3462402359455,36.3437687703821,
37.3412973048187,38.3388258392553,39.3363543736919,40.3338829081285,41.3314114425651,
42.3289399770017,43.3264685114383,44.3239970458749,45.3215255803115,46.3190541147481,
47.3165826491847,48.3141111836213,49.3116397180578,50.3091682524944,51.3066967869311,
52.3042253213677,53.3017538558043,54.2992823902408,55.2968109246774,56.294339459114,
57.2918679935507,58.2893965279873,59.2869250624238,60.2844535968604,61.281982131297,
62.2795106657336,63.2770392001703,64.2745677346068,65.2720962690434,66.26962480348,
67.2671533379166,68.2646818723533,69.2622104067898,70.2597389412264,71.257267475663,
72.2547960100996,73.2523245445362,74.2498530789728,75.2473816134094,76.244910147846,
77.2424386822826,78.2399672167192,79.2374957511558,80.2350242855924,81.232552820029,
82.2300813544656,83.2276098889022,84.2251384233388,85.2226669577754,86.220195492212,
87.2177240266486,88.2152525610852,89.2127810955218,90.2103096299584,91.207838164395,
92.2053666988316,93.2028952332682,94.2004237677048,95.1979523021414,96.195480836578,
97.1930093710146,98.1905379054512,99.1880664398878,100.185594974324,101.183123508761,
102.180652043198,103.178180577634,104.175709112071,105.173237646507,106.170766180944,
107.168294715381,108.165823249817,109.163351784254,110.16088031869,111.158408853127,
112.155937387564,113.153465922,114.150994456437,115.148522990873),
 .UNSPECIFIED.);
#593=B_SPLINE_SURFACE_WITH_KNOTS('',3,3,((#32392,#32393,#32394,#32395,#32396,
#32397,#32398,#32399,#32400,#32401,#32402,#32403,#32404,#32405,#32406,#32407,
#32408,#32409,#32410,#32411,#32412,#32413,#32414,#32415,#32416,#32417,#32418,
#32419,#32420,#32421,#32422,#32423,#32424,#32425,#32426,#32427,#32428,#32429,
#32430,#32431,#32432,#32433,#32434,#32435,#32436,#32437,#32438,#32439,#32440,
#32441,#32442,#32443,#32444,#32445,#32446,#32447,#32448,#32449,#32450,#32451,
#32452,#32453,#32454,#32455,#32456,#32457,#32458,#32459,#32460,#32461,#32462,
#32463,#32464,#32465,#32466,#32467,#32468,#32469,#32470,#32471,#32472,#32473,
#32474,#32475,#32476,#32477,#32478,#32479,#32480,#32481,#32482,#32483,#32484,
#32485,#32486,#32487,#32488,#32489,#32490,#32491,#32492,#32493,#32494,#32495),
(#32496,#32497,#32498,#32499,#32500,#32501,#32502,#32503,#32504,#32505,
#32506,#32507,#32508,#32509,#32510,#32511,#32512,#32513,#32514,#32515,#32516,
#32517,#32518,#32519,#32520,#32521,#32522,#32523,#32524,#32525,#32526,#32527,
#32528,#32529,#32530,#32531,#32532,#32533,#32534,#32535,#32536,#32537,#32538,
#32539,#32540,#32541,#32542,#32543,#32544,#32545,#32546,#32547,#32548,#32549,
#32550,#32551,#32552,#32553,#32554,#32555,#32556,#32557,#32558,#32559,#32560,
#32561,#32562,#32563,#32564,#32565,#32566,#32567,#32568,#32569,#32570,#32571,
#32572,#32573,#32574,#32575,#32576,#32577,#32578,#32579,#32580,#32581,#32582,
#32583,#32584,#32585,#32586,#32587,#32588,#32589,#32590,#32591,#32592,#32593,
#32594,#32595,#32596,#32597,#32598,#32599),(#32600,#32601,#32602,#32603,
#32604,#32605,#32606,#32607,#32608,#32609,#32610,#32611,#32612,#32613,#32614,
#32615,#32616,#32617,#32618,#32619,#32620,#32621,#32622,#32623,#32624,#32625,
#32626,#32627,#32628,#32629,#32630,#32631,#32632,#32633,#32634,#32635,#32636,
#32637,#32638,#32639,#32640,#32641,#32642,#32643,#32644,#32645,#32646,#32647,
#32648,#32649,#32650,#32651,#32652,#32653,#32654,#32655,#32656,#32657,#32658,
#32659,#32660,#32661,#32662,#32663,#32664,#32665,#32666,#32667,#32668,#32669,
#32670,#32671,#32672,#32673,#32674,#32675,#32676,#32677,#32678,#32679,#32680,
#32681,#32682,#32683,#32684,#32685,#32686,#32687,#32688,#32689,#32690,#32691,
#32692,#32693,#32694,#32695,#32696,#32697,#32698,#32699,#32700,#32701,#32702,
#32703),(#32704,#32705,#32706,#32707,#32708,#32709,#32710,#32711,#32712,
#32713,#32714,#32715,#32716,#32717,#32718,#32719,#32720,#32721,#32722,#32723,
#32724,#32725,#32726,#32727,#32728,#32729,#32730,#32731,#32732,#32733,#32734,
#32735,#32736,#32737,#32738,#32739,#32740,#32741,#32742,#32743,#32744,#32745,
#32746,#32747,#32748,#32749,#32750,#32751,#32752,#32753,#32754,#32755,#32756,
#32757,#32758,#32759,#32760,#32761,#32762,#32763,#32764,#32765,#32766,#32767,
#32768,#32769,#32770,#32771,#32772,#32773,#32774,#32775,#32776,#32777,#32778,
#32779,#32780,#32781,#32782,#32783,#32784,#32785,#32786,#32787,#32788,#32789,
#32790,#32791,#32792,#32793,#32794,#32795,#32796,#32797,#32798,#32799,#32800,
#32801,#32802,#32803,#32804,#32805,#32806,#32807)),.UNSPECIFIED.,.F.,.F.,
 .F.,(4,4),(4,1,1,1,1,1,1,1,1,1,1,1,1,1,1,1,1,1,1,1,1,1,1,1,1,1,1,1,1,1,
1,1,1,1,1,1,1,1,1,1,1,1,1,1,1,1,1,1,1,1,1,1,1,1,1,1,1,1,1,1,1,1,1,1,1,1,
1,1,1,1,1,1,1,1,1,1,1,1,1,1,1,1,1,1,1,1,1,1,1,1,1,1,1,1,1,1,1,1,1,1,1,4),
(0.,0.0448889834294935),(11.8615800042566,12.8591085386932,13.8566370731298,
14.8541656075664,15.851694142003,16.8492226764396,17.8467512108762,18.8442797453128,
19.8418082797494,20.839336814186,21.8368653486226,22.8343938830592,23.8319224174958,
24.8294509519324,25.826979486369,26.8245080208056,27.8220365552422,28.8195650896788,
29.8170936241154,30.814622158552,31.8121506929886,32.8096792274252,33.8072077618618,
34.8047362962984,35.802264830735,36.7997933651716,37.7973218996082,38.7948504340448,
39.7923789684814,40.789907502918,41.7874360373546,42.7849645717912,43.7824931062278,
44.7800216406644,45.777550175101,46.7750787095376,47.7726072439742,48.7701357784108,
49.7676643128474,50.765192847284,51.7627213817206,52.7602499161572,53.7577784505938,
54.7553069850304,55.752835519467,56.7503640539036,57.7478925883402,58.7454211227768,
59.7429496572134,60.74047819165,61.7380067260866,62.7355352605232,63.7330637949598,
64.7305923293964,65.728120863833,66.7256493982696,67.7231779327062,68.7207064671428,
69.7182350015794,70.715763536016,71.7132920704526,72.7108206048892,73.7083491393258,
74.7058776737624,75.703406208199,76.7009347426356,77.6984632770722,78.6959918115088,
79.6935203459454,80.691048880382,81.6885774148186,82.6861059492552,83.6836344836918,
84.6811630181284,85.678691552565,86.6762200870016,87.6737486214382,88.6712771558748,
89.6688056903114,90.666334224748,91.6638627591846,92.6613912936212,93.6589198280578,
94.6564483624944,95.653976896931,96.6515054313676,97.6490339658042,98.6465625002408,
99.6440910346774,100.641619569114,101.639148103551,102.636676637987,103.634205172424,
104.63173370686,105.629262241297,106.626790775734,107.62431931017,108.621847844607,
109.619376379043,110.61690491348,111.614433447917,112.611961982353),
 .UNSPECIFIED.);
#594=B_SPLINE_SURFACE_WITH_KNOTS('',3,3,((#32915,#32916,#32917,#32918,#32919,
#32920,#32921,#32922,#32923,#32924,#32925,#32926,#32927,#32928,#32929,#32930,
#32931,#32932,#32933,#32934,#32935,#32936,#32937,#32938,#32939,#32940,#32941,
#32942,#32943,#32944,#32945,#32946,#32947,#32948,#32949,#32950,#32951,#32952,
#32953,#32954,#32955,#32956,#32957,#32958,#32959,#32960,#32961,#32962,#32963,
#32964,#32965,#32966,#32967,#32968,#32969,#32970,#32971,#32972,#32973,#32974,
#32975,#32976,#32977,#32978,#32979,#32980,#32981,#32982,#32983,#32984,#32985,
#32986,#32987,#32988,#32989,#32990,#32991,#32992,#32993,#32994,#32995,#32996,
#32997,#32998,#32999,#33000,#33001,#33002,#33003,#33004,#33005,#33006,#33007,
#33008,#33009,#33010,#33011,#33012,#33013,#33014,#33015,#33016,#33017,#33018),
(#33019,#33020,#33021,#33022,#33023,#33024,#33025,#33026,#33027,#33028,
#33029,#33030,#33031,#33032,#33033,#33034,#33035,#33036,#33037,#33038,#33039,
#33040,#33041,#33042,#33043,#33044,#33045,#33046,#33047,#33048,#33049,#33050,
#33051,#33052,#33053,#33054,#33055,#33056,#33057,#33058,#33059,#33060,#33061,
#33062,#33063,#33064,#33065,#33066,#33067,#33068,#33069,#33070,#33071,#33072,
#33073,#33074,#33075,#33076,#33077,#33078,#33079,#33080,#33081,#33082,#33083,
#33084,#33085,#33086,#33087,#33088,#33089,#33090,#33091,#33092,#33093,#33094,
#33095,#33096,#33097,#33098,#33099,#33100,#33101,#33102,#33103,#33104,#33105,
#33106,#33107,#33108,#33109,#33110,#33111,#33112,#33113,#33114,#33115,#33116,
#33117,#33118,#33119,#33120,#33121,#33122),(#33123,#33124,#33125,#33126,
#33127,#33128,#33129,#33130,#33131,#33132,#33133,#33134,#33135,#33136,#33137,
#33138,#33139,#33140,#33141,#33142,#33143,#33144,#33145,#33146,#33147,#33148,
#33149,#33150,#33151,#33152,#33153,#33154,#33155,#33156,#33157,#33158,#33159,
#33160,#33161,#33162,#33163,#33164,#33165,#33166,#33167,#33168,#33169,#33170,
#33171,#33172,#33173,#33174,#33175,#33176,#33177,#33178,#33179,#33180,#33181,
#33182,#33183,#33184,#33185,#33186,#33187,#33188,#33189,#33190,#33191,#33192,
#33193,#33194,#33195,#33196,#33197,#33198,#33199,#33200,#33201,#33202,#33203,
#33204,#33205,#33206,#33207,#33208,#33209,#33210,#33211,#33212,#33213,#33214,
#33215,#33216,#33217,#33218,#33219,#33220,#33221,#33222,#33223,#33224,#33225,
#33226),(#33227,#33228,#33229,#33230,#33231,#33232,#33233,#33234,#33235,
#33236,#33237,#33238,#33239,#33240,#33241,#33242,#33243,#33244,#33245,#33246,
#33247,#33248,#33249,#33250,#33251,#33252,#33253,#33254,#33255,#33256,#33257,
#33258,#33259,#33260,#33261,#33262,#33263,#33264,#33265,#33266,#33267,#33268,
#33269,#33270,#33271,#33272,#33273,#33274,#33275,#33276,#33277,#33278,#33279,
#33280,#33281,#33282,#33283,#33284,#33285,#33286,#33287,#33288,#33289,#33290,
#33291,#33292,#33293,#33294,#33295,#33296,#33297,#33298,#33299,#33300,#33301,
#33302,#33303,#33304,#33305,#33306,#33307,#33308,#33309,#33310,#33311,#33312,
#33313,#33314,#33315,#33316,#33317,#33318,#33319,#33320,#33321,#33322,#33323,
#33324,#33325,#33326,#33327,#33328,#33329,#33330)),.UNSPECIFIED.,.F.,.F.,
 .F.,(4,4),(4,1,1,1,1,1,1,1,1,1,1,1,1,1,1,1,1,1,1,1,1,1,1,1,1,1,1,1,1,1,
1,1,1,1,1,1,1,1,1,1,1,1,1,1,1,1,1,1,1,1,1,1,1,1,1,1,1,1,1,1,1,1,1,1,1,1,
1,1,1,1,1,1,1,1,1,1,1,1,1,1,1,1,1,1,1,1,1,1,1,1,1,1,1,1,1,1,1,1,1,1,1,4),
(0.,0.0448889834294935),(14.3981410127769,15.3956695472135,16.3931980816501,
17.3907266160867,18.3882551505233,19.3857836849599,20.3833122193965,21.3808407538331,
22.3783692882697,23.3758978227063,24.3734263571429,25.3709548915795,26.3684834260161,
27.3660119604527,28.3635404948893,29.3610690293259,30.3585975637625,31.3561260981991,
32.3536546326357,33.3511831670723,34.3487117015089,35.3462402359455,36.3437687703821,
37.3412973048187,38.3388258392553,39.3363543736919,40.3338829081285,41.3314114425651,
42.3289399770017,43.3264685114383,44.3239970458749,45.3215255803115,46.3190541147481,
47.3165826491847,48.3141111836213,49.3116397180579,50.3091682524945,51.3066967869311,
52.3042253213677,53.3017538558043,54.2992823902409,55.2968109246775,56.2943394591141,
57.2918679935507,58.2893965279873,59.2869250624239,60.2844535968605,61.2819821312971,
62.2795106657337,63.2770392001703,64.2745677346069,65.2720962690435,66.2696248034801,
67.2671533379167,68.2646818723533,69.2622104067899,70.2597389412265,71.2572674756631,
72.2547960100997,73.2523245445363,74.2498530789729,75.2473816134095,76.2449101478461,
77.2424386822827,78.2399672167193,79.2374957511559,80.2350242855925,81.2325528200291,
82.2300813544657,83.2276098889023,84.2251384233389,85.2226669577755,86.2201954922121,
87.2177240266487,88.2152525610853,89.2127810955219,90.2103096299585,91.2078381643951,
92.2053666988317,93.2028952332683,94.2004237677049,95.1979523021415,96.1954808365781,
97.1930093710147,98.1905379054513,99.1880664398879,100.185594974324,101.183123508761,
102.180652043198,103.178180577634,104.175709112071,105.173237646507,106.170766180944,
107.168294715381,108.165823249817,109.163351784254,110.16088031869,111.158408853127,
112.155937387564,113.153465922,114.150994456437,115.148522990873),
 .UNSPECIFIED.);
#595=B_SPLINE_SURFACE_WITH_KNOTS('',3,3,((#33635,#33636,#33637,#33638,#33639,
#33640,#33641,#33642,#33643,#33644,#33645,#33646,#33647,#33648,#33649,#33650,
#33651,#33652,#33653,#33654,#33655,#33656,#33657,#33658,#33659,#33660,#33661,
#33662,#33663,#33664,#33665,#33666,#33667,#33668,#33669,#33670,#33671,#33672,
#33673,#33674,#33675,#33676,#33677,#33678,#33679,#33680,#33681,#33682,#33683,
#33684,#33685,#33686,#33687,#33688,#33689,#33690,#33691,#33692,#33693,#33694,
#33695,#33696,#33697,#33698,#33699,#33700,#33701,#33702,#33703,#33704,#33705,
#33706,#33707,#33708,#33709,#33710,#33711,#33712,#33713,#33714,#33715,#33716,
#33717,#33718,#33719,#33720,#33721,#33722,#33723,#33724,#33725,#33726,#33727,
#33728,#33729,#33730,#33731,#33732,#33733,#33734,#33735,#33736,#33737,#33738),
(#33739,#33740,#33741,#33742,#33743,#33744,#33745,#33746,#33747,#33748,
#33749,#33750,#33751,#33752,#33753,#33754,#33755,#33756,#33757,#33758,#33759,
#33760,#33761,#33762,#33763,#33764,#33765,#33766,#33767,#33768,#33769,#33770,
#33771,#33772,#33773,#33774,#33775,#33776,#33777,#33778,#33779,#33780,#33781,
#33782,#33783,#33784,#33785,#33786,#33787,#33788,#33789,#33790,#33791,#33792,
#33793,#33794,#33795,#33796,#33797,#33798,#33799,#33800,#33801,#33802,#33803,
#33804,#33805,#33806,#33807,#33808,#33809,#33810,#33811,#33812,#33813,#33814,
#33815,#33816,#33817,#33818,#33819,#33820,#33821,#33822,#33823,#33824,#33825,
#33826,#33827,#33828,#33829,#33830,#33831,#33832,#33833,#33834,#33835,#33836,
#33837,#33838,#33839,#33840,#33841,#33842),(#33843,#33844,#33845,#33846,
#33847,#33848,#33849,#33850,#33851,#33852,#33853,#33854,#33855,#33856,#33857,
#33858,#33859,#33860,#33861,#33862,#33863,#33864,#33865,#33866,#33867,#33868,
#33869,#33870,#33871,#33872,#33873,#33874,#33875,#33876,#33877,#33878,#33879,
#33880,#33881,#33882,#33883,#33884,#33885,#33886,#33887,#33888,#33889,#33890,
#33891,#33892,#33893,#33894,#33895,#33896,#33897,#33898,#33899,#33900,#33901,
#33902,#33903,#33904,#33905,#33906,#33907,#33908,#33909,#33910,#33911,#33912,
#33913,#33914,#33915,#33916,#33917,#33918,#33919,#33920,#33921,#33922,#33923,
#33924,#33925,#33926,#33927,#33928,#33929,#33930,#33931,#33932,#33933,#33934,
#33935,#33936,#33937,#33938,#33939,#33940,#33941,#33942,#33943,#33944,#33945,
#33946),(#33947,#33948,#33949,#33950,#33951,#33952,#33953,#33954,#33955,
#33956,#33957,#33958,#33959,#33960,#33961,#33962,#33963,#33964,#33965,#33966,
#33967,#33968,#33969,#33970,#33971,#33972,#33973,#33974,#33975,#33976,#33977,
#33978,#33979,#33980,#33981,#33982,#33983,#33984,#33985,#33986,#33987,#33988,
#33989,#33990,#33991,#33992,#33993,#33994,#33995,#33996,#33997,#33998,#33999,
#34000,#34001,#34002,#34003,#34004,#34005,#34006,#34007,#34008,#34009,#34010,
#34011,#34012,#34013,#34014,#34015,#34016,#34017,#34018,#34019,#34020,#34021,
#34022,#34023,#34024,#34025,#34026,#34027,#34028,#34029,#34030,#34031,#34032,
#34033,#34034,#34035,#34036,#34037,#34038,#34039,#34040,#34041,#34042,#34043,
#34044,#34045,#34046,#34047,#34048,#34049,#34050)),.UNSPECIFIED.,.F.,.F.,
 .F.,(4,4),(4,1,1,1,1,1,1,1,1,1,1,1,1,1,1,1,1,1,1,1,1,1,1,1,1,1,1,1,1,1,
1,1,1,1,1,1,1,1,1,1,1,1,1,1,1,1,1,1,1,1,1,1,1,1,1,1,1,1,1,1,1,1,1,1,1,1,
1,1,1,1,1,1,1,1,1,1,1,1,1,1,1,1,1,1,1,1,1,1,1,1,1,1,1,1,1,1,1,1,1,1,1,4),
(0.,0.0448889834294935),(11.8615800042566,12.8591085386932,13.8566370731298,
14.8541656075664,15.851694142003,16.8492226764396,17.8467512108762,18.8442797453128,
19.8418082797494,20.839336814186,21.8368653486226,22.8343938830592,23.8319224174958,
24.8294509519324,25.826979486369,26.8245080208056,27.8220365552422,28.8195650896788,
29.8170936241154,30.814622158552,31.8121506929886,32.8096792274252,33.8072077618618,
34.8047362962984,35.802264830735,36.7997933651716,37.7973218996082,38.7948504340448,
39.7923789684814,40.789907502918,41.7874360373546,42.7849645717912,43.7824931062278,
44.7800216406644,45.777550175101,46.7750787095376,47.7726072439742,48.7701357784108,
49.7676643128474,50.765192847284,51.7627213817206,52.7602499161572,53.7577784505938,
54.7553069850304,55.752835519467,56.7503640539036,57.7478925883402,58.7454211227768,
59.7429496572134,60.74047819165,61.7380067260866,62.7355352605232,63.7330637949598,
64.7305923293964,65.728120863833,66.7256493982696,67.7231779327062,68.7207064671428,
69.7182350015794,70.715763536016,71.7132920704526,72.7108206048892,73.7083491393258,
74.7058776737624,75.703406208199,76.7009347426356,77.6984632770722,78.6959918115088,
79.6935203459454,80.691048880382,81.6885774148186,82.6861059492552,83.6836344836918,
84.6811630181284,85.678691552565,86.6762200870016,87.6737486214382,88.6712771558748,
89.6688056903114,90.666334224748,91.6638627591846,92.6613912936212,93.6589198280578,
94.6564483624944,95.653976896931,96.6515054313676,97.6490339658042,98.6465625002408,
99.6440910346774,100.641619569114,101.639148103551,102.636676637987,103.634205172424,
104.63173370686,105.629262241297,106.626790775734,107.62431931017,108.621847844607,
109.619376379043,110.61690491348,111.614433447917,112.611961982353),
 .UNSPECIFIED.);
#596=B_SPLINE_SURFACE_WITH_KNOTS('',3,3,((#34158,#34159,#34160,#34161,#34162,
#34163,#34164,#34165,#34166,#34167,#34168,#34169,#34170,#34171,#34172,#34173,
#34174,#34175,#34176,#34177,#34178,#34179,#34180,#34181,#34182,#34183,#34184,
#34185,#34186,#34187,#34188,#34189,#34190,#34191,#34192,#34193,#34194,#34195,
#34196,#34197,#34198,#34199,#34200,#34201,#34202,#34203,#34204,#34205,#34206,
#34207,#34208,#34209,#34210,#34211,#34212,#34213,#34214,#34215,#34216,#34217,
#34218,#34219,#34220,#34221,#34222,#34223,#34224,#34225,#34226,#34227,#34228,
#34229,#34230,#34231,#34232,#34233,#34234,#34235,#34236,#34237,#34238,#34239,
#34240,#34241,#34242,#34243,#34244,#34245,#34246,#34247,#34248,#34249,#34250,
#34251,#34252,#34253,#34254,#34255,#34256,#34257,#34258,#34259,#34260,#34261),
(#34262,#34263,#34264,#34265,#34266,#34267,#34268,#34269,#34270,#34271,
#34272,#34273,#34274,#34275,#34276,#34277,#34278,#34279,#34280,#34281,#34282,
#34283,#34284,#34285,#34286,#34287,#34288,#34289,#34290,#34291,#34292,#34293,
#34294,#34295,#34296,#34297,#34298,#34299,#34300,#34301,#34302,#34303,#34304,
#34305,#34306,#34307,#34308,#34309,#34310,#34311,#34312,#34313,#34314,#34315,
#34316,#34317,#34318,#34319,#34320,#34321,#34322,#34323,#34324,#34325,#34326,
#34327,#34328,#34329,#34330,#34331,#34332,#34333,#34334,#34335,#34336,#34337,
#34338,#34339,#34340,#34341,#34342,#34343,#34344,#34345,#34346,#34347,#34348,
#34349,#34350,#34351,#34352,#34353,#34354,#34355,#34356,#34357,#34358,#34359,
#34360,#34361,#34362,#34363,#34364,#34365),(#34366,#34367,#34368,#34369,
#34370,#34371,#34372,#34373,#34374,#34375,#34376,#34377,#34378,#34379,#34380,
#34381,#34382,#34383,#34384,#34385,#34386,#34387,#34388,#34389,#34390,#34391,
#34392,#34393,#34394,#34395,#34396,#34397,#34398,#34399,#34400,#34401,#34402,
#34403,#34404,#34405,#34406,#34407,#34408,#34409,#34410,#34411,#34412,#34413,
#34414,#34415,#34416,#34417,#34418,#34419,#34420,#34421,#34422,#34423,#34424,
#34425,#34426,#34427,#34428,#34429,#34430,#34431,#34432,#34433,#34434,#34435,
#34436,#34437,#34438,#34439,#34440,#34441,#34442,#34443,#34444,#34445,#34446,
#34447,#34448,#34449,#34450,#34451,#34452,#34453,#34454,#34455,#34456,#34457,
#34458,#34459,#34460,#34461,#34462,#34463,#34464,#34465,#34466,#34467,#34468,
#34469),(#34470,#34471,#34472,#34473,#34474,#34475,#34476,#34477,#34478,
#34479,#34480,#34481,#34482,#34483,#34484,#34485,#34486,#34487,#34488,#34489,
#34490,#34491,#34492,#34493,#34494,#34495,#34496,#34497,#34498,#34499,#34500,
#34501,#34502,#34503,#34504,#34505,#34506,#34507,#34508,#34509,#34510,#34511,
#34512,#34513,#34514,#34515,#34516,#34517,#34518,#34519,#34520,#34521,#34522,
#34523,#34524,#34525,#34526,#34527,#34528,#34529,#34530,#34531,#34532,#34533,
#34534,#34535,#34536,#34537,#34538,#34539,#34540,#34541,#34542,#34543,#34544,
#34545,#34546,#34547,#34548,#34549,#34550,#34551,#34552,#34553,#34554,#34555,
#34556,#34557,#34558,#34559,#34560,#34561,#34562,#34563,#34564,#34565,#34566,
#34567,#34568,#34569,#34570,#34571,#34572,#34573)),.UNSPECIFIED.,.F.,.F.,
 .F.,(4,4),(4,1,1,1,1,1,1,1,1,1,1,1,1,1,1,1,1,1,1,1,1,1,1,1,1,1,1,1,1,1,
1,1,1,1,1,1,1,1,1,1,1,1,1,1,1,1,1,1,1,1,1,1,1,1,1,1,1,1,1,1,1,1,1,1,1,1,
1,1,1,1,1,1,1,1,1,1,1,1,1,1,1,1,1,1,1,1,1,1,1,1,1,1,1,1,1,1,1,1,1,1,1,4),
(0.,0.0448889834294935),(14.3981410127769,15.3956695472135,16.3931980816501,
17.3907266160867,18.3882551505233,19.3857836849599,20.3833122193965,21.3808407538331,
22.3783692882697,23.3758978227063,24.3734263571429,25.3709548915795,26.3684834260161,
27.3660119604527,28.3635404948893,29.3610690293259,30.3585975637625,31.3561260981991,
32.3536546326357,33.3511831670723,34.3487117015089,35.3462402359455,36.3437687703821,
37.3412973048187,38.3388258392553,39.3363543736919,40.3338829081285,41.3314114425651,
42.3289399770017,43.3264685114383,44.3239970458749,45.3215255803115,46.3190541147481,
47.3165826491847,48.3141111836213,49.3116397180578,50.3091682524944,51.3066967869311,
52.3042253213677,53.3017538558043,54.2992823902408,55.2968109246774,56.294339459114,
57.2918679935507,58.2893965279873,59.2869250624238,60.2844535968604,61.281982131297,
62.2795106657336,63.2770392001703,64.2745677346068,65.2720962690434,66.26962480348,
67.2671533379166,68.2646818723533,69.2622104067898,70.2597389412264,71.257267475663,
72.2547960100996,73.2523245445362,74.2498530789728,75.2473816134094,76.244910147846,
77.2424386822826,78.2399672167192,79.2374957511558,80.2350242855924,81.232552820029,
82.2300813544656,83.2276098889022,84.2251384233388,85.2226669577754,86.220195492212,
87.2177240266486,88.2152525610852,89.2127810955218,90.2103096299584,91.207838164395,
92.2053666988316,93.2028952332682,94.2004237677048,95.1979523021414,96.195480836578,
97.1930093710146,98.1905379054512,99.1880664398878,100.185594974324,101.183123508761,
102.180652043198,103.178180577634,104.175709112071,105.173237646507,106.170766180944,
107.168294715381,108.165823249817,109.163351784254,110.16088031869,111.158408853127,
112.155937387564,113.153465922,114.150994456437,115.148522990873),
 .UNSPECIFIED.);
#597=B_SPLINE_SURFACE_WITH_KNOTS('',3,3,((#36638,#36639,#36640,#36641,#36642,
#36643,#36644,#36645,#36646,#36647,#36648,#36649,#36650,#36651,#36652,#36653,
#36654,#36655,#36656,#36657,#36658,#36659,#36660,#36661,#36662,#36663,#36664,
#36665,#36666,#36667,#36668,#36669,#36670,#36671,#36672,#36673,#36674,#36675,
#36676,#36677,#36678,#36679,#36680,#36681,#36682,#36683,#36684,#36685,#36686,
#36687,#36688,#36689,#36690,#36691,#36692,#36693,#36694,#36695,#36696,#36697,
#36698,#36699,#36700,#36701,#36702,#36703,#36704,#36705,#36706,#36707,#36708,
#36709,#36710,#36711,#36712,#36713,#36714,#36715,#36716,#36717,#36718,#36719,
#36720,#36721,#36722,#36723,#36724,#36725,#36726,#36727,#36728,#36729,#36730,
#36731,#36732,#36733,#36734,#36735,#36736,#36737,#36738,#36739,#36740,#36741,
#36742,#36743),(#36744,#36745,#36746,#36747,#36748,#36749,#36750,#36751,
#36752,#36753,#36754,#36755,#36756,#36757,#36758,#36759,#36760,#36761,#36762,
#36763,#36764,#36765,#36766,#36767,#36768,#36769,#36770,#36771,#36772,#36773,
#36774,#36775,#36776,#36777,#36778,#36779,#36780,#36781,#36782,#36783,#36784,
#36785,#36786,#36787,#36788,#36789,#36790,#36791,#36792,#36793,#36794,#36795,
#36796,#36797,#36798,#36799,#36800,#36801,#36802,#36803,#36804,#36805,#36806,
#36807,#36808,#36809,#36810,#36811,#36812,#36813,#36814,#36815,#36816,#36817,
#36818,#36819,#36820,#36821,#36822,#36823,#36824,#36825,#36826,#36827,#36828,
#36829,#36830,#36831,#36832,#36833,#36834,#36835,#36836,#36837,#36838,#36839,
#36840,#36841,#36842,#36843,#36844,#36845,#36846,#36847,#36848,#36849),
(#36850,#36851,#36852,#36853,#36854,#36855,#36856,#36857,#36858,#36859,
#36860,#36861,#36862,#36863,#36864,#36865,#36866,#36867,#36868,#36869,#36870,
#36871,#36872,#36873,#36874,#36875,#36876,#36877,#36878,#36879,#36880,#36881,
#36882,#36883,#36884,#36885,#36886,#36887,#36888,#36889,#36890,#36891,#36892,
#36893,#36894,#36895,#36896,#36897,#36898,#36899,#36900,#36901,#36902,#36903,
#36904,#36905,#36906,#36907,#36908,#36909,#36910,#36911,#36912,#36913,#36914,
#36915,#36916,#36917,#36918,#36919,#36920,#36921,#36922,#36923,#36924,#36925,
#36926,#36927,#36928,#36929,#36930,#36931,#36932,#36933,#36934,#36935,#36936,
#36937,#36938,#36939,#36940,#36941,#36942,#36943,#36944,#36945,#36946,#36947,
#36948,#36949,#36950,#36951,#36952,#36953,#36954,#36955),(#36956,#36957,
#36958,#36959,#36960,#36961,#36962,#36963,#36964,#36965,#36966,#36967,#36968,
#36969,#36970,#36971,#36972,#36973,#36974,#36975,#36976,#36977,#36978,#36979,
#36980,#36981,#36982,#36983,#36984,#36985,#36986,#36987,#36988,#36989,#36990,
#36991,#36992,#36993,#36994,#36995,#36996,#36997,#36998,#36999,#37000,#37001,
#37002,#37003,#37004,#37005,#37006,#37007,#37008,#37009,#37010,#37011,#37012,
#37013,#37014,#37015,#37016,#37017,#37018,#37019,#37020,#37021,#37022,#37023,
#37024,#37025,#37026,#37027,#37028,#37029,#37030,#37031,#37032,#37033,#37034,
#37035,#37036,#37037,#37038,#37039,#37040,#37041,#37042,#37043,#37044,#37045,
#37046,#37047,#37048,#37049,#37050,#37051,#37052,#37053,#37054,#37055,#37056,
#37057,#37058,#37059,#37060,#37061)),.UNSPECIFIED.,.F.,.F.,.F.,(4,4),(4,
1,1,1,1,1,1,1,1,1,1,1,1,1,1,1,1,1,1,1,1,1,1,1,1,1,1,1,1,1,1,1,1,1,1,1,1,
1,1,1,1,1,1,1,1,1,1,1,1,1,1,1,1,1,1,1,1,1,1,1,1,1,1,1,1,1,1,1,1,1,1,1,1,
1,1,1,1,1,1,1,1,1,1,1,1,1,1,1,1,1,1,1,1,1,1,1,1,1,1,1,1,1,1,4),(0.,0.0460148164544132),
(11.6154215191105,12.6127573616628,13.610093204215,14.6074290467673,15.6047648893195,
16.6021007318718,17.599436574424,18.5967724169762,19.5941082595285,20.5914441020807,
21.588779944633,22.5861157871852,23.5834516297375,24.5807874722897,25.5781233148419,
26.5754591573942,27.5727949999464,28.5701308424987,29.5674666850509,30.5648025276032,
31.5621383701554,32.5594742127077,33.5568100552599,34.5541458978121,35.5514817403644,
36.5488175829166,37.5461534254689,38.5434892680211,39.5408251105734,40.5381609531256,
41.5354967956779,42.5328326382301,43.5301684807823,44.5275043233346,45.5248401658868,
46.5221760084391,47.5195118509913,48.5168476935436,49.5141835360958,50.5115193786481,
51.5088552212003,52.5061910637525,53.5035269063048,54.500862748857,55.4981985914093,
56.4955344339615,57.4928702765138,58.490206119066,59.4875419616182,60.4848778041705,
61.4822136467227,62.479549489275,63.4768853318272,64.4742211743795,65.4715570169317,
66.468892859484,67.4662287020362,68.4635645445884,69.4609003871407,70.4582362296929,
71.4555720722452,72.4529079147974,73.4502437573497,74.4475795999019,75.4449154424541,
76.4422512850064,77.4395871275586,78.4369229701109,79.4342588126631,80.4315946552154,
81.4289304977676,82.4262663403199,83.4236021828721,84.4209380254243,85.4182738679766,
86.4156097105288,87.4129455530811,88.4102813956333,89.4076172381856,90.4049530807378,
91.4022889232901,92.3996247658423,93.3969606083945,94.3942964509468,95.391632293499,
96.3889681360513,97.3863039786035,98.3836398211558,99.380975663708,100.37831150626,
101.375647348812,102.372983191365,103.370319033917,104.367654876469,105.364990719021,
106.362326561574,107.359662404126,108.356998246678,109.35433408923,110.351669931783,
111.349005774335,112.346341616887,113.343677459439,114.341013301992),
 .UNSPECIFIED.);
#598=B_SPLINE_SURFACE_WITH_KNOTS('',3,3,((#37181,#37182,#37183,#37184,#37185,
#37186,#37187,#37188,#37189,#37190,#37191,#37192,#37193,#37194,#37195,#37196,
#37197,#37198,#37199,#37200,#37201,#37202,#37203,#37204,#37205,#37206,#37207,
#37208,#37209,#37210,#37211,#37212,#37213,#37214,#37215,#37216,#37217,#37218,
#37219,#37220,#37221,#37222,#37223,#37224,#37225,#37226,#37227,#37228,#37229,
#37230,#37231,#37232,#37233,#37234,#37235,#37236,#37237,#37238,#37239,#37240,
#37241,#37242,#37243,#37244,#37245,#37246,#37247,#37248,#37249,#37250,#37251,
#37252,#37253,#37254,#37255,#37256,#37257,#37258,#37259,#37260,#37261,#37262,
#37263,#37264,#37265,#37266,#37267,#37268,#37269,#37270,#37271,#37272,#37273,
#37274,#37275,#37276,#37277,#37278,#37279,#37280,#37281,#37282,#37283,#37284,
#37285,#37286,#37287,#37288),(#37289,#37290,#37291,#37292,#37293,#37294,
#37295,#37296,#37297,#37298,#37299,#37300,#37301,#37302,#37303,#37304,#37305,
#37306,#37307,#37308,#37309,#37310,#37311,#37312,#37313,#37314,#37315,#37316,
#37317,#37318,#37319,#37320,#37321,#37322,#37323,#37324,#37325,#37326,#37327,
#37328,#37329,#37330,#37331,#37332,#37333,#37334,#37335,#37336,#37337,#37338,
#37339,#37340,#37341,#37342,#37343,#37344,#37345,#37346,#37347,#37348,#37349,
#37350,#37351,#37352,#37353,#37354,#37355,#37356,#37357,#37358,#37359,#37360,
#37361,#37362,#37363,#37364,#37365,#37366,#37367,#37368,#37369,#37370,#37371,
#37372,#37373,#37374,#37375,#37376,#37377,#37378,#37379,#37380,#37381,#37382,
#37383,#37384,#37385,#37386,#37387,#37388,#37389,#37390,#37391,#37392,#37393,
#37394,#37395,#37396),(#37397,#37398,#37399,#37400,#37401,#37402,#37403,
#37404,#37405,#37406,#37407,#37408,#37409,#37410,#37411,#37412,#37413,#37414,
#37415,#37416,#37417,#37418,#37419,#37420,#37421,#37422,#37423,#37424,#37425,
#37426,#37427,#37428,#37429,#37430,#37431,#37432,#37433,#37434,#37435,#37436,
#37437,#37438,#37439,#37440,#37441,#37442,#37443,#37444,#37445,#37446,#37447,
#37448,#37449,#37450,#37451,#37452,#37453,#37454,#37455,#37456,#37457,#37458,
#37459,#37460,#37461,#37462,#37463,#37464,#37465,#37466,#37467,#37468,#37469,
#37470,#37471,#37472,#37473,#37474,#37475,#37476,#37477,#37478,#37479,#37480,
#37481,#37482,#37483,#37484,#37485,#37486,#37487,#37488,#37489,#37490,#37491,
#37492,#37493,#37494,#37495,#37496,#37497,#37498,#37499,#37500,#37501,#37502,
#37503,#37504),(#37505,#37506,#37507,#37508,#37509,#37510,#37511,#37512,
#37513,#37514,#37515,#37516,#37517,#37518,#37519,#37520,#37521,#37522,#37523,
#37524,#37525,#37526,#37527,#37528,#37529,#37530,#37531,#37532,#37533,#37534,
#37535,#37536,#37537,#37538,#37539,#37540,#37541,#37542,#37543,#37544,#37545,
#37546,#37547,#37548,#37549,#37550,#37551,#37552,#37553,#37554,#37555,#37556,
#37557,#37558,#37559,#37560,#37561,#37562,#37563,#37564,#37565,#37566,#37567,
#37568,#37569,#37570,#37571,#37572,#37573,#37574,#37575,#37576,#37577,#37578,
#37579,#37580,#37581,#37582,#37583,#37584,#37585,#37586,#37587,#37588,#37589,
#37590,#37591,#37592,#37593,#37594,#37595,#37596,#37597,#37598,#37599,#37600,
#37601,#37602,#37603,#37604,#37605,#37606,#37607,#37608,#37609,#37610,#37611,
#37612)),.UNSPECIFIED.,.F.,.F.,.F.,(4,4),(4,1,1,1,1,1,1,1,1,1,1,1,1,1,1,
1,1,1,1,1,1,1,1,1,1,1,1,1,1,1,1,1,1,1,1,1,1,1,1,1,1,1,1,1,1,1,1,1,1,1,1,
1,1,1,1,1,1,1,1,1,1,1,1,1,1,1,1,1,1,1,1,1,1,1,1,1,1,1,1,1,1,1,1,1,1,1,1,
1,1,1,1,1,1,1,1,1,1,1,1,1,1,1,1,1,1,4),(0.,0.0460148164544132),(8.31058692273969,
9.30859389336977,10.3066008639999,11.30460783463,12.30261480526,13.3006217758901,
14.2986287465202,15.2966357171503,16.2946426877804,17.2926496584105,18.2906566290406,
19.2886635996707,20.2866705703008,21.2846775409308,22.2826845115609,23.280691482191,
24.2786984528211,25.2767054234512,26.2747123940813,27.2727193647114,28.2707263353415,
29.2687333059716,30.2667402766016,31.2647472472317,32.2627542178618,33.2607611884919,
34.258768159122,35.2567751297521,36.2547821003822,37.2527890710123,38.2507960416424,
39.2488030122724,40.2468099829025,41.2448169535326,42.2428239241627,43.2408308947928,
44.2388378654229,45.236844836053,46.2348518066831,47.2328587773132,48.2308657479432,
49.2288727185733,50.2268796892034,51.2248866598335,52.2228936304636,53.2209006010937,
54.2189075717238,55.2169145423539,56.214921512984,57.212928483614,58.2109354542441,
59.2089424248742,60.2069493955043,61.2049563661344,62.2029633367645,63.2009703073946,
64.1989772780247,65.1969842486548,66.1949912192848,67.1929981899149,68.191005160545,
69.1890121311751,70.1870191018052,71.1850260724353,72.1830330430654,73.1810400136955,
74.1790469843256,75.1770539549557,76.1750609255857,77.1730678962158,78.1710748668459,
79.169081837476,80.1670888081061,81.1650957787362,82.1631027493663,83.1611097199964,
84.1591166906264,85.1571236612565,86.1551306318866,87.1531376025167,88.1511445731468,
89.1491515437769,90.147158514407,91.1451654850371,92.1431724556672,93.1411794262973,
94.1391863969273,95.1371933675574,96.1352003381875,97.1332073088176,98.1312142794477,
99.1292212500778,100.127228220708,101.125235191338,102.123242161968,103.121249132598,
104.119256103228,105.117263073858,106.115270044488,107.113277015118,108.111283985749,
109.109290956379,110.107297927009,111.105304897639,112.103311868269,113.101318838899),
 .UNSPECIFIED.);
#599=B_SPLINE_SURFACE_WITH_KNOTS('',3,3,((#38873,#38874,#38875,#38876,#38877,
#38878,#38879,#38880,#38881,#38882,#38883,#38884,#38885,#38886,#38887,#38888,
#38889,#38890,#38891,#38892,#38893,#38894,#38895,#38896,#38897,#38898,#38899,
#38900,#38901,#38902,#38903,#38904,#38905,#38906,#38907,#38908,#38909,#38910,
#38911,#38912,#38913,#38914,#38915,#38916,#38917,#38918,#38919,#38920,#38921,
#38922,#38923,#38924,#38925,#38926,#38927,#38928,#38929,#38930,#38931,#38932,
#38933,#38934,#38935,#38936,#38937,#38938,#38939,#38940,#38941,#38942,#38943,
#38944,#38945,#38946,#38947,#38948,#38949),(#38950,#38951,#38952,#38953,
#38954,#38955,#38956,#38957,#38958,#38959,#38960,#38961,#38962,#38963,#38964,
#38965,#38966,#38967,#38968,#38969,#38970,#38971,#38972,#38973,#38974,#38975,
#38976,#38977,#38978,#38979,#38980,#38981,#38982,#38983,#38984,#38985,#38986,
#38987,#38988,#38989,#38990,#38991,#38992,#38993,#38994,#38995,#38996,#38997,
#38998,#38999,#39000,#39001,#39002,#39003,#39004,#39005,#39006,#39007,#39008,
#39009,#39010,#39011,#39012,#39013,#39014,#39015,#39016,#39017,#39018,#39019,
#39020,#39021,#39022,#39023,#39024,#39025,#39026),(#39027,#39028,#39029,
#39030,#39031,#39032,#39033,#39034,#39035,#39036,#39037,#39038,#39039,#39040,
#39041,#39042,#39043,#39044,#39045,#39046,#39047,#39048,#39049,#39050,#39051,
#39052,#39053,#39054,#39055,#39056,#39057,#39058,#39059,#39060,#39061,#39062,
#39063,#39064,#39065,#39066,#39067,#39068,#39069,#39070,#39071,#39072,#39073,
#39074,#39075,#39076,#39077,#39078,#39079,#39080,#39081,#39082,#39083,#39084,
#39085,#39086,#39087,#39088,#39089,#39090,#39091,#39092,#39093,#39094,#39095,
#39096,#39097,#39098,#39099,#39100,#39101,#39102,#39103),(#39104,#39105,
#39106,#39107,#39108,#39109,#39110,#39111,#39112,#39113,#39114,#39115,#39116,
#39117,#39118,#39119,#39120,#39121,#39122,#39123,#39124,#39125,#39126,#39127,
#39128,#39129,#39130,#39131,#39132,#39133,#39134,#39135,#39136,#39137,#39138,
#39139,#39140,#39141,#39142,#39143,#39144,#39145,#39146,#39147,#39148,#39149,
#39150,#39151,#39152,#39153,#39154,#39155,#39156,#39157,#39158,#39159,#39160,
#39161,#39162,#39163,#39164,#39165,#39166,#39167,#39168,#39169,#39170,#39171,
#39172,#39173,#39174,#39175,#39176,#39177,#39178,#39179,#39180)),
 .UNSPECIFIED.,.F.,.F.,.F.,(4,4),(4,1,1,1,1,1,1,1,1,1,1,1,1,1,1,1,1,1,1,
1,1,1,1,1,1,1,1,1,1,1,1,1,1,1,1,1,1,1,1,1,1,1,1,1,1,1,1,1,1,1,1,1,1,1,1,
1,1,1,1,1,1,1,1,1,1,1,1,1,1,1,1,1,1,1,4),(0.,0.0658467982010768),(11.6150328478182,
12.6023632471184,13.5896936464185,14.5770240457187,15.5643544450188,16.551684844319,
17.5390152436191,18.5263456429193,19.5136760422194,20.5010064415196,21.4883368408197,
22.4756672401199,23.46299763942,24.4503280387202,25.4376584380203,26.4249888373205,
27.4123192366206,28.3996496359208,29.3869800352209,30.3743104345211,31.3616408338212,
32.3489712331214,33.3363016324215,34.3236320317217,35.3109624310218,36.298292830322,
37.2856232296221,38.2729536289223,39.2602840282224,40.2476144275226,41.2349448268227,
42.2222752261229,43.209605625423,44.1969360247232,45.1842664240233,46.1715968233235,
47.1589272226236,48.1462576219238,49.1335880212239,50.1209184205241,51.1082488198242,
52.0955792191244,53.0829096184245,54.0702400177247,55.0575704170248,56.0449008163249,
57.0322312156251,58.0195616149252,59.0068920142254,59.9942224135255,60.9815528128257,
61.9688832121258,62.956213611426,63.9435440107261,64.9308744100263,65.9182048093264,
66.9055352086266,67.8928656079267,68.8801960072269,69.867526406527,70.8548568058272,
71.8421872051273,72.8295176044275,73.8168480037276,74.8041784030278,75.7915088023279,
76.7788392016281,77.7661696009282,78.7535000002284,79.7408303995285,80.7281607988287,
81.7154911981288,82.702821597429,83.6901519967291,84.6774823960293),
 .UNSPECIFIED.);
#600=B_SPLINE_SURFACE_WITH_KNOTS('',3,3,((#39309,#39310,#39311,#39312,#39313,
#39314,#39315,#39316,#39317,#39318,#39319,#39320,#39321,#39322,#39323,#39324,
#39325,#39326,#39327,#39328,#39329,#39330,#39331,#39332,#39333,#39334,#39335,
#39336,#39337,#39338,#39339,#39340,#39341,#39342,#39343,#39344,#39345,#39346,
#39347,#39348,#39349,#39350,#39351,#39352,#39353,#39354,#39355,#39356,#39357,
#39358,#39359,#39360,#39361,#39362,#39363,#39364,#39365,#39366,#39367,#39368,
#39369,#39370,#39371,#39372,#39373,#39374,#39375,#39376,#39377,#39378,#39379,
#39380,#39381,#39382,#39383,#39384,#39385,#39386,#39387),(#39388,#39389,
#39390,#39391,#39392,#39393,#39394,#39395,#39396,#39397,#39398,#39399,#39400,
#39401,#39402,#39403,#39404,#39405,#39406,#39407,#39408,#39409,#39410,#39411,
#39412,#39413,#39414,#39415,#39416,#39417,#39418,#39419,#39420,#39421,#39422,
#39423,#39424,#39425,#39426,#39427,#39428,#39429,#39430,#39431,#39432,#39433,
#39434,#39435,#39436,#39437,#39438,#39439,#39440,#39441,#39442,#39443,#39444,
#39445,#39446,#39447,#39448,#39449,#39450,#39451,#39452,#39453,#39454,#39455,
#39456,#39457,#39458,#39459,#39460,#39461,#39462,#39463,#39464,#39465,#39466),
(#39467,#39468,#39469,#39470,#39471,#39472,#39473,#39474,#39475,#39476,
#39477,#39478,#39479,#39480,#39481,#39482,#39483,#39484,#39485,#39486,#39487,
#39488,#39489,#39490,#39491,#39492,#39493,#39494,#39495,#39496,#39497,#39498,
#39499,#39500,#39501,#39502,#39503,#39504,#39505,#39506,#39507,#39508,#39509,
#39510,#39511,#39512,#39513,#39514,#39515,#39516,#39517,#39518,#39519,#39520,
#39521,#39522,#39523,#39524,#39525,#39526,#39527,#39528,#39529,#39530,#39531,
#39532,#39533,#39534,#39535,#39536,#39537,#39538,#39539,#39540,#39541,#39542,
#39543,#39544,#39545),(#39546,#39547,#39548,#39549,#39550,#39551,#39552,
#39553,#39554,#39555,#39556,#39557,#39558,#39559,#39560,#39561,#39562,#39563,
#39564,#39565,#39566,#39567,#39568,#39569,#39570,#39571,#39572,#39573,#39574,
#39575,#39576,#39577,#39578,#39579,#39580,#39581,#39582,#39583,#39584,#39585,
#39586,#39587,#39588,#39589,#39590,#39591,#39592,#39593,#39594,#39595,#39596,
#39597,#39598,#39599,#39600,#39601,#39602,#39603,#39604,#39605,#39606,#39607,
#39608,#39609,#39610,#39611,#39612,#39613,#39614,#39615,#39616,#39617,#39618,
#39619,#39620,#39621,#39622,#39623,#39624)),.UNSPECIFIED.,.F.,.F.,.F.,(4,
4),(4,1,1,1,1,1,1,1,1,1,1,1,1,1,1,1,1,1,1,1,1,1,1,1,1,1,1,1,1,1,1,1,1,1,
1,1,1,1,1,1,1,1,1,1,1,1,1,1,1,1,1,1,1,1,1,1,1,1,1,1,1,1,1,1,1,1,1,1,1,1,
1,1,1,1,1,1,4),(0.,0.0658467982010768),(8.30747755240104,9.2960444961263,
10.2846114398516,11.2731783835768,12.2617453273021,13.2503122710274,14.2388792147526,
15.2274461584779,16.2160131022032,17.2045800459284,18.1931469896537,19.181713933379,
20.1702808771042,21.1588478208295,22.1474147645547,23.13598170828,24.1245486520053,
25.1131155957305,26.1016825394558,27.0902494831811,28.0788164269063,29.0673833706316,
30.0559503143569,31.0445172580821,32.0330842018074,33.0216511455327,34.0102180892579,
34.9987850329832,35.9873519767085,36.9759189204337,37.964485864159,38.9530528078842,
39.9416197516095,40.9301866953348,41.91875363906,42.9073205827853,43.8958875265106,
44.8844544702358,45.8730214139611,46.8615883576864,47.8501553014116,48.8387222451369,
49.8272891888622,50.8158561325874,51.8044230763127,52.792990020038,53.7815569637632,
54.7701239074885,55.7586908512138,56.747257794939,57.7358247386643,58.7243916823895,
59.7129586261148,60.7015255698401,61.6900925135653,62.6786594572906,63.6672264010159,
64.6557933447411,65.6443602884664,66.6329272321917,67.6214941759169,68.6100611196422,
69.5986280633675,70.5871950070927,71.575761950818,72.5643288945433,73.5528958382685,
74.5414627819938,75.530029725719,76.5185966694443,77.5071636131696,78.4957305568948,
79.4842975006201,80.4728644443454,81.4614313880706,82.4499983317959,83.4385652755212),
 .UNSPECIFIED.);
#601=B_SPLINE_SURFACE_WITH_KNOTS('',3,3,((#40929,#40930,#40931,#40932,#40933,
#40934,#40935,#40936,#40937,#40938,#40939,#40940,#40941,#40942,#40943,#40944,
#40945,#40946,#40947,#40948,#40949,#40950,#40951,#40952,#40953,#40954,#40955,
#40956,#40957,#40958,#40959,#40960,#40961,#40962,#40963,#40964,#40965,#40966,
#40967,#40968,#40969,#40970,#40971,#40972,#40973,#40974,#40975,#40976,#40977,
#40978,#40979,#40980,#40981,#40982,#40983,#40984,#40985,#40986,#40987,#40988,
#40989,#40990,#40991,#40992,#40993,#40994,#40995,#40996,#40997,#40998,#40999,
#41000,#41001,#41002,#41003,#41004,#41005,#41006,#41007,#41008,#41009,#41010,
#41011,#41012,#41013,#41014,#41015,#41016,#41017,#41018,#41019,#41020,#41021,
#41022,#41023,#41024,#41025,#41026,#41027,#41028,#41029,#41030,#41031,#41032,
#41033,#41034,#41035,#41036,#41037,#41038,#41039,#41040,#41041,#41042,#41043,
#41044,#41045,#41046,#41047,#41048,#41049,#41050,#41051,#41052,#41053),
(#41054,#41055,#41056,#41057,#41058,#41059,#41060,#41061,#41062,#41063,
#41064,#41065,#41066,#41067,#41068,#41069,#41070,#41071,#41072,#41073,#41074,
#41075,#41076,#41077,#41078,#41079,#41080,#41081,#41082,#41083,#41084,#41085,
#41086,#41087,#41088,#41089,#41090,#41091,#41092,#41093,#41094,#41095,#41096,
#41097,#41098,#41099,#41100,#41101,#41102,#41103,#41104,#41105,#41106,#41107,
#41108,#41109,#41110,#41111,#41112,#41113,#41114,#41115,#41116,#41117,#41118,
#41119,#41120,#41121,#41122,#41123,#41124,#41125,#41126,#41127,#41128,#41129,
#41130,#41131,#41132,#41133,#41134,#41135,#41136,#41137,#41138,#41139,#41140,
#41141,#41142,#41143,#41144,#41145,#41146,#41147,#41148,#41149,#41150,#41151,
#41152,#41153,#41154,#41155,#41156,#41157,#41158,#41159,#41160,#41161,#41162,
#41163,#41164,#41165,#41166,#41167,#41168,#41169,#41170,#41171,#41172,#41173,
#41174,#41175,#41176,#41177,#41178),(#41179,#41180,#41181,#41182,#41183,
#41184,#41185,#41186,#41187,#41188,#41189,#41190,#41191,#41192,#41193,#41194,
#41195,#41196,#41197,#41198,#41199,#41200,#41201,#41202,#41203,#41204,#41205,
#41206,#41207,#41208,#41209,#41210,#41211,#41212,#41213,#41214,#41215,#41216,
#41217,#41218,#41219,#41220,#41221,#41222,#41223,#41224,#41225,#41226,#41227,
#41228,#41229,#41230,#41231,#41232,#41233,#41234,#41235,#41236,#41237,#41238,
#41239,#41240,#41241,#41242,#41243,#41244,#41245,#41246,#41247,#41248,#41249,
#41250,#41251,#41252,#41253,#41254,#41255,#41256,#41257,#41258,#41259,#41260,
#41261,#41262,#41263,#41264,#41265,#41266,#41267,#41268,#41269,#41270,#41271,
#41272,#41273,#41274,#41275,#41276,#41277,#41278,#41279,#41280,#41281,#41282,
#41283,#41284,#41285,#41286,#41287,#41288,#41289,#41290,#41291,#41292,#41293,
#41294,#41295,#41296,#41297,#41298,#41299,#41300,#41301,#41302,#41303),
(#41304,#41305,#41306,#41307,#41308,#41309,#41310,#41311,#41312,#41313,
#41314,#41315,#41316,#41317,#41318,#41319,#41320,#41321,#41322,#41323,#41324,
#41325,#41326,#41327,#41328,#41329,#41330,#41331,#41332,#41333,#41334,#41335,
#41336,#41337,#41338,#41339,#41340,#41341,#41342,#41343,#41344,#41345,#41346,
#41347,#41348,#41349,#41350,#41351,#41352,#41353,#41354,#41355,#41356,#41357,
#41358,#41359,#41360,#41361,#41362,#41363,#41364,#41365,#41366,#41367,#41368,
#41369,#41370,#41371,#41372,#41373,#41374,#41375,#41376,#41377,#41378,#41379,
#41380,#41381,#41382,#41383,#41384,#41385,#41386,#41387,#41388,#41389,#41390,
#41391,#41392,#41393,#41394,#41395,#41396,#41397,#41398,#41399,#41400,#41401,
#41402,#41403,#41404,#41405,#41406,#41407,#41408,#41409,#41410,#41411,#41412,
#41413,#41414,#41415,#41416,#41417,#41418,#41419,#41420,#41421,#41422,#41423,
#41424,#41425,#41426,#41427,#41428)),.UNSPECIFIED.,.F.,.F.,.F.,(4,4),(4,
1,1,1,1,1,1,1,1,1,1,1,1,1,1,1,1,1,1,1,1,1,1,1,1,1,1,1,1,1,1,1,1,1,1,1,1,
1,1,1,1,1,1,1,1,1,1,1,1,1,1,1,1,1,1,1,1,1,1,1,1,1,1,1,1,1,1,1,1,1,1,1,1,
1,1,1,1,1,1,1,1,1,1,1,1,1,1,1,1,1,1,1,1,1,1,1,1,1,1,1,1,1,1,1,1,1,1,1,1,
1,1,1,1,1,1,1,1,1,1,1,1,1,4),(0.,0.0989001011121828),(8.30505915324874,
8.80271834784681,9.30037754244489,9.79803673704296,10.295695931641,10.7933551262391,
11.2910143208372,11.7886735154353,12.2863327100333,12.7839919046314,13.2816510992295,
13.7793102938275,14.2769694884256,14.7746286830237,15.2722878776218,15.7699470722198,
16.2676062668179,16.765265461416,17.2629246560141,17.7605838506121,18.2582430452102,
18.7559022398083,19.2535614344064,19.7512206290044,20.2488798236025,20.7465390182006,
21.2441982127987,21.7418574073967,22.2395166019948,22.7371757965929,23.2348349911909,
23.732494185789,24.2301533803871,24.7278125749852,25.2254717695832,25.7231309641813,
26.2207901587794,26.7184493533775,27.2161085479755,27.7137677425736,28.2114269371717,
28.7090861317698,29.2067453263678,29.7044045209659,30.202063715564,30.699722910162,
31.1973821047601,31.6950412993582,32.1927004939563,32.6903596885543,33.1880188831524,
33.6856780777505,34.1833372723486,34.6809964669466,35.1786556615447,35.6763148561428,
36.1739740507409,36.6716332453389,37.169292439937,37.6669516345351,38.1646108291331,
38.6622700237312,39.1599292183293,39.6575884129274,40.1552476075254,40.6529068021235,
41.1505659967216,41.6482251913197,42.1458843859177,42.6435435805158,43.1412027751139,
43.638861969712,44.13652116431,44.6341803589081,45.1318395535062,45.6294987481042,
46.1271579427023,46.6248171373004,47.1224763318985,47.6201355264965,48.1177947210946,
48.6154539156927,49.1131131102908,49.6107723048888,50.1084314994869,50.606090694085,
51.103749888683,51.6014090832811,52.0990682778792,52.5967274724773,53.0943866670753,
53.5920458616734,54.0897050562715,54.5873642508696,55.0850234454676,55.5826826400657,
56.0803418346638,56.5780010292619,57.0756602238599,57.573319418458,58.0709786130561,
58.5686378076541,59.0662970022522,59.5639561968503,60.0616153914484,60.5592745860464,
61.0569337806445,61.5545929752426,62.0522521698407,62.5499113644387,63.0475705590368,
63.5452297536349,64.042888948233,64.540548142831,65.0382073374291,65.5358665320272,
66.0335257266252,66.5311849212233,67.0288441158214,67.5265033104195,68.0241625050175,
68.5218216996156,69.0194808942137),.UNSPECIFIED.);
#602=B_SPLINE_SURFACE_WITH_KNOTS('',3,3,((#41703,#41704,#41705,#41706,#41707,
#41708,#41709,#41710,#41711,#41712,#41713,#41714,#41715,#41716,#41717,#41718,
#41719,#41720,#41721,#41722,#41723,#41724,#41725,#41726,#41727,#41728,#41729,
#41730,#41731,#41732,#41733,#41734,#41735,#41736,#41737,#41738,#41739,#41740,
#41741,#41742,#41743,#41744,#41745,#41746,#41747,#41748,#41749,#41750,#41751,
#41752,#41753,#41754,#41755,#41756,#41757,#41758,#41759,#41760,#41761,#41762,
#41763,#41764,#41765,#41766,#41767,#41768,#41769,#41770,#41771,#41772,#41773,
#41774,#41775,#41776,#41777,#41778,#41779,#41780,#41781,#41782,#41783,#41784,
#41785,#41786,#41787,#41788,#41789,#41790,#41791,#41792,#41793,#41794,#41795,
#41796,#41797,#41798,#41799,#41800,#41801,#41802,#41803,#41804,#41805,#41806,
#41807,#41808,#41809,#41810,#41811,#41812,#41813,#41814,#41815,#41816,#41817,
#41818,#41819,#41820,#41821,#41822,#41823,#41824,#41825,#41826,#41827),
(#41828,#41829,#41830,#41831,#41832,#41833,#41834,#41835,#41836,#41837,
#41838,#41839,#41840,#41841,#41842,#41843,#41844,#41845,#41846,#41847,#41848,
#41849,#41850,#41851,#41852,#41853,#41854,#41855,#41856,#41857,#41858,#41859,
#41860,#41861,#41862,#41863,#41864,#41865,#41866,#41867,#41868,#41869,#41870,
#41871,#41872,#41873,#41874,#41875,#41876,#41877,#41878,#41879,#41880,#41881,
#41882,#41883,#41884,#41885,#41886,#41887,#41888,#41889,#41890,#41891,#41892,
#41893,#41894,#41895,#41896,#41897,#41898,#41899,#41900,#41901,#41902,#41903,
#41904,#41905,#41906,#41907,#41908,#41909,#41910,#41911,#41912,#41913,#41914,
#41915,#41916,#41917,#41918,#41919,#41920,#41921,#41922,#41923,#41924,#41925,
#41926,#41927,#41928,#41929,#41930,#41931,#41932,#41933,#41934,#41935,#41936,
#41937,#41938,#41939,#41940,#41941,#41942,#41943,#41944,#41945,#41946,#41947,
#41948,#41949,#41950,#41951,#41952),(#41953,#41954,#41955,#41956,#41957,
#41958,#41959,#41960,#41961,#41962,#41963,#41964,#41965,#41966,#41967,#41968,
#41969,#41970,#41971,#41972,#41973,#41974,#41975,#41976,#41977,#41978,#41979,
#41980,#41981,#41982,#41983,#41984,#41985,#41986,#41987,#41988,#41989,#41990,
#41991,#41992,#41993,#41994,#41995,#41996,#41997,#41998,#41999,#42000,#42001,
#42002,#42003,#42004,#42005,#42006,#42007,#42008,#42009,#42010,#42011,#42012,
#42013,#42014,#42015,#42016,#42017,#42018,#42019,#42020,#42021,#42022,#42023,
#42024,#42025,#42026,#42027,#42028,#42029,#42030,#42031,#42032,#42033,#42034,
#42035,#42036,#42037,#42038,#42039,#42040,#42041,#42042,#42043,#42044,#42045,
#42046,#42047,#42048,#42049,#42050,#42051,#42052,#42053,#42054,#42055,#42056,
#42057,#42058,#42059,#42060,#42061,#42062,#42063,#42064,#42065,#42066,#42067,
#42068,#42069,#42070,#42071,#42072,#42073,#42074,#42075,#42076,#42077),
(#42078,#42079,#42080,#42081,#42082,#42083,#42084,#42085,#42086,#42087,
#42088,#42089,#42090,#42091,#42092,#42093,#42094,#42095,#42096,#42097,#42098,
#42099,#42100,#42101,#42102,#42103,#42104,#42105,#42106,#42107,#42108,#42109,
#42110,#42111,#42112,#42113,#42114,#42115,#42116,#42117,#42118,#42119,#42120,
#42121,#42122,#42123,#42124,#42125,#42126,#42127,#42128,#42129,#42130,#42131,
#42132,#42133,#42134,#42135,#42136,#42137,#42138,#42139,#42140,#42141,#42142,
#42143,#42144,#42145,#42146,#42147,#42148,#42149,#42150,#42151,#42152,#42153,
#42154,#42155,#42156,#42157,#42158,#42159,#42160,#42161,#42162,#42163,#42164,
#42165,#42166,#42167,#42168,#42169,#42170,#42171,#42172,#42173,#42174,#42175,
#42176,#42177,#42178,#42179,#42180,#42181,#42182,#42183,#42184,#42185,#42186,
#42187,#42188,#42189,#42190,#42191,#42192,#42193,#42194,#42195,#42196,#42197,
#42198,#42199,#42200,#42201,#42202)),.UNSPECIFIED.,.F.,.F.,.F.,(4,4),(4,
1,1,1,1,1,1,1,1,1,1,1,1,1,1,1,1,1,1,1,1,1,1,1,1,1,1,1,1,1,1,1,1,1,1,1,1,
1,1,1,1,1,1,1,1,1,1,1,1,1,1,1,1,1,1,1,1,1,1,1,1,1,1,1,1,1,1,1,1,1,1,1,1,
1,1,1,1,1,1,1,1,1,1,1,1,1,1,1,1,1,1,1,1,1,1,1,1,1,1,1,1,1,1,1,1,1,1,1,1,
1,1,1,1,1,1,1,1,1,1,1,1,1,4),(0.,0.0989001011121828),(11.6147305479242,
12.1123897425223,12.6100489371204,13.1077081317185,13.6053673263165,14.1030265209146,
14.6006857155127,15.0983449101107,15.5960041047088,16.0936632993069,16.591322493905,
17.088981688503,17.5866408831011,18.0843000776992,18.5819592722973,19.0796184668953,
19.5772776614934,20.0749368560915,20.5725960506896,21.0702552452876,21.5679144398857,
22.0655736344838,22.5632328290818,23.0608920236799,23.558551218278,24.0562104128761,
24.5538696074741,25.0515288020722,25.5491879966703,26.0468471912684,26.5445063858664,
27.0421655804645,27.5398247750626,28.0374839696607,28.5351431642587,29.0328023588568,
29.5304615534549,30.0281207480529,30.525779942651,31.0234391372491,31.5210983318472,
32.0187575264452,32.5164167210433,33.0140759156414,33.5117351102395,34.0093943048375,
34.5070534994356,35.0047126940337,35.5023718886318,36.0000310832298,36.4976902778279,
36.995349472426,37.4930086670241,37.9906678616221,38.4883270562202,38.9859862508183,
39.4836454454163,39.9813046400144,40.4789638346125,40.9766230292106,41.4742822238086,
41.9719414184067,42.4696006130048,42.9672598076029,43.4649190022009,43.962578196799,
44.4602373913971,44.9578965859952,45.4555557805932,45.9532149751913,46.4508741697894,
46.9485333643874,47.4461925589855,47.9438517535836,48.4415109481817,48.9391701427797,
49.4368293373778,49.9344885319759,50.432147726574,50.929806921172,51.4274661157701,
51.9251253103682,52.4227845049663,52.9204436995643,53.4181028941624,53.9157620887605,
54.4134212833585,54.9110804779566,55.4087396725547,55.9063988671528,56.4040580617508,
56.9017172563489,57.399376450947,57.8970356455451,58.3946948401431,58.8923540347412,
59.3900132293393,59.8876724239374,60.3853316185354,60.8829908131335,61.3806500077316,
61.8783092023296,62.3759683969277,62.8736275915258,63.3712867861239,63.8689459807219,
64.36660517532,64.8642643699181,65.3619235645162,65.8595827591142,66.3572419537123,
66.8549011483104,67.3525603429085,67.8502195375065,68.3478787321046,68.8455379267027,
69.3431971213007,69.8408563158988,70.3385155104969,70.836174705095,71.333833899693,
71.8314930942911,72.3291522888892),.UNSPECIFIED.);
#603=FACE_OUTER_BOUND('',#1147,.T.);
#604=FACE_OUTER_BOUND('',#1148,.T.);
#605=FACE_OUTER_BOUND('',#1149,.T.);
#606=FACE_OUTER_BOUND('',#1150,.T.);
#607=FACE_OUTER_BOUND('',#1151,.T.);
#608=FACE_OUTER_BOUND('',#1152,.T.);
#609=FACE_OUTER_BOUND('',#1153,.T.);
#610=FACE_OUTER_BOUND('',#1154,.T.);
#611=FACE_OUTER_BOUND('',#1155,.T.);
#612=FACE_OUTER_BOUND('',#1156,.T.);
#613=FACE_OUTER_BOUND('',#1157,.T.);
#614=FACE_OUTER_BOUND('',#1158,.T.);
#615=FACE_OUTER_BOUND('',#1159,.T.);
#616=FACE_OUTER_BOUND('',#1160,.T.);
#617=FACE_OUTER_BOUND('',#1161,.T.);
#618=FACE_OUTER_BOUND('',#1162,.T.);
#619=FACE_OUTER_BOUND('',#1163,.T.);
#620=FACE_OUTER_BOUND('',#1164,.T.);
#621=FACE_OUTER_BOUND('',#1165,.T.);
#622=FACE_OUTER_BOUND('',#1166,.T.);
#623=FACE_OUTER_BOUND('',#1167,.T.);
#624=FACE_OUTER_BOUND('',#1168,.T.);
#625=FACE_OUTER_BOUND('',#1169,.T.);
#626=FACE_OUTER_BOUND('',#1170,.T.);
#627=FACE_OUTER_BOUND('',#1171,.T.);
#628=FACE_OUTER_BOUND('',#1172,.T.);
#629=FACE_OUTER_BOUND('',#1173,.T.);
#630=FACE_OUTER_BOUND('',#1174,.T.);
#631=FACE_OUTER_BOUND('',#1175,.T.);
#632=FACE_OUTER_BOUND('',#1176,.T.);
#633=FACE_OUTER_BOUND('',#1177,.T.);
#634=FACE_OUTER_BOUND('',#1178,.T.);
#635=FACE_OUTER_BOUND('',#1179,.T.);
#636=FACE_OUTER_BOUND('',#1180,.T.);
#637=FACE_OUTER_BOUND('',#1181,.T.);
#638=FACE_OUTER_BOUND('',#1182,.T.);
#639=FACE_OUTER_BOUND('',#1183,.T.);
#640=FACE_OUTER_BOUND('',#1184,.T.);
#641=FACE_OUTER_BOUND('',#1185,.T.);
#642=FACE_OUTER_BOUND('',#1186,.T.);
#643=FACE_OUTER_BOUND('',#1187,.T.);
#644=FACE_OUTER_BOUND('',#1188,.T.);
#645=FACE_OUTER_BOUND('',#1189,.T.);
#646=FACE_OUTER_BOUND('',#1190,.T.);
#647=FACE_OUTER_BOUND('',#1191,.T.);
#648=FACE_OUTER_BOUND('',#1192,.T.);
#649=FACE_OUTER_BOUND('',#1193,.T.);
#650=FACE_OUTER_BOUND('',#1194,.T.);
#651=FACE_OUTER_BOUND('',#1195,.T.);
#652=FACE_OUTER_BOUND('',#1196,.T.);
#653=FACE_OUTER_BOUND('',#1197,.T.);
#654=FACE_OUTER_BOUND('',#1198,.T.);
#655=FACE_OUTER_BOUND('',#1199,.T.);
#656=FACE_OUTER_BOUND('',#1200,.T.);
#657=FACE_OUTER_BOUND('',#1201,.T.);
#658=FACE_OUTER_BOUND('',#1202,.T.);
#659=FACE_OUTER_BOUND('',#1203,.T.);
#660=FACE_OUTER_BOUND('',#1204,.T.);
#661=FACE_OUTER_BOUND('',#1205,.T.);
#662=FACE_OUTER_BOUND('',#1206,.T.);
#663=FACE_OUTER_BOUND('',#1207,.T.);
#664=FACE_OUTER_BOUND('',#1208,.T.);
#665=FACE_OUTER_BOUND('',#1209,.T.);
#666=FACE_OUTER_BOUND('',#1210,.T.);
#667=FACE_OUTER_BOUND('',#1211,.T.);
#668=FACE_OUTER_BOUND('',#1212,.T.);
#669=FACE_OUTER_BOUND('',#1213,.T.);
#670=FACE_OUTER_BOUND('',#1214,.T.);
#671=FACE_OUTER_BOUND('',#1215,.T.);
#672=FACE_OUTER_BOUND('',#1216,.T.);
#673=FACE_OUTER_BOUND('',#1217,.T.);
#674=FACE_OUTER_BOUND('',#1218,.T.);
#675=FACE_OUTER_BOUND('',#1219,.T.);
#676=FACE_OUTER_BOUND('',#1220,.T.);
#677=FACE_OUTER_BOUND('',#1221,.T.);
#678=FACE_OUTER_BOUND('',#1222,.T.);
#679=FACE_OUTER_BOUND('',#1223,.T.);
#680=FACE_OUTER_BOUND('',#1224,.T.);
#681=FACE_OUTER_BOUND('',#1225,.T.);
#682=FACE_OUTER_BOUND('',#1226,.T.);
#683=FACE_OUTER_BOUND('',#1227,.T.);
#684=FACE_OUTER_BOUND('',#1228,.T.);
#685=FACE_OUTER_BOUND('',#1229,.T.);
#686=FACE_OUTER_BOUND('',#1230,.T.);
#687=FACE_OUTER_BOUND('',#1231,.T.);
#688=FACE_OUTER_BOUND('',#1232,.T.);
#689=FACE_OUTER_BOUND('',#1233,.T.);
#690=FACE_OUTER_BOUND('',#1234,.T.);
#691=FACE_OUTER_BOUND('',#1235,.T.);
#692=FACE_OUTER_BOUND('',#1236,.T.);
#693=FACE_OUTER_BOUND('',#1237,.T.);
#694=FACE_OUTER_BOUND('',#1238,.T.);
#695=FACE_OUTER_BOUND('',#1239,.T.);
#696=FACE_OUTER_BOUND('',#1240,.T.);
#697=FACE_OUTER_BOUND('',#1241,.T.);
#698=FACE_OUTER_BOUND('',#1242,.T.);
#699=FACE_OUTER_BOUND('',#1243,.T.);
#700=FACE_OUTER_BOUND('',#1244,.T.);
#701=FACE_OUTER_BOUND('',#1245,.T.);
#702=FACE_OUTER_BOUND('',#1246,.T.);
#703=FACE_OUTER_BOUND('',#1247,.T.);
#704=FACE_OUTER_BOUND('',#1248,.T.);
#705=FACE_OUTER_BOUND('',#1249,.T.);
#706=FACE_OUTER_BOUND('',#1250,.T.);
#707=FACE_OUTER_BOUND('',#1251,.T.);
#708=FACE_OUTER_BOUND('',#1252,.T.);
#709=FACE_OUTER_BOUND('',#1253,.T.);
#710=FACE_OUTER_BOUND('',#1254,.T.);
#711=FACE_OUTER_BOUND('',#1255,.T.);
#712=FACE_OUTER_BOUND('',#1256,.T.);
#713=FACE_OUTER_BOUND('',#1257,.T.);
#714=FACE_OUTER_BOUND('',#1258,.T.);
#715=FACE_OUTER_BOUND('',#1259,.T.);
#716=FACE_OUTER_BOUND('',#1260,.T.);
#717=FACE_OUTER_BOUND('',#1261,.T.);
#718=FACE_OUTER_BOUND('',#1262,.T.);
#719=FACE_OUTER_BOUND('',#1263,.T.);
#720=FACE_OUTER_BOUND('',#1264,.T.);
#721=FACE_OUTER_BOUND('',#1265,.T.);
#722=FACE_OUTER_BOUND('',#1266,.T.);
#723=FACE_OUTER_BOUND('',#1267,.T.);
#724=FACE_OUTER_BOUND('',#1268,.T.);
#725=FACE_OUTER_BOUND('',#1269,.T.);
#726=FACE_OUTER_BOUND('',#1270,.T.);
#727=FACE_OUTER_BOUND('',#1271,.T.);
#728=FACE_OUTER_BOUND('',#1272,.T.);
#729=FACE_OUTER_BOUND('',#1273,.T.);
#730=FACE_OUTER_BOUND('',#1274,.T.);
#731=FACE_OUTER_BOUND('',#1275,.T.);
#732=FACE_OUTER_BOUND('',#1276,.T.);
#733=FACE_OUTER_BOUND('',#1277,.T.);
#734=FACE_OUTER_BOUND('',#1278,.T.);
#735=FACE_OUTER_BOUND('',#1279,.T.);
#736=FACE_OUTER_BOUND('',#1280,.T.);
#737=FACE_OUTER_BOUND('',#1281,.T.);
#738=FACE_OUTER_BOUND('',#1282,.T.);
#739=FACE_OUTER_BOUND('',#1283,.T.);
#740=FACE_OUTER_BOUND('',#1284,.T.);
#741=FACE_OUTER_BOUND('',#1285,.T.);
#742=FACE_OUTER_BOUND('',#1286,.T.);
#743=FACE_OUTER_BOUND('',#1287,.T.);
#744=FACE_OUTER_BOUND('',#1288,.T.);
#745=FACE_OUTER_BOUND('',#1289,.T.);
#746=FACE_OUTER_BOUND('',#1290,.T.);
#747=FACE_OUTER_BOUND('',#1291,.T.);
#748=FACE_OUTER_BOUND('',#1292,.T.);
#749=FACE_OUTER_BOUND('',#1293,.T.);
#750=FACE_OUTER_BOUND('',#1294,.T.);
#751=FACE_OUTER_BOUND('',#1295,.T.);
#752=FACE_OUTER_BOUND('',#1296,.T.);
#753=FACE_OUTER_BOUND('',#1297,.T.);
#754=FACE_OUTER_BOUND('',#1298,.T.);
#755=FACE_OUTER_BOUND('',#1299,.T.);
#756=FACE_OUTER_BOUND('',#1300,.T.);
#757=FACE_OUTER_BOUND('',#1301,.T.);
#758=FACE_OUTER_BOUND('',#1302,.T.);
#759=FACE_OUTER_BOUND('',#1303,.T.);
#760=FACE_OUTER_BOUND('',#1304,.T.);
#761=FACE_OUTER_BOUND('',#1305,.T.);
#762=FACE_OUTER_BOUND('',#1306,.T.);
#763=FACE_OUTER_BOUND('',#1307,.T.);
#764=FACE_OUTER_BOUND('',#1308,.T.);
#765=FACE_OUTER_BOUND('',#1309,.T.);
#766=FACE_OUTER_BOUND('',#1310,.T.);
#767=FACE_OUTER_BOUND('',#1311,.T.);
#768=FACE_OUTER_BOUND('',#1312,.T.);
#769=FACE_OUTER_BOUND('',#1313,.T.);
#770=FACE_OUTER_BOUND('',#1314,.T.);
#771=FACE_OUTER_BOUND('',#1315,.T.);
#772=FACE_OUTER_BOUND('',#1316,.T.);
#773=FACE_OUTER_BOUND('',#1317,.T.);
#774=FACE_OUTER_BOUND('',#1318,.T.);
#775=FACE_OUTER_BOUND('',#1319,.T.);
#776=FACE_OUTER_BOUND('',#1320,.T.);
#777=FACE_OUTER_BOUND('',#1321,.T.);
#778=FACE_OUTER_BOUND('',#1322,.T.);
#779=FACE_OUTER_BOUND('',#1323,.T.);
#780=FACE_OUTER_BOUND('',#1324,.T.);
#781=FACE_OUTER_BOUND('',#1325,.T.);
#782=FACE_OUTER_BOUND('',#1326,.T.);
#783=FACE_OUTER_BOUND('',#1327,.T.);
#784=FACE_OUTER_BOUND('',#1328,.T.);
#785=FACE_OUTER_BOUND('',#1329,.T.);
#786=FACE_OUTER_BOUND('',#1330,.T.);
#787=FACE_OUTER_BOUND('',#1331,.T.);
#788=FACE_OUTER_BOUND('',#1332,.T.);
#789=FACE_OUTER_BOUND('',#1333,.T.);
#790=FACE_OUTER_BOUND('',#1334,.T.);
#791=FACE_OUTER_BOUND('',#1335,.T.);
#792=FACE_OUTER_BOUND('',#1336,.T.);
#793=FACE_OUTER_BOUND('',#1337,.T.);
#794=FACE_OUTER_BOUND('',#1338,.T.);
#795=FACE_OUTER_BOUND('',#1339,.T.);
#796=FACE_OUTER_BOUND('',#1340,.T.);
#797=FACE_OUTER_BOUND('',#1341,.T.);
#798=FACE_OUTER_BOUND('',#1342,.T.);
#799=FACE_OUTER_BOUND('',#1343,.T.);
#800=FACE_OUTER_BOUND('',#1344,.T.);
#801=FACE_OUTER_BOUND('',#1345,.T.);
#802=FACE_OUTER_BOUND('',#1346,.T.);
#803=FACE_OUTER_BOUND('',#1347,.T.);
#804=FACE_OUTER_BOUND('',#1348,.T.);
#805=FACE_OUTER_BOUND('',#1349,.T.);
#806=FACE_OUTER_BOUND('',#1350,.T.);
#807=FACE_OUTER_BOUND('',#1351,.T.);
#808=FACE_OUTER_BOUND('',#1352,.T.);
#809=FACE_OUTER_BOUND('',#1353,.T.);
#810=FACE_OUTER_BOUND('',#1354,.T.);
#811=FACE_OUTER_BOUND('',#1355,.T.);
#812=FACE_OUTER_BOUND('',#1356,.T.);
#813=FACE_OUTER_BOUND('',#1357,.T.);
#814=FACE_OUTER_BOUND('',#1358,.T.);
#815=FACE_OUTER_BOUND('',#1359,.T.);
#816=FACE_OUTER_BOUND('',#1360,.T.);
#817=FACE_OUTER_BOUND('',#1361,.T.);
#818=FACE_OUTER_BOUND('',#1362,.T.);
#819=FACE_OUTER_BOUND('',#1363,.T.);
#820=FACE_OUTER_BOUND('',#1364,.T.);
#821=FACE_OUTER_BOUND('',#1365,.T.);
#822=FACE_OUTER_BOUND('',#1366,.T.);
#823=FACE_OUTER_BOUND('',#1367,.T.);
#824=FACE_OUTER_BOUND('',#1368,.T.);
#825=FACE_OUTER_BOUND('',#1369,.T.);
#826=FACE_OUTER_BOUND('',#1370,.T.);
#827=FACE_OUTER_BOUND('',#1371,.T.);
#828=FACE_OUTER_BOUND('',#1372,.T.);
#829=FACE_OUTER_BOUND('',#1373,.T.);
#830=FACE_OUTER_BOUND('',#1374,.T.);
#831=FACE_OUTER_BOUND('',#1375,.T.);
#832=FACE_OUTER_BOUND('',#1376,.T.);
#833=FACE_OUTER_BOUND('',#1377,.T.);
#834=FACE_OUTER_BOUND('',#1378,.T.);
#835=FACE_OUTER_BOUND('',#1379,.T.);
#836=FACE_OUTER_BOUND('',#1380,.T.);
#837=FACE_OUTER_BOUND('',#1381,.T.);
#838=FACE_OUTER_BOUND('',#1382,.T.);
#839=FACE_OUTER_BOUND('',#1383,.T.);
#840=FACE_OUTER_BOUND('',#1384,.T.);
#841=FACE_OUTER_BOUND('',#1385,.T.);
#842=FACE_OUTER_BOUND('',#1386,.T.);
#843=FACE_OUTER_BOUND('',#1387,.T.);
#844=FACE_OUTER_BOUND('',#1388,.T.);
#845=FACE_OUTER_BOUND('',#1389,.T.);
#846=FACE_OUTER_BOUND('',#1390,.T.);
#847=FACE_OUTER_BOUND('',#1391,.T.);
#848=FACE_OUTER_BOUND('',#1392,.T.);
#849=FACE_OUTER_BOUND('',#1393,.T.);
#850=FACE_OUTER_BOUND('',#1394,.T.);
#851=FACE_OUTER_BOUND('',#1395,.T.);
#852=FACE_OUTER_BOUND('',#1396,.T.);
#853=FACE_OUTER_BOUND('',#1397,.T.);
#854=FACE_OUTER_BOUND('',#1398,.T.);
#855=FACE_OUTER_BOUND('',#1399,.T.);
#856=FACE_OUTER_BOUND('',#1400,.T.);
#857=FACE_OUTER_BOUND('',#1401,.T.);
#858=FACE_OUTER_BOUND('',#1402,.T.);
#859=FACE_OUTER_BOUND('',#1403,.T.);
#860=FACE_OUTER_BOUND('',#1404,.T.);
#861=FACE_OUTER_BOUND('',#1405,.T.);
#862=FACE_OUTER_BOUND('',#1406,.T.);
#863=FACE_OUTER_BOUND('',#1407,.T.);
#864=FACE_OUTER_BOUND('',#1408,.T.);
#865=FACE_OUTER_BOUND('',#1409,.T.);
#866=FACE_OUTER_BOUND('',#1410,.T.);
#867=FACE_OUTER_BOUND('',#1412,.T.);
#868=FACE_OUTER_BOUND('',#1413,.T.);
#869=FACE_OUTER_BOUND('',#1414,.T.);
#870=FACE_OUTER_BOUND('',#1420,.T.);
#871=FACE_OUTER_BOUND('',#1421,.T.);
#872=FACE_OUTER_BOUND('',#1422,.T.);
#873=FACE_OUTER_BOUND('',#1423,.T.);
#874=FACE_OUTER_BOUND('',#1424,.T.);
#875=FACE_OUTER_BOUND('',#1425,.T.);
#876=FACE_OUTER_BOUND('',#1426,.T.);
#877=FACE_OUTER_BOUND('',#1427,.T.);
#878=FACE_OUTER_BOUND('',#1428,.T.);
#879=FACE_OUTER_BOUND('',#1429,.T.);
#880=FACE_OUTER_BOUND('',#1430,.T.);
#881=FACE_OUTER_BOUND('',#1431,.T.);
#882=FACE_OUTER_BOUND('',#1432,.T.);
#883=FACE_OUTER_BOUND('',#1433,.T.);
#884=FACE_OUTER_BOUND('',#1434,.T.);
#885=FACE_OUTER_BOUND('',#1435,.T.);
#886=FACE_OUTER_BOUND('',#1436,.T.);
#887=FACE_OUTER_BOUND('',#1437,.T.);
#888=FACE_OUTER_BOUND('',#1438,.T.);
#889=FACE_OUTER_BOUND('',#1439,.T.);
#890=FACE_OUTER_BOUND('',#1440,.T.);
#891=FACE_OUTER_BOUND('',#1441,.T.);
#892=FACE_OUTER_BOUND('',#1442,.T.);
#893=FACE_OUTER_BOUND('',#1443,.T.);
#894=FACE_OUTER_BOUND('',#1444,.T.);
#895=FACE_OUTER_BOUND('',#1445,.T.);
#896=FACE_OUTER_BOUND('',#1446,.T.);
#897=FACE_OUTER_BOUND('',#1447,.T.);
#898=FACE_OUTER_BOUND('',#1448,.T.);
#899=FACE_OUTER_BOUND('',#1449,.T.);
#900=FACE_OUTER_BOUND('',#1450,.T.);
#901=FACE_OUTER_BOUND('',#1451,.T.);
#902=FACE_OUTER_BOUND('',#1452,.T.);
#903=FACE_OUTER_BOUND('',#1453,.T.);
#904=FACE_OUTER_BOUND('',#1454,.T.);
#905=FACE_OUTER_BOUND('',#1455,.T.);
#906=FACE_OUTER_BOUND('',#1456,.T.);
#907=FACE_OUTER_BOUND('',#1457,.T.);
#908=FACE_OUTER_BOUND('',#1458,.T.);
#909=FACE_OUTER_BOUND('',#1459,.T.);
#910=FACE_OUTER_BOUND('',#1460,.T.);
#911=FACE_OUTER_BOUND('',#1461,.T.);
#912=FACE_OUTER_BOUND('',#1462,.T.);
#913=FACE_OUTER_BOUND('',#1463,.T.);
#914=FACE_OUTER_BOUND('',#1464,.T.);
#915=FACE_OUTER_BOUND('',#1465,.T.);
#916=FACE_OUTER_BOUND('',#1466,.T.);
#917=FACE_OUTER_BOUND('',#1467,.T.);
#918=FACE_OUTER_BOUND('',#1468,.T.);
#919=FACE_OUTER_BOUND('',#1469,.T.);
#920=FACE_OUTER_BOUND('',#1470,.T.);
#921=FACE_OUTER_BOUND('',#1471,.T.);
#922=FACE_OUTER_BOUND('',#1472,.T.);
#923=FACE_OUTER_BOUND('',#1473,.T.);
#924=FACE_OUTER_BOUND('',#1474,.T.);
#925=FACE_OUTER_BOUND('',#1475,.T.);
#926=FACE_OUTER_BOUND('',#1476,.T.);
#927=FACE_OUTER_BOUND('',#1477,.T.);
#928=FACE_OUTER_BOUND('',#1478,.T.);
#929=FACE_OUTER_BOUND('',#1479,.T.);
#930=FACE_OUTER_BOUND('',#1480,.T.);
#931=FACE_OUTER_BOUND('',#1481,.T.);
#932=FACE_OUTER_BOUND('',#1482,.T.);
#933=FACE_OUTER_BOUND('',#1483,.T.);
#934=FACE_OUTER_BOUND('',#1484,.T.);
#935=FACE_OUTER_BOUND('',#1485,.T.);
#936=FACE_OUTER_BOUND('',#1486,.T.);
#937=FACE_OUTER_BOUND('',#1487,.T.);
#938=FACE_OUTER_BOUND('',#1488,.T.);
#939=FACE_OUTER_BOUND('',#1489,.T.);
#940=FACE_OUTER_BOUND('',#1490,.T.);
#941=FACE_OUTER_BOUND('',#1491,.T.);
#942=FACE_OUTER_BOUND('',#1510,.T.);
#943=FACE_OUTER_BOUND('',#1511,.T.);
#944=FACE_OUTER_BOUND('',#1512,.T.);
#945=FACE_OUTER_BOUND('',#1514,.T.);
#946=FACE_OUTER_BOUND('',#1515,.T.);
#947=FACE_OUTER_BOUND('',#1534,.T.);
#948=FACE_OUTER_BOUND('',#1535,.T.);
#949=FACE_OUTER_BOUND('',#1536,.T.);
#950=FACE_OUTER_BOUND('',#1542,.T.);
#951=FACE_OUTER_BOUND('',#1543,.T.);
#952=FACE_OUTER_BOUND('',#1544,.T.);
#953=FACE_OUTER_BOUND('',#1545,.T.);
#954=FACE_OUTER_BOUND('',#1546,.T.);
#955=FACE_OUTER_BOUND('',#1547,.T.);
#956=FACE_OUTER_BOUND('',#1548,.T.);
#957=FACE_OUTER_BOUND('',#1549,.T.);
#958=FACE_OUTER_BOUND('',#1550,.T.);
#959=FACE_OUTER_BOUND('',#1555,.T.);
#960=FACE_OUTER_BOUND('',#1560,.T.);
#961=FACE_OUTER_BOUND('',#1561,.T.);
#962=FACE_OUTER_BOUND('',#1562,.T.);
#963=FACE_OUTER_BOUND('',#1563,.T.);
#964=FACE_OUTER_BOUND('',#1564,.T.);
#965=FACE_OUTER_BOUND('',#1565,.T.);
#966=FACE_OUTER_BOUND('',#1566,.T.);
#967=FACE_OUTER_BOUND('',#1567,.T.);
#968=FACE_OUTER_BOUND('',#1568,.T.);
#969=FACE_OUTER_BOUND('',#1569,.T.);
#970=FACE_OUTER_BOUND('',#1570,.T.);
#971=FACE_OUTER_BOUND('',#1571,.T.);
#972=FACE_OUTER_BOUND('',#1572,.T.);
#973=FACE_OUTER_BOUND('',#1578,.T.);
#974=FACE_OUTER_BOUND('',#1584,.T.);
#975=FACE_OUTER_BOUND('',#1585,.T.);
#976=FACE_OUTER_BOUND('',#1586,.T.);
#977=FACE_OUTER_BOUND('',#1588,.T.);
#978=FACE_OUTER_BOUND('',#1590,.T.);
#979=FACE_OUTER_BOUND('',#1591,.T.);
#980=FACE_OUTER_BOUND('',#1592,.T.);
#981=FACE_OUTER_BOUND('',#1593,.T.);
#982=FACE_OUTER_BOUND('',#1594,.T.);
#983=FACE_OUTER_BOUND('',#1595,.T.);
#984=FACE_OUTER_BOUND('',#1596,.T.);
#985=FACE_OUTER_BOUND('',#1597,.T.);
#986=FACE_OUTER_BOUND('',#1598,.T.);
#987=FACE_OUTER_BOUND('',#1599,.T.);
#988=FACE_OUTER_BOUND('',#1600,.T.);
#989=FACE_OUTER_BOUND('',#1601,.T.);
#990=FACE_OUTER_BOUND('',#1602,.T.);
#991=FACE_OUTER_BOUND('',#1603,.T.);
#992=FACE_OUTER_BOUND('',#1604,.T.);
#993=FACE_OUTER_BOUND('',#1605,.T.);
#994=FACE_OUTER_BOUND('',#1606,.T.);
#995=FACE_OUTER_BOUND('',#1607,.T.);
#996=FACE_OUTER_BOUND('',#1608,.T.);
#997=FACE_OUTER_BOUND('',#1609,.T.);
#998=FACE_OUTER_BOUND('',#1610,.T.);
#999=FACE_OUTER_BOUND('',#1611,.T.);
#1000=FACE_OUTER_BOUND('',#1612,.T.);
#1001=FACE_OUTER_BOUND('',#1631,.T.);
#1002=FACE_OUTER_BOUND('',#1650,.T.);
#1003=FACE_OUTER_BOUND('',#1651,.T.);
#1004=FACE_OUTER_BOUND('',#1652,.T.);
#1005=FACE_OUTER_BOUND('',#1653,.T.);
#1006=FACE_OUTER_BOUND('',#1654,.T.);
#1007=FACE_OUTER_BOUND('',#1655,.T.);
#1008=FACE_OUTER_BOUND('',#1656,.T.);
#1009=FACE_OUTER_BOUND('',#1657,.T.);
#1010=FACE_OUTER_BOUND('',#1658,.T.);
#1011=FACE_OUTER_BOUND('',#1659,.T.);
#1012=FACE_OUTER_BOUND('',#1660,.T.);
#1013=FACE_OUTER_BOUND('',#1661,.T.);
#1014=FACE_OUTER_BOUND('',#1669,.T.);
#1015=FACE_OUTER_BOUND('',#1677,.T.);
#1016=FACE_OUTER_BOUND('',#1678,.T.);
#1017=FACE_OUTER_BOUND('',#1679,.T.);
#1018=FACE_OUTER_BOUND('',#1680,.T.);
#1019=FACE_OUTER_BOUND('',#1681,.T.);
#1020=FACE_OUTER_BOUND('',#1682,.T.);
#1021=FACE_OUTER_BOUND('',#1683,.T.);
#1022=FACE_OUTER_BOUND('',#1684,.T.);
#1023=FACE_OUTER_BOUND('',#1685,.T.);
#1024=FACE_OUTER_BOUND('',#1686,.T.);
#1025=FACE_OUTER_BOUND('',#1687,.T.);
#1026=FACE_OUTER_BOUND('',#1688,.T.);
#1027=FACE_OUTER_BOUND('',#1689,.T.);
#1028=FACE_OUTER_BOUND('',#1690,.T.);
#1029=FACE_OUTER_BOUND('',#1691,.T.);
#1030=FACE_OUTER_BOUND('',#1692,.T.);
#1031=FACE_OUTER_BOUND('',#1693,.T.);
#1032=FACE_OUTER_BOUND('',#1694,.T.);
#1033=FACE_OUTER_BOUND('',#1695,.T.);
#1034=FACE_OUTER_BOUND('',#1696,.T.);
#1035=FACE_OUTER_BOUND('',#1697,.T.);
#1036=FACE_OUTER_BOUND('',#1698,.T.);
#1037=FACE_OUTER_BOUND('',#1699,.T.);
#1038=FACE_OUTER_BOUND('',#1700,.T.);
#1039=FACE_OUTER_BOUND('',#1701,.T.);
#1040=FACE_OUTER_BOUND('',#1702,.T.);
#1041=FACE_OUTER_BOUND('',#1703,.T.);
#1042=FACE_OUTER_BOUND('',#1704,.T.);
#1043=FACE_OUTER_BOUND('',#1705,.T.);
#1044=FACE_OUTER_BOUND('',#1706,.T.);
#1045=FACE_OUTER_BOUND('',#1707,.T.);
#1046=FACE_OUTER_BOUND('',#1708,.T.);
#1047=FACE_OUTER_BOUND('',#1709,.T.);
#1048=FACE_OUTER_BOUND('',#1710,.T.);
#1049=FACE_OUTER_BOUND('',#1711,.T.);
#1050=FACE_OUTER_BOUND('',#1712,.T.);
#1051=FACE_OUTER_BOUND('',#1713,.T.);
#1052=FACE_OUTER_BOUND('',#1714,.T.);
#1053=FACE_OUTER_BOUND('',#1715,.T.);
#1054=FACE_OUTER_BOUND('',#1716,.T.);
#1055=FACE_OUTER_BOUND('',#1717,.T.);
#1056=FACE_OUTER_BOUND('',#1718,.T.);
#1057=FACE_OUTER_BOUND('',#1719,.T.);
#1058=FACE_OUTER_BOUND('',#1720,.T.);
#1059=FACE_OUTER_BOUND('',#1721,.T.);
#1060=FACE_OUTER_BOUND('',#1723,.T.);
#1061=FACE_OUTER_BOUND('',#1724,.T.);
#1062=FACE_OUTER_BOUND('',#1726,.T.);
#1063=FACE_OUTER_BOUND('',#1727,.T.);
#1064=FACE_OUTER_BOUND('',#1728,.T.);
#1065=FACE_OUTER_BOUND('',#1729,.T.);
#1066=FACE_OUTER_BOUND('',#1730,.T.);
#1067=FACE_OUTER_BOUND('',#1731,.T.);
#1068=FACE_OUTER_BOUND('',#1732,.T.);
#1069=FACE_OUTER_BOUND('',#1733,.T.);
#1070=FACE_OUTER_BOUND('',#1734,.T.);
#1071=FACE_OUTER_BOUND('',#1735,.T.);
#1072=FACE_OUTER_BOUND('',#1736,.T.);
#1073=FACE_OUTER_BOUND('',#1737,.T.);
#1074=FACE_OUTER_BOUND('',#1738,.T.);
#1075=FACE_OUTER_BOUND('',#1739,.T.);
#1076=FACE_OUTER_BOUND('',#1740,.T.);
#1077=FACE_OUTER_BOUND('',#1741,.T.);
#1078=FACE_OUTER_BOUND('',#1742,.T.);
#1079=FACE_OUTER_BOUND('',#1743,.T.);
#1080=FACE_OUTER_BOUND('',#1744,.T.);
#1081=FACE_OUTER_BOUND('',#1745,.T.);
#1082=FACE_OUTER_BOUND('',#1746,.T.);
#1083=FACE_OUTER_BOUND('',#1747,.T.);
#1084=FACE_OUTER_BOUND('',#1748,.T.);
#1085=FACE_OUTER_BOUND('',#1749,.T.);
#1086=FACE_OUTER_BOUND('',#1750,.T.);
#1087=FACE_OUTER_BOUND('',#1751,.T.);
#1088=FACE_OUTER_BOUND('',#1752,.T.);
#1089=FACE_OUTER_BOUND('',#1753,.T.);
#1090=FACE_OUTER_BOUND('',#1754,.T.);
#1091=FACE_OUTER_BOUND('',#1755,.T.);
#1092=FACE_OUTER_BOUND('',#1756,.T.);
#1093=FACE_OUTER_BOUND('',#1757,.T.);
#1094=FACE_OUTER_BOUND('',#1758,.T.);
#1095=FACE_OUTER_BOUND('',#1759,.T.);
#1096=FACE_OUTER_BOUND('',#1760,.T.);
#1097=FACE_OUTER_BOUND('',#1761,.T.);
#1098=FACE_OUTER_BOUND('',#1763,.T.);
#1099=FACE_OUTER_BOUND('',#1764,.T.);
#1100=FACE_OUTER_BOUND('',#1766,.T.);
#1101=FACE_OUTER_BOUND('',#1767,.T.);
#1102=FACE_OUTER_BOUND('',#1768,.T.);
#1103=FACE_OUTER_BOUND('',#1769,.T.);
#1104=FACE_OUTER_BOUND('',#1770,.T.);
#1105=FACE_OUTER_BOUND('',#1771,.T.);
#1106=FACE_OUTER_BOUND('',#1772,.T.);
#1107=FACE_OUTER_BOUND('',#1773,.T.);
#1108=FACE_OUTER_BOUND('',#1774,.T.);
#1109=FACE_OUTER_BOUND('',#1775,.T.);
#1110=FACE_OUTER_BOUND('',#1776,.T.);
#1111=FACE_OUTER_BOUND('',#1777,.T.);
#1112=FACE_OUTER_BOUND('',#1778,.T.);
#1113=FACE_OUTER_BOUND('',#1779,.T.);
#1114=FACE_OUTER_BOUND('',#1780,.T.);
#1115=FACE_OUTER_BOUND('',#1781,.T.);
#1116=FACE_OUTER_BOUND('',#1782,.T.);
#1117=FACE_OUTER_BOUND('',#1783,.T.);
#1118=FACE_OUTER_BOUND('',#1784,.T.);
#1119=FACE_OUTER_BOUND('',#1785,.T.);
#1120=FACE_OUTER_BOUND('',#1786,.T.);
#1121=FACE_OUTER_BOUND('',#1787,.T.);
#1122=FACE_OUTER_BOUND('',#1788,.T.);
#1123=FACE_OUTER_BOUND('',#1789,.T.);
#1124=FACE_OUTER_BOUND('',#1790,.T.);
#1125=FACE_OUTER_BOUND('',#1792,.T.);
#1126=FACE_OUTER_BOUND('',#1794,.T.);
#1127=FACE_OUTER_BOUND('',#1795,.T.);
#1128=FACE_OUTER_BOUND('',#1796,.T.);
#1129=FACE_OUTER_BOUND('',#1798,.T.);
#1130=FACE_OUTER_BOUND('',#1800,.T.);
#1131=FACE_OUTER_BOUND('',#1801,.T.);
#1132=FACE_OUTER_BOUND('',#1802,.T.);
#1133=FACE_OUTER_BOUND('',#1804,.T.);
#1134=FACE_OUTER_BOUND('',#1806,.T.);
#1135=FACE_OUTER_BOUND('',#1807,.T.);
#1136=FACE_OUTER_BOUND('',#1808,.T.);
#1137=FACE_OUTER_BOUND('',#1809,.T.);
#1138=FACE_OUTER_BOUND('',#1811,.T.);
#1139=FACE_OUTER_BOUND('',#1813,.T.);
#1140=FACE_OUTER_BOUND('',#1814,.T.);
#1141=FACE_OUTER_BOUND('',#1816,.T.);
#1142=FACE_OUTER_BOUND('',#1817,.T.);
#1143=FACE_OUTER_BOUND('',#1819,.T.);
#1144=FACE_OUTER_BOUND('',#1820,.T.);
#1145=FACE_OUTER_BOUND('',#1821,.T.);
#1146=FACE_OUTER_BOUND('',#1823,.T.);
#1147=EDGE_LOOP('',(#6389,#6390,#6391,#6392,#6393,#6394,#6395,#6396));
#1148=EDGE_LOOP('',(#6397,#6398,#6399,#6400));
#1149=EDGE_LOOP('',(#6401,#6402,#6403,#6404));
#1150=EDGE_LOOP('',(#6405,#6406,#6407,#6408));
#1151=EDGE_LOOP('',(#6409,#6410,#6411,#6412));
#1152=EDGE_LOOP('',(#6413,#6414,#6415,#6416));
#1153=EDGE_LOOP('',(#6417,#6418,#6419,#6420));
#1154=EDGE_LOOP('',(#6421,#6422,#6423,#6424));
#1155=EDGE_LOOP('',(#6425,#6426,#6427,#6428));
#1156=EDGE_LOOP('',(#6429,#6430,#6431,#6432));
#1157=EDGE_LOOP('',(#6433,#6434,#6435,#6436));
#1158=EDGE_LOOP('',(#6437,#6438,#6439,#6440));
#1159=EDGE_LOOP('',(#6441,#6442,#6443,#6444));
#1160=EDGE_LOOP('',(#6445,#6446,#6447,#6448));
#1161=EDGE_LOOP('',(#6449,#6450,#6451,#6452));
#1162=EDGE_LOOP('',(#6453,#6454,#6455,#6456));
#1163=EDGE_LOOP('',(#6457,#6458,#6459,#6460));
#1164=EDGE_LOOP('',(#6461,#6462,#6463,#6464));
#1165=EDGE_LOOP('',(#6465,#6466,#6467,#6468));
#1166=EDGE_LOOP('',(#6469,#6470,#6471,#6472));
#1167=EDGE_LOOP('',(#6473,#6474,#6475,#6476));
#1168=EDGE_LOOP('',(#6477,#6478,#6479,#6480));
#1169=EDGE_LOOP('',(#6481,#6482,#6483,#6484));
#1170=EDGE_LOOP('',(#6485,#6486,#6487,#6488));
#1171=EDGE_LOOP('',(#6489,#6490,#6491,#6492));
#1172=EDGE_LOOP('',(#6493,#6494,#6495,#6496));
#1173=EDGE_LOOP('',(#6497,#6498,#6499,#6500));
#1174=EDGE_LOOP('',(#6501,#6502,#6503,#6504));
#1175=EDGE_LOOP('',(#6505,#6506,#6507,#6508));
#1176=EDGE_LOOP('',(#6509,#6510,#6511,#6512));
#1177=EDGE_LOOP('',(#6513,#6514,#6515,#6516));
#1178=EDGE_LOOP('',(#6517,#6518,#6519,#6520,#6521,#6522,#6523,#6524));
#1179=EDGE_LOOP('',(#6525,#6526,#6527,#6528));
#1180=EDGE_LOOP('',(#6529,#6530,#6531,#6532));
#1181=EDGE_LOOP('',(#6533,#6534,#6535,#6536));
#1182=EDGE_LOOP('',(#6537,#6538,#6539,#6540));
#1183=EDGE_LOOP('',(#6541,#6542,#6543,#6544));
#1184=EDGE_LOOP('',(#6545,#6546,#6547,#6548));
#1185=EDGE_LOOP('',(#6549,#6550,#6551,#6552));
#1186=EDGE_LOOP('',(#6553,#6554,#6555,#6556));
#1187=EDGE_LOOP('',(#6557,#6558,#6559,#6560));
#1188=EDGE_LOOP('',(#6561,#6562,#6563,#6564));
#1189=EDGE_LOOP('',(#6565,#6566,#6567,#6568));
#1190=EDGE_LOOP('',(#6569,#6570,#6571,#6572));
#1191=EDGE_LOOP('',(#6573,#6574,#6575,#6576));
#1192=EDGE_LOOP('',(#6577,#6578,#6579,#6580));
#1193=EDGE_LOOP('',(#6581,#6582,#6583,#6584));
#1194=EDGE_LOOP('',(#6585,#6586,#6587,#6588));
#1195=EDGE_LOOP('',(#6589,#6590,#6591,#6592));
#1196=EDGE_LOOP('',(#6593,#6594,#6595,#6596));
#1197=EDGE_LOOP('',(#6597,#6598,#6599,#6600));
#1198=EDGE_LOOP('',(#6601,#6602,#6603,#6604));
#1199=EDGE_LOOP('',(#6605,#6606,#6607,#6608));
#1200=EDGE_LOOP('',(#6609,#6610,#6611,#6612));
#1201=EDGE_LOOP('',(#6613,#6614,#6615,#6616));
#1202=EDGE_LOOP('',(#6617,#6618,#6619,#6620));
#1203=EDGE_LOOP('',(#6621,#6622,#6623,#6624));
#1204=EDGE_LOOP('',(#6625,#6626,#6627,#6628));
#1205=EDGE_LOOP('',(#6629,#6630,#6631,#6632));
#1206=EDGE_LOOP('',(#6633,#6634,#6635,#6636));
#1207=EDGE_LOOP('',(#6637,#6638,#6639,#6640));
#1208=EDGE_LOOP('',(#6641,#6642,#6643,#6644));
#1209=EDGE_LOOP('',(#6645,#6646,#6647,#6648,#6649,#6650,#6651,#6652));
#1210=EDGE_LOOP('',(#6653,#6654,#6655,#6656));
#1211=EDGE_LOOP('',(#6657,#6658,#6659,#6660));
#1212=EDGE_LOOP('',(#6661,#6662,#6663,#6664));
#1213=EDGE_LOOP('',(#6665,#6666,#6667,#6668));
#1214=EDGE_LOOP('',(#6669,#6670,#6671,#6672));
#1215=EDGE_LOOP('',(#6673,#6674,#6675,#6676));
#1216=EDGE_LOOP('',(#6677,#6678,#6679,#6680));
#1217=EDGE_LOOP('',(#6681,#6682,#6683,#6684));
#1218=EDGE_LOOP('',(#6685,#6686,#6687,#6688));
#1219=EDGE_LOOP('',(#6689,#6690,#6691,#6692));
#1220=EDGE_LOOP('',(#6693,#6694,#6695,#6696));
#1221=EDGE_LOOP('',(#6697,#6698,#6699,#6700));
#1222=EDGE_LOOP('',(#6701,#6702,#6703,#6704));
#1223=EDGE_LOOP('',(#6705,#6706,#6707,#6708));
#1224=EDGE_LOOP('',(#6709,#6710,#6711,#6712));
#1225=EDGE_LOOP('',(#6713,#6714,#6715,#6716));
#1226=EDGE_LOOP('',(#6717,#6718,#6719,#6720));
#1227=EDGE_LOOP('',(#6721,#6722,#6723,#6724));
#1228=EDGE_LOOP('',(#6725,#6726,#6727,#6728));
#1229=EDGE_LOOP('',(#6729,#6730,#6731,#6732));
#1230=EDGE_LOOP('',(#6733,#6734,#6735,#6736));
#1231=EDGE_LOOP('',(#6737,#6738,#6739,#6740));
#1232=EDGE_LOOP('',(#6741,#6742,#6743,#6744));
#1233=EDGE_LOOP('',(#6745,#6746,#6747,#6748));
#1234=EDGE_LOOP('',(#6749,#6750,#6751,#6752));
#1235=EDGE_LOOP('',(#6753,#6754,#6755,#6756));
#1236=EDGE_LOOP('',(#6757,#6758,#6759,#6760));
#1237=EDGE_LOOP('',(#6761,#6762,#6763,#6764));
#1238=EDGE_LOOP('',(#6765,#6766,#6767,#6768));
#1239=EDGE_LOOP('',(#6769,#6770,#6771,#6772));
#1240=EDGE_LOOP('',(#6773,#6774,#6775,#6776,#6777,#6778,#6779,#6780));
#1241=EDGE_LOOP('',(#6781,#6782,#6783,#6784));
#1242=EDGE_LOOP('',(#6785,#6786,#6787,#6788));
#1243=EDGE_LOOP('',(#6789,#6790,#6791,#6792));
#1244=EDGE_LOOP('',(#6793,#6794,#6795,#6796));
#1245=EDGE_LOOP('',(#6797,#6798,#6799,#6800));
#1246=EDGE_LOOP('',(#6801,#6802,#6803,#6804));
#1247=EDGE_LOOP('',(#6805,#6806,#6807,#6808));
#1248=EDGE_LOOP('',(#6809,#6810,#6811,#6812));
#1249=EDGE_LOOP('',(#6813,#6814,#6815,#6816));
#1250=EDGE_LOOP('',(#6817,#6818,#6819,#6820));
#1251=EDGE_LOOP('',(#6821,#6822,#6823,#6824));
#1252=EDGE_LOOP('',(#6825,#6826,#6827,#6828));
#1253=EDGE_LOOP('',(#6829,#6830,#6831,#6832));
#1254=EDGE_LOOP('',(#6833,#6834,#6835,#6836));
#1255=EDGE_LOOP('',(#6837,#6838,#6839,#6840));
#1256=EDGE_LOOP('',(#6841,#6842,#6843,#6844));
#1257=EDGE_LOOP('',(#6845,#6846,#6847,#6848));
#1258=EDGE_LOOP('',(#6849,#6850,#6851,#6852));
#1259=EDGE_LOOP('',(#6853,#6854,#6855,#6856));
#1260=EDGE_LOOP('',(#6857,#6858,#6859,#6860));
#1261=EDGE_LOOP('',(#6861,#6862,#6863,#6864));
#1262=EDGE_LOOP('',(#6865,#6866,#6867,#6868));
#1263=EDGE_LOOP('',(#6869,#6870,#6871,#6872));
#1264=EDGE_LOOP('',(#6873,#6874,#6875,#6876));
#1265=EDGE_LOOP('',(#6877,#6878,#6879,#6880));
#1266=EDGE_LOOP('',(#6881,#6882,#6883,#6884));
#1267=EDGE_LOOP('',(#6885,#6886,#6887,#6888));
#1268=EDGE_LOOP('',(#6889,#6890,#6891,#6892));
#1269=EDGE_LOOP('',(#6893,#6894,#6895,#6896));
#1270=EDGE_LOOP('',(#6897,#6898,#6899,#6900));
#1271=EDGE_LOOP('',(#6901,#6902,#6903,#6904,#6905,#6906));
#1272=EDGE_LOOP('',(#6907,#6908,#6909,#6910));
#1273=EDGE_LOOP('',(#6911,#6912,#6913,#6914));
#1274=EDGE_LOOP('',(#6915,#6916,#6917,#6918));
#1275=EDGE_LOOP('',(#6919,#6920,#6921,#6922));
#1276=EDGE_LOOP('',(#6923,#6924,#6925,#6926));
#1277=EDGE_LOOP('',(#6927,#6928,#6929,#6930));
#1278=EDGE_LOOP('',(#6931,#6932,#6933,#6934));
#1279=EDGE_LOOP('',(#6935,#6936,#6937,#6938));
#1280=EDGE_LOOP('',(#6939,#6940,#6941,#6942));
#1281=EDGE_LOOP('',(#6943,#6944,#6945,#6946));
#1282=EDGE_LOOP('',(#6947,#6948,#6949,#6950));
#1283=EDGE_LOOP('',(#6951,#6952,#6953,#6954));
#1284=EDGE_LOOP('',(#6955,#6956,#6957,#6958));
#1285=EDGE_LOOP('',(#6959,#6960,#6961,#6962));
#1286=EDGE_LOOP('',(#6963,#6964,#6965,#6966,#6967,#6968));
#1287=EDGE_LOOP('',(#6969,#6970,#6971,#6972));
#1288=EDGE_LOOP('',(#6973,#6974,#6975,#6976));
#1289=EDGE_LOOP('',(#6977,#6978,#6979,#6980));
#1290=EDGE_LOOP('',(#6981,#6982,#6983,#6984));
#1291=EDGE_LOOP('',(#6985,#6986,#6987,#6988));
#1292=EDGE_LOOP('',(#6989,#6990,#6991,#6992));
#1293=EDGE_LOOP('',(#6993,#6994,#6995,#6996));
#1294=EDGE_LOOP('',(#6997,#6998,#6999,#7000));
#1295=EDGE_LOOP('',(#7001,#7002,#7003,#7004));
#1296=EDGE_LOOP('',(#7005,#7006,#7007,#7008));
#1297=EDGE_LOOP('',(#7009,#7010,#7011,#7012));
#1298=EDGE_LOOP('',(#7013,#7014,#7015,#7016));
#1299=EDGE_LOOP('',(#7017,#7018,#7019,#7020));
#1300=EDGE_LOOP('',(#7021,#7022,#7023,#7024));
#1301=EDGE_LOOP('',(#7025,#7026,#7027,#7028));
#1302=EDGE_LOOP('',(#7029,#7030,#7031,#7032));
#1303=EDGE_LOOP('',(#7033,#7034,#7035,#7036));
#1304=EDGE_LOOP('',(#7037,#7038,#7039,#7040));
#1305=EDGE_LOOP('',(#7041,#7042,#7043,#7044));
#1306=EDGE_LOOP('',(#7045,#7046,#7047,#7048));
#1307=EDGE_LOOP('',(#7049,#7050,#7051,#7052));
#1308=EDGE_LOOP('',(#7053,#7054,#7055,#7056));
#1309=EDGE_LOOP('',(#7057,#7058,#7059,#7060));
#1310=EDGE_LOOP('',(#7061,#7062,#7063,#7064));
#1311=EDGE_LOOP('',(#7065,#7066,#7067,#7068));
#1312=EDGE_LOOP('',(#7069,#7070,#7071,#7072));
#1313=EDGE_LOOP('',(#7073,#7074,#7075,#7076));
#1314=EDGE_LOOP('',(#7077,#7078,#7079,#7080));
#1315=EDGE_LOOP('',(#7081,#7082,#7083,#7084));
#1316=EDGE_LOOP('',(#7085,#7086,#7087,#7088));
#1317=EDGE_LOOP('',(#7089,#7090,#7091,#7092));
#1318=EDGE_LOOP('',(#7093,#7094,#7095,#7096));
#1319=EDGE_LOOP('',(#7097,#7098,#7099,#7100));
#1320=EDGE_LOOP('',(#7101,#7102,#7103,#7104));
#1321=EDGE_LOOP('',(#7105,#7106,#7107,#7108));
#1322=EDGE_LOOP('',(#7109,#7110,#7111,#7112));
#1323=EDGE_LOOP('',(#7113,#7114,#7115,#7116));
#1324=EDGE_LOOP('',(#7117,#7118,#7119,#7120));
#1325=EDGE_LOOP('',(#7121,#7122,#7123,#7124));
#1326=EDGE_LOOP('',(#7125,#7126,#7127,#7128));
#1327=EDGE_LOOP('',(#7129,#7130,#7131,#7132));
#1328=EDGE_LOOP('',(#7133,#7134,#7135,#7136));
#1329=EDGE_LOOP('',(#7137,#7138,#7139,#7140));
#1330=EDGE_LOOP('',(#7141,#7142,#7143,#7144));
#1331=EDGE_LOOP('',(#7145,#7146,#7147,#7148,#7149,#7150,#7151,#7152));
#1332=EDGE_LOOP('',(#7153,#7154,#7155,#7156));
#1333=EDGE_LOOP('',(#7157,#7158,#7159,#7160));
#1334=EDGE_LOOP('',(#7161,#7162,#7163,#7164));
#1335=EDGE_LOOP('',(#7165,#7166,#7167,#7168));
#1336=EDGE_LOOP('',(#7169,#7170,#7171,#7172));
#1337=EDGE_LOOP('',(#7173,#7174,#7175,#7176));
#1338=EDGE_LOOP('',(#7177,#7178,#7179,#7180));
#1339=EDGE_LOOP('',(#7181,#7182,#7183,#7184));
#1340=EDGE_LOOP('',(#7185,#7186,#7187,#7188));
#1341=EDGE_LOOP('',(#7189,#7190,#7191,#7192));
#1342=EDGE_LOOP('',(#7193,#7194,#7195,#7196));
#1343=EDGE_LOOP('',(#7197,#7198,#7199,#7200));
#1344=EDGE_LOOP('',(#7201,#7202,#7203,#7204));
#1345=EDGE_LOOP('',(#7205,#7206,#7207,#7208));
#1346=EDGE_LOOP('',(#7209,#7210,#7211,#7212));
#1347=EDGE_LOOP('',(#7213,#7214,#7215,#7216));
#1348=EDGE_LOOP('',(#7217,#7218,#7219,#7220));
#1349=EDGE_LOOP('',(#7221,#7222,#7223,#7224));
#1350=EDGE_LOOP('',(#7225,#7226,#7227,#7228));
#1351=EDGE_LOOP('',(#7229,#7230,#7231,#7232));
#1352=EDGE_LOOP('',(#7233,#7234,#7235,#7236));
#1353=EDGE_LOOP('',(#7237,#7238,#7239,#7240));
#1354=EDGE_LOOP('',(#7241,#7242,#7243,#7244));
#1355=EDGE_LOOP('',(#7245,#7246,#7247,#7248));
#1356=EDGE_LOOP('',(#7249,#7250,#7251,#7252));
#1357=EDGE_LOOP('',(#7253,#7254,#7255,#7256));
#1358=EDGE_LOOP('',(#7257,#7258,#7259,#7260));
#1359=EDGE_LOOP('',(#7261,#7262,#7263,#7264));
#1360=EDGE_LOOP('',(#7265,#7266,#7267,#7268));
#1361=EDGE_LOOP('',(#7269,#7270,#7271,#7272,#7273,#7274,#7275,#7276));
#1362=EDGE_LOOP('',(#7277,#7278,#7279,#7280));
#1363=EDGE_LOOP('',(#7281,#7282,#7283,#7284));
#1364=EDGE_LOOP('',(#7285,#7286,#7287,#7288));
#1365=EDGE_LOOP('',(#7289,#7290,#7291,#7292));
#1366=EDGE_LOOP('',(#7293,#7294,#7295,#7296));
#1367=EDGE_LOOP('',(#7297,#7298,#7299,#7300));
#1368=EDGE_LOOP('',(#7301,#7302,#7303,#7304));
#1369=EDGE_LOOP('',(#7305,#7306,#7307,#7308));
#1370=EDGE_LOOP('',(#7309,#7310,#7311,#7312));
#1371=EDGE_LOOP('',(#7313,#7314,#7315,#7316));
#1372=EDGE_LOOP('',(#7317,#7318,#7319,#7320));
#1373=EDGE_LOOP('',(#7321,#7322,#7323,#7324));
#1374=EDGE_LOOP('',(#7325,#7326,#7327,#7328));
#1375=EDGE_LOOP('',(#7329,#7330,#7331,#7332));
#1376=EDGE_LOOP('',(#7333,#7334,#7335,#7336));
#1377=EDGE_LOOP('',(#7337,#7338,#7339,#7340));
#1378=EDGE_LOOP('',(#7341,#7342,#7343,#7344));
#1379=EDGE_LOOP('',(#7345,#7346,#7347,#7348));
#1380=EDGE_LOOP('',(#7349,#7350,#7351,#7352));
#1381=EDGE_LOOP('',(#7353,#7354,#7355,#7356));
#1382=EDGE_LOOP('',(#7357,#7358,#7359,#7360));
#1383=EDGE_LOOP('',(#7361,#7362,#7363,#7364));
#1384=EDGE_LOOP('',(#7365,#7366,#7367,#7368));
#1385=EDGE_LOOP('',(#7369,#7370,#7371,#7372));
#1386=EDGE_LOOP('',(#7373,#7374,#7375,#7376));
#1387=EDGE_LOOP('',(#7377,#7378,#7379,#7380));
#1388=EDGE_LOOP('',(#7381,#7382,#7383,#7384));
#1389=EDGE_LOOP('',(#7385,#7386,#7387,#7388));
#1390=EDGE_LOOP('',(#7389,#7390,#7391,#7392));
#1391=EDGE_LOOP('',(#7393,#7394,#7395,#7396));
#1392=EDGE_LOOP('',(#7397,#7398,#7399,#7400));
#1393=EDGE_LOOP('',(#7401,#7402,#7403,#7404));
#1394=EDGE_LOOP('',(#7405,#7406,#7407,#7408));
#1395=EDGE_LOOP('',(#7409,#7410,#7411,#7412));
#1396=EDGE_LOOP('',(#7413,#7414,#7415,#7416));
#1397=EDGE_LOOP('',(#7417,#7418,#7419,#7420));
#1398=EDGE_LOOP('',(#7421,#7422,#7423,#7424));
#1399=EDGE_LOOP('',(#7425,#7426,#7427,#7428));
#1400=EDGE_LOOP('',(#7429,#7430,#7431,#7432));
#1401=EDGE_LOOP('',(#7433,#7434,#7435,#7436));
#1402=EDGE_LOOP('',(#7437,#7438,#7439,#7440));
#1403=EDGE_LOOP('',(#7441,#7442,#7443,#7444));
#1404=EDGE_LOOP('',(#7445,#7446,#7447,#7448));
#1405=EDGE_LOOP('',(#7449,#7450,#7451,#7452));
#1406=EDGE_LOOP('',(#7453,#7454,#7455,#7456));
#1407=EDGE_LOOP('',(#7457,#7458,#7459,#7460));
#1408=EDGE_LOOP('',(#7461,#7462,#7463,#7464,#7465,#7466,#7467,#7468,#7469,
#7470,#7471,#7472,#7473,#7474,#7475,#7476,#7477,#7478,#7479,#7480));
#1409=EDGE_LOOP('',(#7481,#7482,#7483,#7484,#7485,#7486,#7487,#7488,#7489,
#7490,#7491,#7492,#7493,#7494,#7495,#7496,#7497,#7498,#7499,#7500));
#1410=EDGE_LOOP('',(#7501));
#1411=EDGE_LOOP('',(#7502,#7503,#7504,#7505));
#1412=EDGE_LOOP('',(#7506,#7507,#7508,#7509));
#1413=EDGE_LOOP('',(#7510,#7511,#7512,#7513));
#1414=EDGE_LOOP('',(#7514,#7515,#7516,#7517));
#1415=EDGE_LOOP('',(#7518,#7519,#7520,#7521));
#1416=EDGE_LOOP('',(#7522,#7523,#7524,#7525));
#1417=EDGE_LOOP('',(#7526,#7527,#7528,#7529));
#1418=EDGE_LOOP('',(#7530,#7531,#7532,#7533));
#1419=EDGE_LOOP('',(#7534));
#1420=EDGE_LOOP('',(#7535,#7536,#7537,#7538,#7539));
#1421=EDGE_LOOP('',(#7540,#7541,#7542,#7543));
#1422=EDGE_LOOP('',(#7544,#7545,#7546,#7547,#7548,#7549,#7550,#7551,#7552,
#7553,#7554,#7555,#7556,#7557,#7558,#7559,#7560,#7561,#7562,#7563,#7564,
#7565,#7566,#7567,#7568,#7569,#7570,#7571,#7572,#7573,#7574,#7575,#7576,
#7577));
#1423=EDGE_LOOP('',(#7578,#7579,#7580,#7581,#7582,#7583,#7584,#7585,#7586,
#7587,#7588,#7589,#7590,#7591,#7592,#7593,#7594,#7595,#7596,#7597,#7598,
#7599,#7600,#7601,#7602,#7603,#7604,#7605,#7606,#7607,#7608,#7609,#7610,
#7611));
#1424=EDGE_LOOP('',(#7612,#7613,#7614,#7615));
#1425=EDGE_LOOP('',(#7616,#7617,#7618,#7619,#7620));
#1426=EDGE_LOOP('',(#7621,#7622,#7623,#7624));
#1427=EDGE_LOOP('',(#7625,#7626,#7627,#7628,#7629,#7630,#7631,#7632,#7633,
#7634,#7635,#7636,#7637,#7638,#7639,#7640,#7641,#7642,#7643,#7644,#7645,
#7646,#7647,#7648,#7649,#7650,#7651,#7652,#7653,#7654,#7655,#7656,#7657,
#7658));
#1428=EDGE_LOOP('',(#7659,#7660,#7661,#7662,#7663,#7664,#7665,#7666,#7667,
#7668,#7669,#7670,#7671,#7672,#7673,#7674,#7675,#7676,#7677,#7678,#7679,
#7680,#7681,#7682,#7683,#7684,#7685,#7686,#7687,#7688,#7689,#7690,#7691,
#7692));
#1429=EDGE_LOOP('',(#7693,#7694,#7695,#7696));
#1430=EDGE_LOOP('',(#7697,#7698,#7699));
#1431=EDGE_LOOP('',(#7700,#7701,#7702,#7703,#7704,#7705));
#1432=EDGE_LOOP('',(#7706,#7707,#7708));
#1433=EDGE_LOOP('',(#7709,#7710,#7711,#7712));
#1434=EDGE_LOOP('',(#7713,#7714,#7715,#7716,#7717,#7718,#7719,#7720,#7721,
#7722,#7723,#7724,#7725,#7726,#7727,#7728,#7729,#7730,#7731,#7732,#7733,
#7734,#7735,#7736,#7737,#7738,#7739,#7740,#7741,#7742,#7743,#7744,#7745,
#7746,#7747));
#1435=EDGE_LOOP('',(#7748,#7749,#7750,#7751,#7752,#7753,#7754,#7755,#7756,
#7757,#7758,#7759,#7760,#7761,#7762,#7763,#7764,#7765,#7766,#7767,#7768,
#7769,#7770,#7771,#7772,#7773,#7774,#7775,#7776,#7777,#7778,#7779,#7780,
#7781,#7782));
#1436=EDGE_LOOP('',(#7783,#7784,#7785));
#1437=EDGE_LOOP('',(#7786,#7787,#7788));
#1438=EDGE_LOOP('',(#7789,#7790,#7791,#7792,#7793,#7794));
#1439=EDGE_LOOP('',(#7795,#7796,#7797));
#1440=EDGE_LOOP('',(#7798,#7799,#7800,#7801));
#1441=EDGE_LOOP('',(#7802,#7803,#7804,#7805,#7806,#7807,#7808,#7809,#7810,
#7811,#7812,#7813,#7814,#7815,#7816,#7817,#7818,#7819,#7820,#7821,#7822,
#7823,#7824,#7825,#7826,#7827,#7828,#7829,#7830,#7831,#7832,#7833,#7834,
#7835,#7836));
#1442=EDGE_LOOP('',(#7837,#7838,#7839,#7840,#7841,#7842,#7843,#7844,#7845,
#7846,#7847,#7848,#7849,#7850,#7851,#7852,#7853,#7854,#7855,#7856,#7857,
#7858,#7859,#7860,#7861,#7862,#7863,#7864,#7865,#7866,#7867,#7868,#7869,
#7870,#7871));
#1443=EDGE_LOOP('',(#7872,#7873,#7874));
#1444=EDGE_LOOP('',(#7875,#7876,#7877,#7878));
#1445=EDGE_LOOP('',(#7879));
#1446=EDGE_LOOP('',(#7880));
#1447=EDGE_LOOP('',(#7881,#7882,#7883,#7884));
#1448=EDGE_LOOP('',(#7885,#7886,#7887,#7888));
#1449=EDGE_LOOP('',(#7889,#7890,#7891,#7892));
#1450=EDGE_LOOP('',(#7893,#7894,#7895,#7896,#7897,#7898,#7899,#7900,#7901,
#7902,#7903,#7904,#7905,#7906,#7907,#7908,#7909,#7910,#7911,#7912,#7913,
#7914,#7915,#7916,#7917,#7918,#7919,#7920,#7921,#7922,#7923,#7924,#7925,
#7926,#7927,#7928));
#1451=EDGE_LOOP('',(#7929,#7930,#7931,#7932,#7933,#7934,#7935,#7936,#7937,
#7938,#7939,#7940,#7941,#7942,#7943,#7944,#7945,#7946,#7947,#7948,#7949,
#7950,#7951,#7952,#7953,#7954,#7955,#7956,#7957,#7958,#7959,#7960,#7961,
#7962,#7963));
#1452=EDGE_LOOP('',(#7964,#7965,#7966,#7967));
#1453=EDGE_LOOP('',(#7968,#7969,#7970,#7971));
#1454=EDGE_LOOP('',(#7972,#7973,#7974,#7975));
#1455=EDGE_LOOP('',(#7976,#7977,#7978,#7979,#7980,#7981,#7982,#7983,#7984,
#7985,#7986,#7987,#7988,#7989,#7990,#7991,#7992,#7993,#7994,#7995,#7996,
#7997,#7998,#7999,#8000,#8001,#8002,#8003,#8004,#8005,#8006,#8007,#8008,
#8009,#8010,#8011));
#1456=EDGE_LOOP('',(#8012,#8013,#8014,#8015,#8016,#8017,#8018,#8019,#8020,
#8021,#8022,#8023,#8024,#8025,#8026,#8027,#8028,#8029,#8030,#8031,#8032,
#8033,#8034,#8035,#8036,#8037,#8038,#8039,#8040,#8041,#8042,#8043,#8044,
#8045,#8046));
#1457=EDGE_LOOP('',(#8047,#8048,#8049,#8050));
#1458=EDGE_LOOP('',(#8051,#8052,#8053,#8054));
#1459=EDGE_LOOP('',(#8055,#8056,#8057,#8058));
#1460=EDGE_LOOP('',(#8059,#8060,#8061,#8062,#8063,#8064,#8065,#8066,#8067,
#8068,#8069,#8070,#8071,#8072,#8073,#8074,#8075,#8076,#8077,#8078,#8079,
#8080,#8081,#8082,#8083,#8084,#8085,#8086,#8087,#8088,#8089,#8090,#8091,
#8092,#8093,#8094));
#1461=EDGE_LOOP('',(#8095,#8096,#8097,#8098,#8099,#8100,#8101,#8102,#8103,
#8104,#8105,#8106,#8107,#8108,#8109,#8110,#8111,#8112,#8113,#8114,#8115,
#8116,#8117,#8118,#8119,#8120,#8121,#8122,#8123,#8124,#8125,#8126,#8127,
#8128,#8129));
#1462=EDGE_LOOP('',(#8130,#8131,#8132,#8133));
#1463=EDGE_LOOP('',(#8134,#8135,#8136,#8137));
#1464=EDGE_LOOP('',(#8138,#8139,#8140,#8141));
#1465=EDGE_LOOP('',(#8142,#8143,#8144,#8145,#8146,#8147,#8148,#8149,#8150,
#8151,#8152,#8153,#8154,#8155,#8156,#8157,#8158,#8159,#8160,#8161,#8162,
#8163,#8164,#8165,#8166,#8167,#8168,#8169,#8170,#8171,#8172,#8173,#8174,
#8175,#8176,#8177));
#1466=EDGE_LOOP('',(#8178,#8179,#8180,#8181,#8182,#8183,#8184,#8185,#8186,
#8187,#8188,#8189,#8190,#8191,#8192,#8193,#8194,#8195,#8196,#8197,#8198,
#8199,#8200,#8201,#8202,#8203,#8204,#8205,#8206,#8207,#8208,#8209,#8210,
#8211,#8212));
#1467=EDGE_LOOP('',(#8213,#8214,#8215,#8216));
#1468=EDGE_LOOP('',(#8217));
#1469=EDGE_LOOP('',(#8218));
#1470=EDGE_LOOP('',(#8219));
#1471=EDGE_LOOP('',(#8220));
#1472=EDGE_LOOP('',(#8221,#8222,#8223,#8224));
#1473=EDGE_LOOP('',(#8225,#8226,#8227,#8228));
#1474=EDGE_LOOP('',(#8229,#8230,#8231,#8232));
#1475=EDGE_LOOP('',(#8233,#8234,#8235,#8236));
#1476=EDGE_LOOP('',(#8237,#8238,#8239,#8240));
#1477=EDGE_LOOP('',(#8241,#8242,#8243,#8244));
#1478=EDGE_LOOP('',(#8245,#8246,#8247,#8248));
#1479=EDGE_LOOP('',(#8249,#8250,#8251,#8252));
#1480=EDGE_LOOP('',(#8253,#8254,#8255,#8256,#8257,#8258,#8259,#8260,#8261,
#8262,#8263,#8264,#8265));
#1481=EDGE_LOOP('',(#8266,#8267,#8268,#8269));
#1482=EDGE_LOOP('',(#8270,#8271,#8272,#8273));
#1483=EDGE_LOOP('',(#8274,#8275,#8276,#8277));
#1484=EDGE_LOOP('',(#8278,#8279,#8280,#8281));
#1485=EDGE_LOOP('',(#8282,#8283,#8284,#8285));
#1486=EDGE_LOOP('',(#8286,#8287,#8288,#8289));
#1487=EDGE_LOOP('',(#8290,#8291,#8292,#8293));
#1488=EDGE_LOOP('',(#8294,#8295,#8296,#8297,#8298,#8299,#8300,#8301,#8302,
#8303,#8304,#8305,#8306));
#1489=EDGE_LOOP('',(#8307,#8308,#8309,#8310));
#1490=EDGE_LOOP('',(#8311,#8312,#8313,#8314));
#1491=EDGE_LOOP('',(#8315,#8316,#8317,#8318));
#1492=EDGE_LOOP('',(#8319));
#1493=EDGE_LOOP('',(#8320));
#1494=EDGE_LOOP('',(#8321));
#1495=EDGE_LOOP('',(#8322));
#1496=EDGE_LOOP('',(#8323));
#1497=EDGE_LOOP('',(#8324));
#1498=EDGE_LOOP('',(#8325));
#1499=EDGE_LOOP('',(#8326));
#1500=EDGE_LOOP('',(#8327));
#1501=EDGE_LOOP('',(#8328));
#1502=EDGE_LOOP('',(#8329));
#1503=EDGE_LOOP('',(#8330));
#1504=EDGE_LOOP('',(#8331));
#1505=EDGE_LOOP('',(#8332));
#1506=EDGE_LOOP('',(#8333));
#1507=EDGE_LOOP('',(#8334));
#1508=EDGE_LOOP('',(#8335));
#1509=EDGE_LOOP('',(#8336));
#1510=EDGE_LOOP('',(#8337,#8338,#8339,#8340));
#1511=EDGE_LOOP('',(#8341,#8342,#8343,#8344));
#1512=EDGE_LOOP('',(#8345,#8346,#8347,#8348));
#1513=EDGE_LOOP('',(#8349,#8350,#8351,#8352));
#1514=EDGE_LOOP('',(#8353,#8354,#8355,#8356));
#1515=EDGE_LOOP('',(#8357,#8358,#8359,#8360));
#1516=EDGE_LOOP('',(#8361));
#1517=EDGE_LOOP('',(#8362));
#1518=EDGE_LOOP('',(#8363));
#1519=EDGE_LOOP('',(#8364));
#1520=EDGE_LOOP('',(#8365));
#1521=EDGE_LOOP('',(#8366));
#1522=EDGE_LOOP('',(#8367));
#1523=EDGE_LOOP('',(#8368));
#1524=EDGE_LOOP('',(#8369));
#1525=EDGE_LOOP('',(#8370));
#1526=EDGE_LOOP('',(#8371));
#1527=EDGE_LOOP('',(#8372));
#1528=EDGE_LOOP('',(#8373));
#1529=EDGE_LOOP('',(#8374));
#1530=EDGE_LOOP('',(#8375));
#1531=EDGE_LOOP('',(#8376));
#1532=EDGE_LOOP('',(#8377));
#1533=EDGE_LOOP('',(#8378));
#1534=EDGE_LOOP('',(#8379,#8380,#8381,#8382));
#1535=EDGE_LOOP('',(#8383,#8384,#8385,#8386));
#1536=EDGE_LOOP('',(#8387,#8388,#8389,#8390));
#1537=EDGE_LOOP('',(#8391,#8392,#8393,#8394));
#1538=EDGE_LOOP('',(#8395,#8396,#8397,#8398));
#1539=EDGE_LOOP('',(#8399,#8400,#8401,#8402));
#1540=EDGE_LOOP('',(#8403,#8404,#8405,#8406));
#1541=EDGE_LOOP('',(#8407,#8408,#8409,#8410));
#1542=EDGE_LOOP('',(#8411,#8412,#8413,#8414));
#1543=EDGE_LOOP('',(#8415,#8416,#8417,#8418));
#1544=EDGE_LOOP('',(#8419,#8420,#8421,#8422));
#1545=EDGE_LOOP('',(#8423,#8424,#8425,#8426));
#1546=EDGE_LOOP('',(#8427,#8428,#8429,#8430));
#1547=EDGE_LOOP('',(#8431,#8432,#8433,#8434));
#1548=EDGE_LOOP('',(#8435,#8436,#8437,#8438));
#1549=EDGE_LOOP('',(#8439,#8440,#8441,#8442));
#1550=EDGE_LOOP('',(#8443,#8444,#8445,#8446));
#1551=EDGE_LOOP('',(#8447));
#1552=EDGE_LOOP('',(#8448));
#1553=EDGE_LOOP('',(#8449));
#1554=EDGE_LOOP('',(#8450));
#1555=EDGE_LOOP('',(#8451,#8452,#8453,#8454));
#1556=EDGE_LOOP('',(#8455));
#1557=EDGE_LOOP('',(#8456));
#1558=EDGE_LOOP('',(#8457));
#1559=EDGE_LOOP('',(#8458));
#1560=EDGE_LOOP('',(#8459,#8460,#8461,#8462));
#1561=EDGE_LOOP('',(#8463,#8464,#8465,#8466));
#1562=EDGE_LOOP('',(#8467,#8468,#8469,#8470));
#1563=EDGE_LOOP('',(#8471,#8472,#8473,#8474));
#1564=EDGE_LOOP('',(#8475,#8476,#8477,#8478));
#1565=EDGE_LOOP('',(#8479,#8480,#8481,#8482));
#1566=EDGE_LOOP('',(#8483,#8484,#8485,#8486));
#1567=EDGE_LOOP('',(#8487,#8488,#8489,#8490));
#1568=EDGE_LOOP('',(#8491,#8492,#8493,#8494));
#1569=EDGE_LOOP('',(#8495,#8496,#8497,#8498));
#1570=EDGE_LOOP('',(#8499,#8500,#8501,#8502));
#1571=EDGE_LOOP('',(#8503,#8504,#8505,#8506));
#1572=EDGE_LOOP('',(#8507,#8508,#8509,#8510));
#1573=EDGE_LOOP('',(#8511,#8512,#8513,#8514));
#1574=EDGE_LOOP('',(#8515));
#1575=EDGE_LOOP('',(#8516));
#1576=EDGE_LOOP('',(#8517));
#1577=EDGE_LOOP('',(#8518));
#1578=EDGE_LOOP('',(#8519,#8520,#8521,#8522));
#1579=EDGE_LOOP('',(#8523,#8524,#8525,#8526));
#1580=EDGE_LOOP('',(#8527));
#1581=EDGE_LOOP('',(#8528));
#1582=EDGE_LOOP('',(#8529));
#1583=EDGE_LOOP('',(#8530));
#1584=EDGE_LOOP('',(#8531,#8532,#8533,#8534));
#1585=EDGE_LOOP('',(#8535,#8536,#8537,#8538));
#1586=EDGE_LOOP('',(#8539));
#1587=EDGE_LOOP('',(#8540));
#1588=EDGE_LOOP('',(#8541));
#1589=EDGE_LOOP('',(#8542));
#1590=EDGE_LOOP('',(#8543,#8544,#8545,#8546));
#1591=EDGE_LOOP('',(#8547,#8548,#8549,#8550));
#1592=EDGE_LOOP('',(#8551,#8552,#8553,#8554));
#1593=EDGE_LOOP('',(#8555,#8556,#8557,#8558));
#1594=EDGE_LOOP('',(#8559,#8560,#8561,#8562));
#1595=EDGE_LOOP('',(#8563,#8564,#8565,#8566));
#1596=EDGE_LOOP('',(#8567,#8568,#8569,#8570));
#1597=EDGE_LOOP('',(#8571,#8572,#8573,#8574));
#1598=EDGE_LOOP('',(#8575,#8576,#8577,#8578));
#1599=EDGE_LOOP('',(#8579,#8580,#8581,#8582));
#1600=EDGE_LOOP('',(#8583,#8584,#8585,#8586));
#1601=EDGE_LOOP('',(#8587,#8588,#8589,#8590));
#1602=EDGE_LOOP('',(#8591,#8592,#8593,#8594));
#1603=EDGE_LOOP('',(#8595,#8596,#8597,#8598));
#1604=EDGE_LOOP('',(#8599,#8600,#8601,#8602));
#1605=EDGE_LOOP('',(#8603,#8604,#8605,#8606));
#1606=EDGE_LOOP('',(#8607,#8608,#8609,#8610));
#1607=EDGE_LOOP('',(#8611,#8612,#8613,#8614));
#1608=EDGE_LOOP('',(#8615,#8616,#8617,#8618));
#1609=EDGE_LOOP('',(#8619,#8620,#8621,#8622));
#1610=EDGE_LOOP('',(#8623,#8624,#8625,#8626));
#1611=EDGE_LOOP('',(#8627,#8628,#8629,#8630));
#1612=EDGE_LOOP('',(#8631,#8632,#8633,#8634));
#1613=EDGE_LOOP('',(#8635));
#1614=EDGE_LOOP('',(#8636));
#1615=EDGE_LOOP('',(#8637));
#1616=EDGE_LOOP('',(#8638));
#1617=EDGE_LOOP('',(#8639));
#1618=EDGE_LOOP('',(#8640));
#1619=EDGE_LOOP('',(#8641));
#1620=EDGE_LOOP('',(#8642));
#1621=EDGE_LOOP('',(#8643));
#1622=EDGE_LOOP('',(#8644));
#1623=EDGE_LOOP('',(#8645));
#1624=EDGE_LOOP('',(#8646));
#1625=EDGE_LOOP('',(#8647));
#1626=EDGE_LOOP('',(#8648));
#1627=EDGE_LOOP('',(#8649));
#1628=EDGE_LOOP('',(#8650));
#1629=EDGE_LOOP('',(#8651));
#1630=EDGE_LOOP('',(#8652));
#1631=EDGE_LOOP('',(#8653,#8654,#8655,#8656));
#1632=EDGE_LOOP('',(#8657));
#1633=EDGE_LOOP('',(#8658));
#1634=EDGE_LOOP('',(#8659));
#1635=EDGE_LOOP('',(#8660));
#1636=EDGE_LOOP('',(#8661));
#1637=EDGE_LOOP('',(#8662));
#1638=EDGE_LOOP('',(#8663));
#1639=EDGE_LOOP('',(#8664));
#1640=EDGE_LOOP('',(#8665));
#1641=EDGE_LOOP('',(#8666));
#1642=EDGE_LOOP('',(#8667));
#1643=EDGE_LOOP('',(#8668));
#1644=EDGE_LOOP('',(#8669));
#1645=EDGE_LOOP('',(#8670));
#1646=EDGE_LOOP('',(#8671));
#1647=EDGE_LOOP('',(#8672));
#1648=EDGE_LOOP('',(#8673));
#1649=EDGE_LOOP('',(#8674));
#1650=EDGE_LOOP('',(#8675,#8676,#8677,#8678));
#1651=EDGE_LOOP('',(#8679,#8680,#8681,#8682));
#1652=EDGE_LOOP('',(#8683,#8684,#8685,#8686));
#1653=EDGE_LOOP('',(#8687,#8688,#8689,#8690));
#1654=EDGE_LOOP('',(#8691,#8692,#8693,#8694));
#1655=EDGE_LOOP('',(#8695,#8696,#8697,#8698));
#1656=EDGE_LOOP('',(#8699,#8700,#8701,#8702));
#1657=EDGE_LOOP('',(#8703,#8704,#8705,#8706));
#1658=EDGE_LOOP('',(#8707,#8708,#8709,#8710));
#1659=EDGE_LOOP('',(#8711,#8712,#8713,#8714));
#1660=EDGE_LOOP('',(#8715,#8716,#8717,#8718));
#1661=EDGE_LOOP('',(#8719,#8720,#8721,#8722));
#1662=EDGE_LOOP('',(#8723));
#1663=EDGE_LOOP('',(#8724));
#1664=EDGE_LOOP('',(#8725));
#1665=EDGE_LOOP('',(#8726));
#1666=EDGE_LOOP('',(#8727));
#1667=EDGE_LOOP('',(#8728));
#1668=EDGE_LOOP('',(#8729));
#1669=EDGE_LOOP('',(#8730,#8731,#8732,#8733));
#1670=EDGE_LOOP('',(#8734));
#1671=EDGE_LOOP('',(#8735));
#1672=EDGE_LOOP('',(#8736));
#1673=EDGE_LOOP('',(#8737));
#1674=EDGE_LOOP('',(#8738));
#1675=EDGE_LOOP('',(#8739));
#1676=EDGE_LOOP('',(#8740));
#1677=EDGE_LOOP('',(#8741,#8742,#8743,#8744));
#1678=EDGE_LOOP('',(#8745,#8746,#8747,#8748));
#1679=EDGE_LOOP('',(#8749,#8750,#8751,#8752));
#1680=EDGE_LOOP('',(#8753,#8754,#8755,#8756));
#1681=EDGE_LOOP('',(#8757,#8758,#8759,#8760));
#1682=EDGE_LOOP('',(#8761,#8762,#8763,#8764));
#1683=EDGE_LOOP('',(#8765,#8766,#8767,#8768));
#1684=EDGE_LOOP('',(#8769,#8770,#8771,#8772));
#1685=EDGE_LOOP('',(#8773,#8774,#8775,#8776));
#1686=EDGE_LOOP('',(#8777,#8778,#8779,#8780));
#1687=EDGE_LOOP('',(#8781,#8782,#8783,#8784));
#1688=EDGE_LOOP('',(#8785,#8786,#8787,#8788));
#1689=EDGE_LOOP('',(#8789,#8790,#8791,#8792));
#1690=EDGE_LOOP('',(#8793,#8794,#8795,#8796));
#1691=EDGE_LOOP('',(#8797,#8798,#8799,#8800));
#1692=EDGE_LOOP('',(#8801,#8802,#8803,#8804));
#1693=EDGE_LOOP('',(#8805,#8806,#8807,#8808));
#1694=EDGE_LOOP('',(#8809,#8810,#8811,#8812));
#1695=EDGE_LOOP('',(#8813,#8814,#8815,#8816));
#1696=EDGE_LOOP('',(#8817,#8818,#8819,#8820));
#1697=EDGE_LOOP('',(#8821,#8822,#8823,#8824));
#1698=EDGE_LOOP('',(#8825,#8826,#8827,#8828));
#1699=EDGE_LOOP('',(#8829,#8830,#8831,#8832));
#1700=EDGE_LOOP('',(#8833,#8834,#8835,#8836));
#1701=EDGE_LOOP('',(#8837,#8838,#8839,#8840));
#1702=EDGE_LOOP('',(#8841,#8842,#8843,#8844));
#1703=EDGE_LOOP('',(#8845,#8846,#8847,#8848));
#1704=EDGE_LOOP('',(#8849,#8850,#8851,#8852));
#1705=EDGE_LOOP('',(#8853,#8854,#8855,#8856));
#1706=EDGE_LOOP('',(#8857,#8858,#8859,#8860));
#1707=EDGE_LOOP('',(#8861,#8862,#8863,#8864));
#1708=EDGE_LOOP('',(#8865,#8866,#8867,#8868));
#1709=EDGE_LOOP('',(#8869,#8870,#8871,#8872,#8873,#8874,#8875,#8876));
#1710=EDGE_LOOP('',(#8877,#8878,#8879,#8880,#8881,#8882,#8883,#8884,#8885,
#8886,#8887,#8888,#8889,#8890,#8891,#8892,#8893,#8894,#8895,#8896,#8897,
#8898,#8899,#8900,#8901,#8902,#8903,#8904,#8905,#8906,#8907,#8908,#8909,
#8910,#8911,#8912));
#1711=EDGE_LOOP('',(#8913,#8914,#8915,#8916));
#1712=EDGE_LOOP('',(#8917,#8918,#8919,#8920,#8921,#8922,#8923,#8924,#8925,
#8926,#8927,#8928,#8929,#8930,#8931,#8932,#8933,#8934,#8935,#8936,#8937,
#8938,#8939,#8940,#8941,#8942,#8943,#8944,#8945,#8946,#8947,#8948,#8949,
#8950,#8951,#8952,#8953));
#1713=EDGE_LOOP('',(#8954,#8955,#8956,#8957));
#1714=EDGE_LOOP('',(#8958,#8959,#8960,#8961));
#1715=EDGE_LOOP('',(#8962,#8963,#8964,#8965));
#1716=EDGE_LOOP('',(#8966,#8967,#8968,#8969));
#1717=EDGE_LOOP('',(#8970,#8971,#8972,#8973));
#1718=EDGE_LOOP('',(#8974,#8975,#8976,#8977));
#1719=EDGE_LOOP('',(#8978,#8979,#8980,#8981));
#1720=EDGE_LOOP('',(#8982,#8983,#8984,#8985,#8986,#8987));
#1721=EDGE_LOOP('',(#8988));
#1722=EDGE_LOOP('',(#8989,#8990,#8991,#8992));
#1723=EDGE_LOOP('',(#8993,#8994,#8995,#8996));
#1724=EDGE_LOOP('',(#8997));
#1725=EDGE_LOOP('',(#8998,#8999,#9000,#9001,#9002,#9003));
#1726=EDGE_LOOP('',(#9004));
#1727=EDGE_LOOP('',(#9005,#9006,#9007,#9008));
#1728=EDGE_LOOP('',(#9009,#9010,#9011,#9012));
#1729=EDGE_LOOP('',(#9013,#9014,#9015,#9016));
#1730=EDGE_LOOP('',(#9017,#9018,#9019,#9020));
#1731=EDGE_LOOP('',(#9021,#9022,#9023,#9024));
#1732=EDGE_LOOP('',(#9025,#9026,#9027,#9028));
#1733=EDGE_LOOP('',(#9029,#9030,#9031,#9032));
#1734=EDGE_LOOP('',(#9033,#9034,#9035,#9036));
#1735=EDGE_LOOP('',(#9037,#9038,#9039,#9040));
#1736=EDGE_LOOP('',(#9041,#9042,#9043,#9044));
#1737=EDGE_LOOP('',(#9045,#9046,#9047,#9048));
#1738=EDGE_LOOP('',(#9049,#9050,#9051,#9052));
#1739=EDGE_LOOP('',(#9053,#9054,#9055,#9056));
#1740=EDGE_LOOP('',(#9057,#9058,#9059,#9060));
#1741=EDGE_LOOP('',(#9061,#9062,#9063,#9064));
#1742=EDGE_LOOP('',(#9065,#9066,#9067,#9068));
#1743=EDGE_LOOP('',(#9069,#9070,#9071,#9072));
#1744=EDGE_LOOP('',(#9073,#9074,#9075,#9076));
#1745=EDGE_LOOP('',(#9077,#9078,#9079,#9080));
#1746=EDGE_LOOP('',(#9081,#9082,#9083,#9084));
#1747=EDGE_LOOP('',(#9085,#9086,#9087,#9088));
#1748=EDGE_LOOP('',(#9089,#9090,#9091,#9092));
#1749=EDGE_LOOP('',(#9093,#9094,#9095,#9096,#9097,#9098,#9099,#9100));
#1750=EDGE_LOOP('',(#9101,#9102,#9103,#9104,#9105,#9106,#9107,#9108,#9109,
#9110,#9111,#9112,#9113,#9114,#9115,#9116,#9117,#9118,#9119,#9120,#9121,
#9122,#9123,#9124,#9125,#9126));
#1751=EDGE_LOOP('',(#9127,#9128,#9129,#9130));
#1752=EDGE_LOOP('',(#9131,#9132,#9133,#9134,#9135,#9136,#9137,#9138,#9139,
#9140,#9141,#9142,#9143,#9144,#9145,#9146,#9147,#9148,#9149,#9150,#9151,
#9152,#9153,#9154,#9155,#9156,#9157));
#1753=EDGE_LOOP('',(#9158,#9159,#9160,#9161));
#1754=EDGE_LOOP('',(#9162,#9163,#9164,#9165));
#1755=EDGE_LOOP('',(#9166,#9167,#9168,#9169));
#1756=EDGE_LOOP('',(#9170,#9171,#9172,#9173));
#1757=EDGE_LOOP('',(#9174,#9175,#9176,#9177));
#1758=EDGE_LOOP('',(#9178,#9179,#9180,#9181));
#1759=EDGE_LOOP('',(#9182,#9183,#9184,#9185));
#1760=EDGE_LOOP('',(#9186,#9187,#9188,#9189,#9190,#9191));
#1761=EDGE_LOOP('',(#9192));
#1762=EDGE_LOOP('',(#9193,#9194,#9195,#9196));
#1763=EDGE_LOOP('',(#9197,#9198,#9199,#9200));
#1764=EDGE_LOOP('',(#9201));
#1765=EDGE_LOOP('',(#9202,#9203,#9204,#9205,#9206,#9207));
#1766=EDGE_LOOP('',(#9208));
#1767=EDGE_LOOP('',(#9209,#9210,#9211,#9212));
#1768=EDGE_LOOP('',(#9213,#9214,#9215,#9216));
#1769=EDGE_LOOP('',(#9217,#9218,#9219,#9220));
#1770=EDGE_LOOP('',(#9221,#9222,#9223,#9224));
#1771=EDGE_LOOP('',(#9225,#9226,#9227,#9228));
#1772=EDGE_LOOP('',(#9229,#9230,#9231,#9232));
#1773=EDGE_LOOP('',(#9233,#9234,#9235,#9236));
#1774=EDGE_LOOP('',(#9237,#9238,#9239,#9240));
#1775=EDGE_LOOP('',(#9241,#9242,#9243,#9244));
#1776=EDGE_LOOP('',(#9245,#9246,#9247,#9248));
#1777=EDGE_LOOP('',(#9249,#9250,#9251,#9252));
#1778=EDGE_LOOP('',(#9253,#9254,#9255,#9256));
#1779=EDGE_LOOP('',(#9257,#9258,#9259,#9260));
#1780=EDGE_LOOP('',(#9261,#9262,#9263,#9264));
#1781=EDGE_LOOP('',(#9265,#9266,#9267,#9268));
#1782=EDGE_LOOP('',(#9269,#9270,#9271,#9272));
#1783=EDGE_LOOP('',(#9273,#9274,#9275,#9276));
#1784=EDGE_LOOP('',(#9277,#9278,#9279,#9280));
#1785=EDGE_LOOP('',(#9281,#9282,#9283,#9284));
#1786=EDGE_LOOP('',(#9285,#9286,#9287,#9288,#9289,#9290,#9291,#9292,#9293,
#9294,#9295,#9296,#9297,#9298,#9299,#9300,#9301,#9302,#9303,#9304,#9305,
#9306,#9307));
#1787=EDGE_LOOP('',(#9308,#9309,#9310,#9311));
#1788=EDGE_LOOP('',(#9312,#9313,#9314,#9315,#9316,#9317,#9318,#9319,#9320,
#9321,#9322,#9323,#9324,#9325,#9326,#9327,#9328,#9329,#9330,#9331,#9332,
#9333,#9334));
#1789=EDGE_LOOP('',(#9335,#9336,#9337,#9338));
#1790=EDGE_LOOP('',(#9339));
#1791=EDGE_LOOP('',(#9340));
#1792=EDGE_LOOP('',(#9341));
#1793=EDGE_LOOP('',(#9342));
#1794=EDGE_LOOP('',(#9343,#9344,#9345,#9346));
#1795=EDGE_LOOP('',(#9347,#9348,#9349,#9350));
#1796=EDGE_LOOP('',(#9351));
#1797=EDGE_LOOP('',(#9352));
#1798=EDGE_LOOP('',(#9353));
#1799=EDGE_LOOP('',(#9354));
#1800=EDGE_LOOP('',(#9355,#9356,#9357,#9358));
#1801=EDGE_LOOP('',(#9359,#9360,#9361,#9362));
#1802=EDGE_LOOP('',(#9363));
#1803=EDGE_LOOP('',(#9364));
#1804=EDGE_LOOP('',(#9365));
#1805=EDGE_LOOP('',(#9366));
#1806=EDGE_LOOP('',(#9367,#9368,#9369,#9370));
#1807=EDGE_LOOP('',(#9371,#9372,#9373,#9374));
#1808=EDGE_LOOP('',(#9375,#9376,#9377,#9378));
#1809=EDGE_LOOP('',(#9379));
#1810=EDGE_LOOP('',(#9380));
#1811=EDGE_LOOP('',(#9381));
#1812=EDGE_LOOP('',(#9382,#9383,#9384,#9385));
#1813=EDGE_LOOP('',(#9386,#9387,#9388,#9389));
#1814=EDGE_LOOP('',(#9390));
#1815=EDGE_LOOP('',(#9391));
#1816=EDGE_LOOP('',(#9392,#9393,#9394,#9395));
#1817=EDGE_LOOP('',(#9396,#9397,#9398,#9399));
#1818=EDGE_LOOP('',(#9400));
#1819=EDGE_LOOP('',(#9401,#9402,#9403,#9404));
#1820=EDGE_LOOP('',(#9405,#9406,#9407,#9408));
#1821=EDGE_LOOP('',(#9409));
#1822=EDGE_LOOP('',(#9410));
#1823=EDGE_LOOP('',(#9411));
#1824=EDGE_LOOP('',(#9412));
#1825=CIRCLE('',#10507,1.666);
#1826=CIRCLE('',#10508,1.666);
#1827=CIRCLE('',#10523,1.666);
#1828=CIRCLE('',#10525,2.05475000000001);
#1829=CIRCLE('',#10541,2.05475000000001);
#1830=CIRCLE('',#10543,1.666);
#1831=CIRCLE('',#10544,1.666);
#1832=CIRCLE('',#10559,1.666);
#1833=CIRCLE('',#10561,2.05475);
#1834=CIRCLE('',#10577,2.05475);
#1835=CIRCLE('',#10579,1.666);
#1836=CIRCLE('',#10580,1.666);
#1837=CIRCLE('',#10595,1.666);
#1838=CIRCLE('',#10597,2.05475000000001);
#1839=CIRCLE('',#10613,2.05475000000001);
#1840=CIRCLE('',#10615,1.666);
#1841=CIRCLE('',#10616,1.666);
#1842=CIRCLE('',#10631,1.666);
#1843=CIRCLE('',#10633,2.05475);
#1844=CIRCLE('',#10649,2.05475);
#1845=CIRCLE('',#10651,2.5175);
#1846=CIRCLE('',#10652,2.5175);
#1847=CIRCLE('',#10667,2.5175);
#1848=CIRCLE('',#10669,2.5175);
#1849=CIRCLE('',#10670,2.5175);
#1850=CIRCLE('',#10685,2.5175);
#1851=CIRCLE('',#10687,3.0735);
#1852=CIRCLE('',#10702,3.0735);
#1853=CIRCLE('',#10704,3.0735);
#1854=CIRCLE('',#10719,3.0735);
#1855=CIRCLE('',#10721,2.5175);
#1856=CIRCLE('',#10722,2.5175);
#1857=CIRCLE('',#10723,2.5175);
#1858=CIRCLE('',#10738,2.5175);
#1859=CIRCLE('',#10740,3.0735);
#1860=CIRCLE('',#10755,3.0735);
#1861=CIRCLE('',#10757,2.5175);
#1862=CIRCLE('',#10758,2.5175);
#1863=CIRCLE('',#10759,2.5175);
#1864=CIRCLE('',#10774,2.5175);
#1865=CIRCLE('',#10776,3.0735);
#1866=CIRCLE('',#10791,3.0735);
#1867=CIRCLE('',#10793,7.263);
#1868=CIRCLE('',#10801,7.263);
#1869=CIRCLE('',#10803,8.1015);
#1870=CIRCLE('',#10811,8.1015);
#1871=CIRCLE('',#10814,12.);
#1872=CIRCLE('',#10817,12.);
#1873=CIRCLE('',#10827,2.5175);
#1874=CIRCLE('',#10833,2.5175);
#1875=CIRCLE('',#10858,5.);
#1876=CIRCLE('',#10859,5.);
#1877=CIRCLE('',#10861,5.);
#1878=CIRCLE('',#10862,5.);
#1879=CIRCLE('',#10864,5.);
#1880=CIRCLE('',#10865,5.);
#1881=CIRCLE('',#10867,5.);
#1882=CIRCLE('',#10868,5.);
#1883=CIRCLE('',#10870,5.);
#1884=CIRCLE('',#10871,5.);
#1885=CIRCLE('',#10873,5.);
#1886=CIRCLE('',#10874,5.);
#1887=CIRCLE('',#10876,5.);
#1888=CIRCLE('',#10877,5.);
#1889=CIRCLE('',#10879,5.);
#1890=CIRCLE('',#10880,5.);
#1891=CIRCLE('',#10882,5.);
#1892=CIRCLE('',#10883,5.);
#1893=CIRCLE('',#10885,5.);
#1894=CIRCLE('',#10886,5.);
#1895=CIRCLE('',#10888,5.);
#1896=CIRCLE('',#10889,5.);
#1897=CIRCLE('',#10891,5.);
#1898=CIRCLE('',#10892,5.);
#1899=CIRCLE('',#10894,5.);
#1900=CIRCLE('',#10895,5.);
#1901=CIRCLE('',#10897,5.);
#1902=CIRCLE('',#10898,5.);
#1903=CIRCLE('',#10900,5.);
#1904=CIRCLE('',#10901,5.);
#1905=CIRCLE('',#10903,5.);
#1906=CIRCLE('',#10904,5.);
#1907=CIRCLE('',#10906,5.);
#1908=CIRCLE('',#10907,5.);
#1909=CIRCLE('',#10909,5.);
#1910=CIRCLE('',#10910,5.);
#1911=CIRCLE('',#10923,2.5);
#1912=CIRCLE('',#10924,2.5);
#1913=CIRCLE('',#10926,2.5);
#1914=CIRCLE('',#10927,2.5);
#1915=CIRCLE('',#10929,2.5);
#1916=CIRCLE('',#10930,2.5);
#1917=CIRCLE('',#10932,2.5);
#1918=CIRCLE('',#10933,2.5);
#1919=CIRCLE('',#10942,2.5);
#1920=CIRCLE('',#10943,2.5);
#1921=CIRCLE('',#10945,2.5);
#1922=CIRCLE('',#10946,2.5);
#1923=CIRCLE('',#10948,2.5);
#1924=CIRCLE('',#10949,2.5);
#1925=CIRCLE('',#10951,2.5);
#1926=CIRCLE('',#10952,2.5);
#1927=CIRCLE('',#10965,4.);
#1928=CIRCLE('',#10966,4.);
#1929=CIRCLE('',#10968,5.);
#1930=CIRCLE('',#10969,5.);
#1931=CIRCLE('',#10974,5.);
#1932=CIRCLE('',#10975,5.);
#1933=CIRCLE('',#10977,5.);
#1934=CIRCLE('',#10978,5.);
#1935=CIRCLE('',#10980,5.);
#1936=CIRCLE('',#10981,5.);
#1937=CIRCLE('',#10983,5.);
#1938=CIRCLE('',#10984,5.);
#1939=CIRCLE('',#10986,5.);
#1940=CIRCLE('',#10987,5.);
#1941=CIRCLE('',#10989,5.);
#1942=CIRCLE('',#10990,5.);
#1943=CIRCLE('',#10992,5.);
#1944=CIRCLE('',#10993,5.);
#1945=CIRCLE('',#10995,5.);
#1946=CIRCLE('',#10996,5.);
#1947=CIRCLE('',#10998,5.);
#1948=CIRCLE('',#10999,5.);
#1949=CIRCLE('',#11001,5.);
#1950=CIRCLE('',#11002,5.);
#1951=CIRCLE('',#11004,5.);
#1952=CIRCLE('',#11005,5.);
#1953=CIRCLE('',#11007,5.);
#1954=CIRCLE('',#11008,5.);
#1955=CIRCLE('',#11010,5.);
#1956=CIRCLE('',#11011,5.);
#1957=CIRCLE('',#11013,5.);
#1958=CIRCLE('',#11014,5.);
#1959=CIRCLE('',#11016,5.);
#1960=CIRCLE('',#11017,5.);
#1961=CIRCLE('',#11019,5.);
#1962=CIRCLE('',#11020,5.);
#1963=CIRCLE('',#11022,5.);
#1964=CIRCLE('',#11023,5.);
#1965=CIRCLE('',#11025,5.);
#1966=CIRCLE('',#11026,5.);
#1967=CIRCLE('',#11035,13.);
#1968=CIRCLE('',#11036,13.);
#1969=CIRCLE('',#11038,4.5);
#1970=CIRCLE('',#11039,4.5);
#1971=CIRCLE('',#11041,4.5);
#1972=CIRCLE('',#11042,4.5);
#1973=CIRCLE('',#11044,3.5);
#1974=CIRCLE('',#11045,3.5);
#1975=CIRCLE('',#11047,3.5);
#1976=CIRCLE('',#11048,3.5);
#1977=CIRCLE('',#11050,3.5);
#1978=CIRCLE('',#11051,3.5);
#1979=CIRCLE('',#11053,3.5);
#1980=CIRCLE('',#11054,3.5);
#1981=CIRCLE('',#11063,1.954);
#1982=CIRCLE('',#11080,1.5555);
#1983=CIRCLE('',#11097,1.954);
#1984=CIRCLE('',#11098,1.);
#1985=CIRCLE('',#11100,1.5555);
#1986=CIRCLE('',#11110,3.5);
#1987=CIRCLE('',#11112,3.5);
#1988=CIRCLE('',#11117,2.942);
#1989=CIRCLE('',#11129,2.37175);
#1990=CIRCLE('',#11141,2.942);
#1991=CIRCLE('',#11142,2.);
#1992=CIRCLE('',#11144,2.37175);
#1993=CIRCLE('',#11154,5.);
#1994=CIRCLE('',#11156,5.);
#1995=CIRCLE('',#11161,7.925);
#1996=CIRCLE('',#11172,7.0685);
#1997=CIRCLE('',#11182,7.0685);
#1998=CIRCLE('',#11184,7.925);
#1999=CIRCLE('',#11186,7.);
#2000=CIRCLE('',#11187,6.);
#2001=CIRCLE('',#11189,7.);
#2002=CIRCLE('',#11190,6.);
#2003=CIRCLE('',#11193,6.);
#2004=CIRCLE('',#11195,7.);
#2005=CIRCLE('',#11197,7.);
#2006=CIRCLE('',#11198,6.);
#2007=CIRCLE('',#11201,6.);
#2008=CIRCLE('',#11203,7.);
#2009=CIRCLE('',#11205,7.);
#2010=CIRCLE('',#11206,6.);
#2011=CIRCLE('',#11209,6.);
#2012=CIRCLE('',#11211,6.);
#2013=CIRCLE('',#11213,4.);
#2014=CIRCLE('',#11215,12.);
#2015=CIRCLE('',#11217,12.);
#2016=CIRCLE('',#11220,4.);
#2017=CIRCLE('',#11224,8.5);
#2018=CIRCLE('',#11225,8.5);
#2019=CIRCLE('',#11227,12.);
#2020=CIRCLE('',#11228,12.);
#2021=B_SPLINE_CURVE_WITH_KNOTS('',3,(#13455,#13456,#13457,#13458,#13459,
#13460,#13461,#13462,#13463,#13464,#13465,#13466,#13467,#13468,#13469,#13470,
#13471,#13472,#13473),.UNSPECIFIED.,.F.,.F.,(4,3,3,3,3,3,4),(95.5576018628658,
95.7627393059135,96.7602678403502,97.7577963747867,98.7553249092233,99.75285344366,
100.750381978097),.UNSPECIFIED.);
#2022=B_SPLINE_CURVE_WITH_KNOTS('',3,(#13477,#13478,#13479,#13480),
 .UNSPECIFIED.,.F.,.F.,(4,4),(-98.735769112822,-98.0941628713862),
 .UNSPECIFIED.);
#2023=B_SPLINE_CURVE_WITH_KNOTS('',3,(#13484,#13485,#13486,#13487,#13488,
#13489,#13490,#13491,#13492,#13493,#13494,#13495,#13496,#13497,#13498,#13499,
#13500,#13501,#13502,#13503,#13504,#13505),.UNSPECIFIED.,.F.,.F.,(4,3,3,
3,3,3,3,4),(-98.0941628713862,-97.7577963747868,-96.7602678403502,-95.7627393059136,
-94.765210771477,-93.7676822370404,-92.7701537026038,-91.8109775642066),
 .UNSPECIFIED.);
#2024=B_SPLINE_CURVE_WITH_KNOTS('',3,(#13510,#13511,#13512,#13513,#13514,
#13515,#13516,#13517,#13518,#13519,#13520,#13521,#13522,#13523,#13524,#13525,
#13526,#13527,#13528,#13529,#13530,#13531),.UNSPECIFIED.,.F.,.F.,(4,3,3,
3,3,3,3,4),(89.2744165556862,89.777568099294,90.7750966337306,91.7726251681672,
92.7701537026037,93.7676822370404,94.7652107714769,95.5576018628658),
 .UNSPECIFIED.);
#2025=B_SPLINE_CURVE_WITH_KNOTS('',3,(#13532,#13533,#13534,#13535,#13536,
#13537,#13538,#13539,#13540,#13541,#13542,#13543,#13544,#13545,#13546,#13547,
#13548,#13549,#13550,#13551,#13552,#13553,#13554,#13555,#13556),
 .UNSPECIFIED.,.F.,.F.,(4,3,3,3,3,3,3,3,4),(-91.8109775642066,-91.7726251681672,
-90.7750966337306,-89.777568099294,-88.7800395648574,-87.7825110304208,
-86.7849824959842,-85.7874539615476,-85.527792257027),.UNSPECIFIED.);
#2026=B_SPLINE_CURVE_WITH_KNOTS('',3,(#13561,#13562,#13563,#13564,#13565,
#13566,#13567,#13568,#13569,#13570,#13571,#13572,#13573,#13574,#13575,#13576,
#13577,#13578,#13579,#13580,#13581,#13582),.UNSPECIFIED.,.F.,.F.,(4,3,3,
3,3,3,3,4),(82.9912312485066,83.7923968926744,84.789925427111,85.7874539615476,
86.7849824959842,87.7825110304208,88.7800395648573,89.2744165556862),
 .UNSPECIFIED.);
#2027=B_SPLINE_CURVE_WITH_KNOTS('',3,(#13583,#13584,#13585,#13586,#13587,
#13588,#13589,#13590,#13591,#13592,#13593,#13594,#13595,#13596,#13597,#13598,
#13599,#13600,#13601,#13602,#13603,#13604),.UNSPECIFIED.,.F.,.F.,(4,3,3,
3,3,3,3,4),(-85.527792257027,-84.789925427111,-83.7923968926744,-82.7948683582378,
-81.7973398238012,-80.7998112893646,-79.802282754928,-79.2446069498474),
 .UNSPECIFIED.);
#2028=B_SPLINE_CURVE_WITH_KNOTS('',3,(#13609,#13610,#13611,#13612,#13613,
#13614,#13615,#13616,#13617,#13618,#13619,#13620,#13621,#13622,#13623,#13624,
#13625,#13626,#13627,#13628,#13629,#13630,#13631,#13632,#13633),
 .UNSPECIFIED.,.F.,.F.,(4,3,3,3,3,3,3,3,4),(76.7080459413271,76.8096971516182,
77.8072256860548,78.8047542204914,79.802282754928,80.7998112893646,81.7973398238012,
82.7948683582378,82.9912312485066),.UNSPECIFIED.);
#2029=B_SPLINE_CURVE_WITH_KNOTS('',3,(#13634,#13635,#13636,#13637,#13638,
#13639,#13640,#13641,#13642,#13643,#13644,#13645,#13646,#13647,#13648,#13649,
#13650,#13651,#13652,#13653,#13654,#13655),.UNSPECIFIED.,.F.,.F.,(4,3,3,
3,3,3,3,4),(-79.2446069498474,-78.8047542204914,-77.8072256860548,-76.8096971516182,
-75.8121686171816,-74.814640082745,-73.8171115483084,-72.9614216426678),
 .UNSPECIFIED.);
#2030=B_SPLINE_CURVE_WITH_KNOTS('',3,(#13660,#13661,#13662,#13663,#13664,
#13665,#13666,#13667,#13668,#13669,#13670,#13671,#13672,#13673,#13674,#13675,
#13676,#13677,#13678,#13679,#13680,#13681),.UNSPECIFIED.,.F.,.F.,(4,3,3,
3,3,3,3,4),(70.4248606341475,70.8245259449986,71.8220544794352,72.8195830138718,
73.8171115483084,74.814640082745,75.8121686171816,76.7080459413271),
 .UNSPECIFIED.);
#2031=B_SPLINE_CURVE_WITH_KNOTS('',3,(#13682,#13683,#13684,#13685,#13686,
#13687,#13688,#13689,#13690,#13691,#13692,#13693,#13694,#13695,#13696,#13697,
#13698,#13699,#13700,#13701,#13702,#13703,#13704,#13705,#13706),
 .UNSPECIFIED.,.F.,.F.,(4,3,3,3,3,3,3,3,4),(-72.9614216426678,-72.8195830138718,
-71.8220544794352,-70.8245259449986,-69.826997410562,-68.8294688761254,
-67.8319403416888,-66.8344118072522,-66.6782363354882),.UNSPECIFIED.);
#2032=B_SPLINE_CURVE_WITH_KNOTS('',3,(#13711,#13712,#13713,#13714,#13715,
#13716,#13717,#13718,#13719,#13720,#13721,#13722,#13723,#13724,#13725,#13726,
#13727,#13728,#13729,#13730,#13731,#13732),.UNSPECIFIED.,.F.,.F.,(4,3,3,
3,3,3,3,4),(64.1416753269678,64.839354738379,65.8368832728156,66.8344118072522,
67.8319403416888,68.8294688761254,69.826997410562,70.4248606341475),
 .UNSPECIFIED.);
#2033=B_SPLINE_CURVE_WITH_KNOTS('',3,(#13733,#13734,#13735,#13736,#13737,
#13738,#13739,#13740,#13741,#13742,#13743,#13744,#13745,#13746,#13747,#13748,
#13749,#13750,#13751,#13752,#13753,#13754),.UNSPECIFIED.,.F.,.F.,(4,3,3,
3,3,3,3,4),(-66.6782363354882,-65.8368832728156,-64.839354738379,-63.8418262039424,
-62.8442976695058,-61.8467691350692,-60.8492406006326,-60.3950510283086),
 .UNSPECIFIED.);
#2034=B_SPLINE_CURVE_WITH_KNOTS('',3,(#13759,#13760,#13761,#13762,#13763,
#13764,#13765,#13766,#13767,#13768,#13769,#13770,#13771,#13772,#13773,#13774,
#13775,#13776,#13777,#13778,#13779,#13780),.UNSPECIFIED.,.F.,.F.,(4,3,3,
3,3,3,3,4),(57.8584900197883,58.8541835317594,59.851712066196,60.8492406006326,
61.8467691350692,62.8442976695058,63.8418262039424,64.1416753269678),
 .UNSPECIFIED.);
#2035=B_SPLINE_CURVE_WITH_KNOTS('',3,(#13781,#13782,#13783,#13784,#13785,
#13786,#13787,#13788,#13789,#13790,#13791,#13792,#13793,#13794,#13795,#13796,
#13797,#13798,#13799,#13800,#13801,#13802),.UNSPECIFIED.,.F.,.F.,(4,3,3,
3,3,3,3,4),(-60.3950510283086,-59.851712066196,-58.8541835317594,-57.8566549973228,
-56.8591264628862,-55.8615979284496,-54.864069394013,-54.111865721129),
 .UNSPECIFIED.);
#2036=B_SPLINE_CURVE_WITH_KNOTS('',3,(#13807,#13808,#13809,#13810,#13811,
#13812,#13813,#13814,#13815,#13816,#13817,#13818,#13819,#13820,#13821,#13822,
#13823,#13824,#13825,#13826,#13827,#13828),.UNSPECIFIED.,.F.,.F.,(4,3,3,
3,3,3,3,4),(51.5753047126087,51.8714837907032,52.8690123251398,53.8665408595764,
54.864069394013,55.8615979284496,56.8591264628862,57.8584900197883),
 .UNSPECIFIED.);
#2037=B_SPLINE_CURVE_WITH_KNOTS('',3,(#13829,#13830,#13831,#13832,#13833,
#13834,#13835,#13836,#13837,#13838,#13839,#13840,#13841,#13842,#13843,#13844,
#13845,#13846,#13847,#13848,#13849,#13850,#13851,#13852,#13853),
 .UNSPECIFIED.,.F.,.F.,(4,3,3,3,3,3,3,3,4),(-54.111865721129,-53.8665408595764,
-52.8690123251398,-51.8714837907032,-50.8739552562666,-49.87642672183,-48.8788981873934,
-47.8813696529568,-47.8286804139494),.UNSPECIFIED.);
#2038=B_SPLINE_CURVE_WITH_KNOTS('',3,(#13858,#13859,#13860,#13861,#13862,
#13863,#13864,#13865,#13866,#13867,#13868,#13869,#13870,#13871,#13872,#13873,
#13874,#13875,#13876,#13877,#13878,#13879),.UNSPECIFIED.,.F.,.F.,(4,3,3,
3,3,3,3,4),(45.2921194054291,45.8863125840836,46.8838411185202,47.8813696529568,
48.8788981873934,49.87642672183,50.8739552562666,51.5753047126087),
 .UNSPECIFIED.);
#2039=B_SPLINE_CURVE_WITH_KNOTS('',3,(#13880,#13881,#13882,#13883,#13884,
#13885,#13886,#13887,#13888,#13889,#13890,#13891,#13892,#13893,#13894,#13895,
#13896,#13897,#13898,#13899,#13900,#13901),.UNSPECIFIED.,.F.,.F.,(4,3,3,
3,3,3,3,4),(-47.8286804139494,-46.8838411185202,-45.8863125840836,-44.888784049647,
-43.8912555152104,-42.8937269807738,-41.8961984463372,-41.5454951067698),
 .UNSPECIFIED.);
#2040=B_SPLINE_CURVE_WITH_KNOTS('',3,(#13906,#13907,#13908,#13909,#13910,
#13911,#13912,#13913,#13914,#13915,#13916,#13917,#13918,#13919,#13920,#13921,
#13922,#13923,#13924,#13925,#13926,#13927),.UNSPECIFIED.,.F.,.F.,(4,3,3,
3,3,3,3,4),(39.0089340982495,39.901141377464,40.8986699119006,41.8961984463372,
42.8937269807738,43.8912555152104,44.888784049647,45.2921194054291),
 .UNSPECIFIED.);
#2041=B_SPLINE_CURVE_WITH_KNOTS('',3,(#13928,#13929,#13930,#13931,#13932,
#13933,#13934,#13935,#13936,#13937,#13938,#13939,#13940,#13941,#13942,#13943,
#13944,#13945,#13946,#13947,#13948,#13949),.UNSPECIFIED.,.F.,.F.,(4,3,3,
3,3,3,3,4),(-41.5454951067698,-40.8986699119006,-39.901141377464,-38.9036128430274,
-37.9060843085908,-36.9085557741542,-35.9110272397176,-35.2623097995902),
 .UNSPECIFIED.);
#2042=B_SPLINE_CURVE_WITH_KNOTS('',3,(#13954,#13955,#13956,#13957,#13958,
#13959,#13960,#13961,#13962,#13963,#13964,#13965,#13966,#13967,#13968,#13969,
#13970,#13971,#13972,#13973,#13974,#13975,#13976,#13977,#13978),
 .UNSPECIFIED.,.F.,.F.,(4,3,3,3,3,3,3,3,4),(32.7257487910699,32.9184416364078,
33.9159701708444,34.913498705281,35.9110272397176,36.9085557741542,37.9060843085908,
38.9036128430274,39.0089340982495),.UNSPECIFIED.);
#2043=B_SPLINE_CURVE_WITH_KNOTS('',3,(#13979,#13980,#13981,#13982,#13983,
#13984,#13985,#13986,#13987,#13988,#13989,#13990,#13991,#13992,#13993,#13994,
#13995,#13996,#13997,#13998,#13999,#14000),.UNSPECIFIED.,.F.,.F.,(4,3,3,
3,3,3,3,4),(-35.2623097995902,-34.913498705281,-33.9159701708444,-32.9184416364078,
-31.9209131019712,-30.9233845675346,-29.925856033098,-28.9791244924106),
 .UNSPECIFIED.);
#2044=B_SPLINE_CURVE_WITH_KNOTS('',3,(#14005,#14006,#14007,#14008,#14009,
#14010,#14011,#14012,#14013,#14014,#14015,#14016,#14017,#14018,#14019,#14020,
#14021,#14022,#14023,#14024,#14025,#14026),.UNSPECIFIED.,.F.,.F.,(4,3,3,
3,3,3,3,4),(26.4425634838903,26.9332704297882,27.9307989642248,28.9283274986614,
29.925856033098,30.9233845675346,31.9209131019712,32.7257487910699),
 .UNSPECIFIED.);
#2045=B_SPLINE_CURVE_WITH_KNOTS('',3,(#14027,#14028,#14029,#14030,#14031,
#14032,#14033,#14034,#14035,#14036,#14037,#14038,#14039,#14040,#14041,#14042,
#14043,#14044,#14045,#14046,#14047,#14048,#14049,#14050,#14051),
 .UNSPECIFIED.,.F.,.F.,(4,3,3,3,3,3,3,3,4),(-28.9791244924106,-28.9283274986614,
-27.9307989642248,-26.9332704297882,-25.9357418953516,-24.938213360915,
-23.9406848264784,-22.9431562920418,-22.6959391852311),.UNSPECIFIED.);
#2046=B_SPLINE_CURVE_WITH_KNOTS('',3,(#14056,#14057,#14058,#14059,#14060,
#14061,#14062,#14063,#14064,#14065,#14066,#14067,#14068,#14069,#14070,#14071,
#14072,#14073,#14074,#14075,#14076,#14077),.UNSPECIFIED.,.F.,.F.,(4,3,3,
3,3,3,3,4),(20.1593781767107,20.9480992231686,21.9456277576052,22.9431562920418,
23.9406848264784,24.938213360915,25.9357418953516,26.4425634838903),
 .UNSPECIFIED.);
#2047=B_SPLINE_CURVE_WITH_KNOTS('',3,(#14078,#14079,#14080,#14081,#14082,
#14083,#14084,#14085,#14086,#14087,#14088,#14089,#14090,#14091,#14092,#14093,
#14094,#14095,#14096,#14097,#14098,#14099),.UNSPECIFIED.,.F.,.F.,(4,3,3,
3,3,3,3,4),(-22.6959391852311,-21.9456277576052,-20.9480992231686,-19.950570688732,
-18.9530421542954,-17.9555136198588,-16.9579850854222,-16.4127538780515),
 .UNSPECIFIED.);
#2048=B_SPLINE_CURVE_WITH_KNOTS('',3,(#14104,#14105,#14106,#14107,#14108,
#14109,#14110,#14111,#14112,#14113,#14114,#14115,#14116,#14117,#14118,#14119,
#14120,#14121,#14122,#14123,#14124,#14125,#14126,#14127,#14128),
 .UNSPECIFIED.,.F.,.F.,(4,3,3,3,3,3,3,3,4),(13.8761928695311,13.9653994821124,
14.962928016549,15.9604565509856,16.9579850854222,17.9555136198588,18.9530421542954,
19.950570688732,20.1593781767107),.UNSPECIFIED.);
#2049=B_SPLINE_CURVE_WITH_KNOTS('',3,(#14129,#14130,#14131,#14132,#14133,
#14134,#14135,#14136,#14137,#14138,#14139,#14140,#14141,#14142,#14143,#14144,
#14145,#14146,#14147,#14148,#14149,#14150),.UNSPECIFIED.,.F.,.F.,(4,3,3,
3,3,3,3,4),(-16.4127538780515,-15.9604565509856,-14.962928016549,-13.9653994821124,
-12.9678709476758,-11.9703424132392,-10.9728138788026,-10.1295685708719),
 .UNSPECIFIED.);
#2050=B_SPLINE_CURVE_WITH_KNOTS('',3,(#14156,#14157,#14158,#14159,#14160,
#14161,#14162,#14163,#14164,#14165,#14166,#14167,#14168),.UNSPECIFIED.,
 .F.,.F.,(4,3,3,3,4),(-3.8463832636923,-2.9925856033098,-1.9950570688732,
-0.997528534436598,0.),.UNSPECIFIED.);
#2051=B_SPLINE_CURVE_WITH_KNOTS('',3,(#14171,#14172,#14173,#14174,#14175,
#14176,#14177,#14178,#14179,#14180,#14181,#14182,#14183,#14184,#14185,#14186,
#14187,#14188,#14189),.UNSPECIFIED.,.F.,.F.,(4,3,3,3,3,3,4),(2.01461286527445,
2.9925856033098,3.9901141377464,4.987642672183,5.9851712066196,6.9826997410562,
7.59300756235153),.UNSPECIFIED.);
#2052=B_SPLINE_CURVE_WITH_KNOTS('',3,(#14195,#14196,#14197,#14198,#14199,
#14200),.UNSPECIFIED.,.F.,.F.,(4,1,1,4),(109.955742875643,110.61690491348,
111.614433447917,112.611961982353),.UNSPECIFIED.);
#2053=B_SPLINE_CURVE_WITH_KNOTS('',3,(#14203,#14204,#14205,#14206,#14207,
#14208,#14209),.UNSPECIFIED.,.F.,.F.,(4,1,1,1,4),(109.955742875643,110.16088031869,
111.158408853127,112.155937387564,113.133910125599),.UNSPECIFIED.);
#2054=B_SPLINE_CURVE_WITH_KNOTS('',3,(#14214,#14215,#14216,#14217,#14218,
#14219,#14220,#14221,#14222,#14223),.UNSPECIFIED.,.F.,.F.,(4,1,1,1,1,1,
1,4),(103.672557568463,104.63173370686,105.629262241297,106.626790775734,
107.62431931017,108.621847844607,109.619376379043,109.955742875643),
 .UNSPECIFIED.);
#2055=B_SPLINE_CURVE_WITH_KNOTS('',3,(#14224,#14225,#14226,#14227,#14228,
#14229,#14230,#14231,#14232,#14233),.UNSPECIFIED.,.F.,.F.,(4,1,1,1,1,1,
1,4),(103.672557568463,104.175709112071,105.173237646507,106.170766180944,
107.168294715381,108.165823249817,109.163351784254,109.955742875643),
 .UNSPECIFIED.);
#2056=B_SPLINE_CURVE_WITH_KNOTS('',3,(#14238,#14239,#14240,#14241,#14242,
#14243,#14244,#14245,#14246,#14247,#14248),.UNSPECIFIED.,.F.,.F.,(4,1,1,
1,1,1,1,1,4),(97.3893722612836,97.6490339658042,98.6465625002408,99.6440910346774,
100.641619569114,101.639148103551,102.636676637987,103.634205172424,103.672557568463),
 .UNSPECIFIED.);
#2057=B_SPLINE_CURVE_WITH_KNOTS('',3,(#14249,#14250,#14251,#14252,#14253,
#14254,#14255,#14256,#14257,#14258),.UNSPECIFIED.,.F.,.F.,(4,1,1,1,1,1,
1,4),(97.3893722612836,98.1905379054512,99.1880664398878,100.185594974324,
101.183123508761,102.180652043198,103.178180577634,103.672557568463),
 .UNSPECIFIED.);
#2058=B_SPLINE_CURVE_WITH_KNOTS('',3,(#14263,#14264,#14265,#14266,#14267,
#14268,#14269,#14270,#14271,#14272),.UNSPECIFIED.,.F.,.F.,(4,1,1,1,1,1,
1,4),(91.106186954104,91.6638627591846,92.6613912936212,93.6589198280578,
94.6564483624944,95.653976896931,96.6515054313676,97.3893722612836),
 .UNSPECIFIED.);
#2059=B_SPLINE_CURVE_WITH_KNOTS('',3,(#14273,#14274,#14275,#14276,#14277,
#14278,#14279,#14280,#14281,#14282,#14283),.UNSPECIFIED.,.F.,.F.,(4,1,1,
1,1,1,1,1,4),(91.106186954104,91.207838164395,92.2053666988316,93.2028952332682,
94.2004237677048,95.1979523021414,96.195480836578,97.1930093710146,97.3893722612836),
 .UNSPECIFIED.);
#2060=B_SPLINE_CURVE_WITH_KNOTS('',3,(#14288,#14289,#14290,#14291,#14292,
#14293,#14294,#14295,#14296,#14297),.UNSPECIFIED.,.F.,.F.,(4,1,1,1,1,1,
1,4),(84.8230016469244,85.678691552565,86.6762200870016,87.6737486214382,
88.6712771558748,89.6688056903114,90.666334224748,91.106186954104),
 .UNSPECIFIED.);
#2061=B_SPLINE_CURVE_WITH_KNOTS('',3,(#14298,#14299,#14300,#14301,#14302,
#14303,#14304,#14305,#14306,#14307),.UNSPECIFIED.,.F.,.F.,(4,1,1,1,1,1,
1,4),(84.8230016469244,85.2226669577754,86.220195492212,87.2177240266486,
88.2152525610852,89.2127810955218,90.2103096299584,91.106186954104),
 .UNSPECIFIED.);
#2062=B_SPLINE_CURVE_WITH_KNOTS('',3,(#14312,#14313,#14314,#14315,#14316,
#14317,#14318,#14319,#14320,#14321,#14322),.UNSPECIFIED.,.F.,.F.,(4,1,1,
1,1,1,1,1,4),(78.5398163397448,78.6959918115088,79.6935203459454,80.691048880382,
81.6885774148186,82.6861059492552,83.6836344836918,84.6811630181284,84.8230016469244),
 .UNSPECIFIED.);
#2063=B_SPLINE_CURVE_WITH_KNOTS('',3,(#14323,#14324,#14325,#14326,#14327,
#14328,#14329,#14330,#14331,#14332),.UNSPECIFIED.,.F.,.F.,(4,1,1,1,1,1,
1,4),(78.5398163397448,79.2374957511558,80.2350242855924,81.232552820029,
82.2300813544656,83.2276098889022,84.2251384233388,84.8230016469244),
 .UNSPECIFIED.);
#2064=B_SPLINE_CURVE_WITH_KNOTS('',3,(#14337,#14338,#14339,#14340,#14341,
#14342,#14343,#14344,#14345,#14346),.UNSPECIFIED.,.F.,.F.,(4,1,1,1,1,1,
1,4),(72.2566310325652,72.7108206048892,73.7083491393258,74.7058776737624,
75.703406208199,76.7009347426356,77.6984632770722,78.5398163397448),
 .UNSPECIFIED.);
#2065=B_SPLINE_CURVE_WITH_KNOTS('',3,(#14347,#14348,#14349,#14350,#14351,
#14352,#14353,#14354,#14355,#14356),.UNSPECIFIED.,.F.,.F.,(4,1,1,1,1,1,
1,4),(72.2566310325652,73.2523245445362,74.2498530789728,75.2473816134094,
76.244910147846,77.2424386822826,78.2399672167192,78.5398163397448),
 .UNSPECIFIED.);
#2066=B_SPLINE_CURVE_WITH_KNOTS('',3,(#14361,#14362,#14363,#14364,#14365,
#14366,#14367,#14368,#14369,#14370),.UNSPECIFIED.,.F.,.F.,(4,1,1,1,1,1,
1,4),(65.9734457253856,66.7256493982696,67.7231779327062,68.7207064671428,
69.7182350015794,70.715763536016,71.7132920704526,72.2566310325652),
 .UNSPECIFIED.);
#2067=B_SPLINE_CURVE_WITH_KNOTS('',3,(#14371,#14372,#14373,#14374,#14375,
#14376,#14377,#14378,#14379,#14380,#14381),.UNSPECIFIED.,.F.,.F.,(4,1,1,
1,1,1,1,1,4),(65.9734457253856,66.26962480348,67.2671533379166,68.2646818723533,
69.2622104067898,70.2597389412264,71.257267475663,72.2547960100996,72.2566310325652),
 .UNSPECIFIED.);
#2068=B_SPLINE_CURVE_WITH_KNOTS('',3,(#14386,#14387,#14388,#14389,#14390,
#14391,#14392,#14393,#14394,#14395,#14396),.UNSPECIFIED.,.F.,.F.,(4,1,1,
1,1,1,1,1,4),(59.690260418206,59.7429496572134,60.74047819165,61.7380067260866,
62.7355352605232,63.7330637949598,64.7305923293964,65.728120863833,65.9734457253856),
 .UNSPECIFIED.);
#2069=B_SPLINE_CURVE_WITH_KNOTS('',3,(#14397,#14398,#14399,#14400,#14401,
#14402,#14403,#14404,#14405,#14406),.UNSPECIFIED.,.F.,.F.,(4,1,1,1,1,1,
1,4),(59.690260418206,60.2844535968604,61.281982131297,62.2795106657336,
63.2770392001703,64.2745677346068,65.2720962690434,65.9734457253856),
 .UNSPECIFIED.);
#2070=B_SPLINE_CURVE_WITH_KNOTS('',3,(#14411,#14412,#14413,#14414,#14415,
#14416,#14417,#14418,#14419,#14420),.UNSPECIFIED.,.F.,.F.,(4,1,1,1,1,1,
1,4),(53.4070751110264,53.7577784505938,54.7553069850304,55.752835519467,
56.7503640539036,57.7478925883402,58.7454211227768,59.690260418206),
 .UNSPECIFIED.);
#2071=B_SPLINE_CURVE_WITH_KNOTS('',3,(#14421,#14422,#14423,#14424,#14425,
#14426,#14427,#14428,#14429,#14430),.UNSPECIFIED.,.F.,.F.,(4,1,1,1,1,1,
1,4),(53.4070751110264,54.2992823902408,55.2968109246774,56.294339459114,
57.2918679935507,58.2893965279873,59.2869250624238,59.690260418206),
 .UNSPECIFIED.);
#2072=B_SPLINE_CURVE_WITH_KNOTS('',3,(#14435,#14436,#14437,#14438,#14439,
#14440,#14441,#14442,#14443,#14444),.UNSPECIFIED.,.F.,.F.,(4,1,1,1,1,1,
1,4),(47.1238898038469,47.7726072439742,48.7701357784108,49.7676643128474,
50.765192847284,51.7627213817206,52.7602499161572,53.4070751110264),
 .UNSPECIFIED.);
#2073=B_SPLINE_CURVE_WITH_KNOTS('',3,(#14445,#14446,#14447,#14448,#14449,
#14450,#14451,#14452,#14453,#14454,#14455),.UNSPECIFIED.,.F.,.F.,(4,1,1,
1,1,1,1,1,4),(47.1238898038469,47.3165826491847,48.3141111836213,49.3116397180578,
50.3091682524944,51.3066967869311,52.3042253213677,53.3017538558043,53.4070751110264),
 .UNSPECIFIED.);
#2074=B_SPLINE_CURVE_WITH_KNOTS('',3,(#14460,#14461,#14462,#14463,#14464,
#14465,#14466,#14467,#14468,#14469),.UNSPECIFIED.,.F.,.F.,(4,1,1,1,1,1,
1,4),(40.8407044966673,41.7874360373546,42.7849645717912,43.7824931062278,
44.7800216406644,45.777550175101,46.7750787095376,47.1238898038469),
 .UNSPECIFIED.);
#2075=B_SPLINE_CURVE_WITH_KNOTS('',3,(#14470,#14471,#14472,#14473,#14474,
#14475,#14476,#14477,#14478,#14479),.UNSPECIFIED.,.F.,.F.,(4,1,1,1,1,1,
1,4),(40.8407044966673,41.3314114425651,42.3289399770017,43.3264685114383,
44.3239970458749,45.3215255803115,46.3190541147481,47.1238898038469),
 .UNSPECIFIED.);
#2076=B_SPLINE_CURVE_WITH_KNOTS('',3,(#14484,#14485,#14486,#14487,#14488,
#14489,#14490,#14491,#14492,#14493,#14494),.UNSPECIFIED.,.F.,.F.,(4,1,1,
1,1,1,1,1,4),(34.5575191894876,34.8047362962984,35.802264830735,36.7997933651716,
37.7973218996082,38.7948504340448,39.7923789684814,40.789907502918,40.8407044966673),
 .UNSPECIFIED.);
#2077=B_SPLINE_CURVE_WITH_KNOTS('',3,(#14495,#14496,#14497,#14498,#14499,
#14500,#14501,#14502,#14503,#14504),.UNSPECIFIED.,.F.,.F.,(4,1,1,1,1,1,
1,4),(34.5575191894876,35.3462402359455,36.3437687703821,37.3412973048187,
38.3388258392553,39.3363543736919,40.3338829081285,40.8407044966673),
 .UNSPECIFIED.);
#2078=B_SPLINE_CURVE_WITH_KNOTS('',3,(#14509,#14510,#14511,#14512,#14513,
#14514,#14515,#14516,#14517,#14518),.UNSPECIFIED.,.F.,.F.,(4,1,1,1,1,1,
1,4),(28.2743338823081,28.8195650896788,29.8170936241154,30.814622158552,
31.8121506929886,32.8096792274252,33.8072077618618,34.5575191894876),
 .UNSPECIFIED.);
#2079=B_SPLINE_CURVE_WITH_KNOTS('',3,(#14519,#14520,#14521,#14522,#14523,
#14524,#14525,#14526,#14527,#14528,#14529),.UNSPECIFIED.,.F.,.F.,(4,1,1,
1,1,1,1,1,4),(28.2743338823081,28.3635404948893,29.3610690293259,30.3585975637625,
31.3561260981991,32.3536546326357,33.3511831670723,34.3487117015089,34.5575191894876),
 .UNSPECIFIED.);
#2080=B_SPLINE_CURVE_WITH_KNOTS('',3,(#14534,#14535,#14536,#14537,#14538,
#14539,#14540,#14541,#14542,#14543),.UNSPECIFIED.,.F.,.F.,(4,1,1,1,1,1,
1,4),(21.9911485751285,22.8343938830592,23.8319224174958,24.8294509519324,
25.826979486369,26.8245080208056,27.8220365552422,28.2743338823081),
 .UNSPECIFIED.);
#2081=B_SPLINE_CURVE_WITH_KNOTS('',3,(#14544,#14545,#14546,#14547,#14548,
#14549,#14550,#14551,#14552,#14553),.UNSPECIFIED.,.F.,.F.,(4,1,1,1,1,1,
1,4),(21.9911485751285,22.3783692882697,23.3758978227063,24.3734263571429,
25.3709548915795,26.3684834260161,27.3660119604527,28.2743338823081),
 .UNSPECIFIED.);
#2082=B_SPLINE_CURVE_WITH_KNOTS('',3,(#14559,#14560,#14561,#14562,#14563),
 .UNSPECIFIED.,.F.,.F.,(4,1,4),(14.3981410127769,15.3956695472135,15.7079632679489),
 .UNSPECIFIED.);
#2083=B_SPLINE_CURVE_WITH_KNOTS('',3,(#14566,#14567,#14568,#14569,#14570),
 .UNSPECIFIED.,.F.,.F.,(4,1,4),(13.8761928695311,14.8541656075664,15.7079632679489),
 .UNSPECIFIED.);
#2084=B_SPLINE_CURVE_WITH_KNOTS('',3,(#14576,#14577,#14578,#14579,#14580,
#14581,#14582,#14583,#14584,#14585,#14586,#14587,#14588,#14589,#14590,#14591,
#14592,#14593,#14594),.UNSPECIFIED.,.F.,.F.,(4,3,3,3,3,3,4),(95.5576018628658,
95.7627393059136,96.7602678403502,97.7577963747868,98.7553249092234,99.75285344366,
100.750381978097),.UNSPECIFIED.);
#2085=B_SPLINE_CURVE_WITH_KNOTS('',3,(#14598,#14599,#14600,#14601),
 .UNSPECIFIED.,.F.,.F.,(4,4),(-98.735769112822,-98.0941628713861),
 .UNSPECIFIED.);
#2086=B_SPLINE_CURVE_WITH_KNOTS('',3,(#14605,#14606,#14607,#14608,#14609,
#14610,#14611,#14612,#14613,#14614,#14615,#14616,#14617,#14618,#14619,#14620,
#14621,#14622,#14623,#14624,#14625,#14626),.UNSPECIFIED.,.F.,.F.,(4,3,3,
3,3,3,3,4),(-98.0941628713861,-97.7577963747867,-96.7602678403501,-95.7627393059135,
-94.7652107714769,-93.7676822370404,-92.7701537026037,-91.8109775642065),
 .UNSPECIFIED.);
#2087=B_SPLINE_CURVE_WITH_KNOTS('',3,(#14631,#14632,#14633,#14634,#14635,
#14636,#14637,#14638,#14639,#14640,#14641,#14642,#14643,#14644,#14645,#14646,
#14647,#14648,#14649,#14650,#14651,#14652),.UNSPECIFIED.,.F.,.F.,(4,3,3,
3,3,3,3,4),(89.2744165556862,89.777568099294,90.7750966337306,91.7726251681672,
92.7701537026038,93.7676822370404,94.765210771477,95.5576018628658),
 .UNSPECIFIED.);
#2088=B_SPLINE_CURVE_WITH_KNOTS('',3,(#14653,#14654,#14655,#14656,#14657,
#14658,#14659,#14660,#14661,#14662,#14663,#14664,#14665,#14666,#14667,#14668,
#14669,#14670,#14671,#14672,#14673,#14674,#14675,#14676,#14677),
 .UNSPECIFIED.,.F.,.F.,(4,3,3,3,3,3,3,3,4),(-91.8109775642065,-91.7726251681671,
-90.7750966337306,-89.7775680992939,-88.7800395648573,-87.7825110304207,
-86.7849824959842,-85.7874539615475,-85.527792257027),.UNSPECIFIED.);
#2089=B_SPLINE_CURVE_WITH_KNOTS('',3,(#14682,#14683,#14684,#14685,#14686,
#14687,#14688,#14689,#14690,#14691,#14692,#14693,#14694,#14695,#14696,#14697,
#14698,#14699,#14700,#14701,#14702,#14703),.UNSPECIFIED.,.F.,.F.,(4,3,3,
3,3,3,3,4),(82.9912312485066,83.7923968926744,84.789925427111,85.7874539615476,
86.7849824959842,87.7825110304208,88.7800395648574,89.2744165556862),
 .UNSPECIFIED.);
#2090=B_SPLINE_CURVE_WITH_KNOTS('',3,(#14704,#14705,#14706,#14707,#14708,
#14709,#14710,#14711,#14712,#14713,#14714,#14715,#14716,#14717,#14718,#14719,
#14720,#14721,#14722,#14723,#14724,#14725),.UNSPECIFIED.,.F.,.F.,(4,3,3,
3,3,3,3,4),(-85.527792257027,-84.7899254271109,-83.7923968926744,-82.7948683582377,
-81.7973398238012,-80.7998112893646,-79.802282754928,-79.2446069498474),
 .UNSPECIFIED.);
#2091=B_SPLINE_CURVE_WITH_KNOTS('',3,(#14730,#14731,#14732,#14733,#14734,
#14735,#14736,#14737,#14738,#14739,#14740,#14741,#14742,#14743,#14744,#14745,
#14746,#14747,#14748,#14749,#14750,#14751,#14752,#14753,#14754),
 .UNSPECIFIED.,.F.,.F.,(4,3,3,3,3,3,3,3,4),(76.708045941327,76.8096971516182,
77.8072256860548,78.8047542204914,79.802282754928,80.7998112893646,81.7973398238012,
82.7948683582378,82.9912312485066),.UNSPECIFIED.);
#2092=B_SPLINE_CURVE_WITH_KNOTS('',3,(#14755,#14756,#14757,#14758,#14759,
#14760,#14761,#14762,#14763,#14764,#14765,#14766,#14767,#14768,#14769,#14770,
#14771,#14772,#14773,#14774,#14775,#14776),.UNSPECIFIED.,.F.,.F.,(4,3,3,
3,3,3,3,4),(-79.2446069498474,-78.8047542204914,-77.8072256860548,-76.8096971516182,
-75.8121686171816,-74.814640082745,-73.8171115483084,-72.9614216426678),
 .UNSPECIFIED.);
#2093=B_SPLINE_CURVE_WITH_KNOTS('',3,(#14781,#14782,#14783,#14784,#14785,
#14786,#14787,#14788,#14789,#14790,#14791,#14792,#14793,#14794,#14795,#14796,
#14797,#14798,#14799,#14800,#14801,#14802),.UNSPECIFIED.,.F.,.F.,(4,3,3,
3,3,3,3,4),(70.4248606341474,70.8245259449986,71.8220544794352,72.8195830138718,
73.8171115483084,74.814640082745,75.8121686171816,76.708045941327),
 .UNSPECIFIED.);
#2094=B_SPLINE_CURVE_WITH_KNOTS('',3,(#14803,#14804,#14805,#14806,#14807,
#14808,#14809,#14810,#14811,#14812,#14813,#14814,#14815,#14816,#14817,#14818,
#14819,#14820,#14821,#14822,#14823,#14824,#14825,#14826,#14827),
 .UNSPECIFIED.,.F.,.F.,(4,3,3,3,3,3,3,3,4),(-72.9614216426678,-72.8195830138717,
-71.8220544794352,-70.8245259449986,-69.826997410562,-68.8294688761254,
-67.8319403416887,-66.8344118072522,-66.6782363354882),.UNSPECIFIED.);
#2095=B_SPLINE_CURVE_WITH_KNOTS('',3,(#14832,#14833,#14834,#14835,#14836,
#14837,#14838,#14839,#14840,#14841,#14842,#14843,#14844,#14845,#14846,#14847,
#14848,#14849,#14850,#14851,#14852,#14853),.UNSPECIFIED.,.F.,.F.,(4,3,3,
3,3,3,3,4),(64.1416753269678,64.839354738379,65.8368832728156,66.8344118072522,
67.8319403416888,68.8294688761254,69.826997410562,70.4248606341474),
 .UNSPECIFIED.);
#2096=B_SPLINE_CURVE_WITH_KNOTS('',3,(#14854,#14855,#14856,#14857,#14858,
#14859,#14860,#14861,#14862,#14863,#14864,#14865,#14866,#14867,#14868,#14869,
#14870,#14871,#14872,#14873,#14874,#14875),.UNSPECIFIED.,.F.,.F.,(4,3,3,
3,3,3,3,4),(-66.6782363354882,-65.8368832728156,-64.839354738379,-63.8418262039424,
-62.8442976695058,-61.8467691350692,-60.8492406006326,-60.3950510283086),
 .UNSPECIFIED.);
#2097=B_SPLINE_CURVE_WITH_KNOTS('',3,(#14880,#14881,#14882,#14883,#14884,
#14885,#14886,#14887,#14888,#14889,#14890,#14891,#14892,#14893,#14894,#14895,
#14896,#14897,#14898,#14899,#14900,#14901),.UNSPECIFIED.,.F.,.F.,(4,3,3,
3,3,3,3,4),(57.8584900197882,58.8541835317594,59.851712066196,60.8492406006326,
61.8467691350692,62.8442976695058,63.8418262039424,64.1416753269678),
 .UNSPECIFIED.);
#2098=B_SPLINE_CURVE_WITH_KNOTS('',3,(#14902,#14903,#14904,#14905,#14906,
#14907,#14908,#14909,#14910,#14911,#14912,#14913,#14914,#14915,#14916,#14917,
#14918,#14919,#14920,#14921,#14922,#14923),.UNSPECIFIED.,.F.,.F.,(4,3,3,
3,3,3,3,4),(-60.3950510283086,-59.851712066196,-58.8541835317594,-57.8566549973228,
-56.8591264628862,-55.8615979284496,-54.864069394013,-54.111865721129),
 .UNSPECIFIED.);
#2099=B_SPLINE_CURVE_WITH_KNOTS('',3,(#14928,#14929,#14930,#14931,#14932,
#14933,#14934,#14935,#14936,#14937,#14938,#14939,#14940,#14941,#14942,#14943,
#14944,#14945,#14946,#14947,#14948,#14949),.UNSPECIFIED.,.F.,.F.,(4,3,3,
3,3,3,3,4),(51.5753047126086,51.8714837907032,52.8690123251398,53.8665408595764,
54.864069394013,55.8615979284496,56.8591264628862,57.8584900197882),
 .UNSPECIFIED.);
#2100=B_SPLINE_CURVE_WITH_KNOTS('',3,(#14950,#14951,#14952,#14953,#14954,
#14955,#14956,#14957,#14958,#14959,#14960,#14961,#14962,#14963,#14964,#14965,
#14966,#14967,#14968,#14969,#14970,#14971,#14972,#14973,#14974),
 .UNSPECIFIED.,.F.,.F.,(4,3,3,3,3,3,3,3,4),(-54.111865721129,-53.8665408595764,
-52.8690123251398,-51.8714837907032,-50.8739552562666,-49.87642672183,-48.8788981873934,
-47.8813696529568,-47.8286804139494),.UNSPECIFIED.);
#2101=B_SPLINE_CURVE_WITH_KNOTS('',3,(#14979,#14980,#14981,#14982,#14983,
#14984,#14985,#14986,#14987,#14988,#14989,#14990,#14991,#14992,#14993,#14994,
#14995,#14996,#14997,#14998,#14999,#15000),.UNSPECIFIED.,.F.,.F.,(4,3,3,
3,3,3,3,4),(45.292119405429,45.8863125840836,46.8838411185202,47.8813696529568,
48.8788981873934,49.87642672183,50.8739552562666,51.5753047126086),
 .UNSPECIFIED.);
#2102=B_SPLINE_CURVE_WITH_KNOTS('',3,(#15001,#15002,#15003,#15004,#15005,
#15006,#15007,#15008,#15009,#15010,#15011,#15012,#15013,#15014,#15015,#15016,
#15017,#15018,#15019,#15020,#15021,#15022),.UNSPECIFIED.,.F.,.F.,(4,3,3,
3,3,3,3,4),(-47.8286804139494,-46.8838411185202,-45.8863125840836,-44.888784049647,
-43.8912555152104,-42.8937269807738,-41.8961984463372,-41.5454951067698),
 .UNSPECIFIED.);
#2103=B_SPLINE_CURVE_WITH_KNOTS('',3,(#15027,#15028,#15029,#15030,#15031,
#15032,#15033,#15034,#15035,#15036,#15037,#15038,#15039,#15040,#15041,#15042,
#15043,#15044,#15045,#15046,#15047,#15048),.UNSPECIFIED.,.F.,.F.,(4,3,3,
3,3,3,3,4),(39.0089340982494,39.901141377464,40.8986699119006,41.8961984463372,
42.8937269807738,43.8912555152104,44.888784049647,45.292119405429),
 .UNSPECIFIED.);
#2104=B_SPLINE_CURVE_WITH_KNOTS('',3,(#15049,#15050,#15051,#15052,#15053,
#15054,#15055,#15056,#15057,#15058,#15059,#15060,#15061,#15062,#15063,#15064,
#15065,#15066,#15067,#15068,#15069,#15070),.UNSPECIFIED.,.F.,.F.,(4,3,3,
3,3,3,3,4),(-41.5454951067698,-40.8986699119006,-39.901141377464,-38.9036128430274,
-37.9060843085908,-36.9085557741542,-35.9110272397176,-35.2623097995902),
 .UNSPECIFIED.);
#2105=B_SPLINE_CURVE_WITH_KNOTS('',3,(#15075,#15076,#15077,#15078,#15079,
#15080,#15081,#15082,#15083,#15084,#15085,#15086,#15087,#15088,#15089,#15090,
#15091,#15092,#15093,#15094,#15095,#15096,#15097,#15098,#15099),
 .UNSPECIFIED.,.F.,.F.,(4,3,3,3,3,3,3,3,4),(32.7257487910699,32.9184416364078,
33.9159701708444,34.913498705281,35.9110272397176,36.9085557741542,37.9060843085908,
38.9036128430274,39.0089340982494),.UNSPECIFIED.);
#2106=B_SPLINE_CURVE_WITH_KNOTS('',3,(#15100,#15101,#15102,#15103,#15104,
#15105,#15106,#15107,#15108,#15109,#15110,#15111,#15112,#15113,#15114,#15115,
#15116,#15117,#15118,#15119,#15120,#15121),.UNSPECIFIED.,.F.,.F.,(4,3,3,
3,3,3,3,4),(-35.2623097995902,-34.913498705281,-33.9159701708444,-32.9184416364078,
-31.9209131019712,-30.9233845675346,-29.925856033098,-28.9791244924106),
 .UNSPECIFIED.);
#2107=B_SPLINE_CURVE_WITH_KNOTS('',3,(#15126,#15127,#15128,#15129,#15130,
#15131,#15132,#15133,#15134,#15135,#15136,#15137,#15138,#15139,#15140,#15141,
#15142,#15143,#15144,#15145,#15146,#15147),.UNSPECIFIED.,.F.,.F.,(4,3,3,
3,3,3,3,4),(26.4425634838902,26.9332704297882,27.9307989642248,28.9283274986614,
29.925856033098,30.9233845675346,31.9209131019712,32.7257487910699),
 .UNSPECIFIED.);
#2108=B_SPLINE_CURVE_WITH_KNOTS('',3,(#15148,#15149,#15150,#15151,#15152,
#15153,#15154,#15155,#15156,#15157,#15158,#15159,#15160,#15161,#15162,#15163,
#15164,#15165,#15166,#15167,#15168,#15169,#15170,#15171,#15172),
 .UNSPECIFIED.,.F.,.F.,(4,3,3,3,3,3,3,3,4),(-28.9791244924106,-28.9283274986614,
-27.9307989642248,-26.9332704297882,-25.9357418953516,-24.938213360915,
-23.9406848264784,-22.9431562920418,-22.695939185231),.UNSPECIFIED.);
#2109=B_SPLINE_CURVE_WITH_KNOTS('',3,(#15177,#15178,#15179,#15180,#15181,
#15182,#15183,#15184,#15185,#15186,#15187,#15188,#15189,#15190,#15191,#15192,
#15193,#15194,#15195,#15196,#15197,#15198),.UNSPECIFIED.,.F.,.F.,(4,3,3,
3,3,3,3,4),(20.1593781767107,20.9480992231686,21.9456277576052,22.9431562920418,
23.9406848264784,24.938213360915,25.9357418953516,26.4425634838902),
 .UNSPECIFIED.);
#2110=B_SPLINE_CURVE_WITH_KNOTS('',3,(#15199,#15200,#15201,#15202,#15203,
#15204,#15205,#15206,#15207,#15208,#15209,#15210,#15211,#15212,#15213,#15214,
#15215,#15216,#15217,#15218,#15219,#15220),.UNSPECIFIED.,.F.,.F.,(4,3,3,
3,3,3,3,4),(-22.695939185231,-21.9456277576052,-20.9480992231686,-19.950570688732,
-18.9530421542954,-17.9555136198588,-16.9579850854222,-16.4127538780514),
 .UNSPECIFIED.);
#2111=B_SPLINE_CURVE_WITH_KNOTS('',3,(#15225,#15226,#15227,#15228,#15229,
#15230,#15231,#15232,#15233,#15234,#15235,#15236,#15237,#15238,#15239,#15240,
#15241,#15242,#15243,#15244,#15245,#15246,#15247,#15248,#15249),
 .UNSPECIFIED.,.F.,.F.,(4,3,3,3,3,3,3,3,4),(13.8761928695311,13.9653994821124,
14.962928016549,15.9604565509856,16.9579850854222,17.9555136198588,18.9530421542954,
19.950570688732,20.1593781767107),.UNSPECIFIED.);
#2112=B_SPLINE_CURVE_WITH_KNOTS('',3,(#15250,#15251,#15252,#15253,#15254,
#15255,#15256,#15257,#15258,#15259,#15260,#15261,#15262,#15263,#15264,#15265,
#15266,#15267,#15268,#15269,#15270,#15271),.UNSPECIFIED.,.F.,.F.,(4,3,3,
3,3,3,3,4),(-16.4127538780514,-15.9604565509856,-14.962928016549,-13.9653994821124,
-12.9678709476758,-11.9703424132392,-10.9728138788026,-10.1295685708719),
 .UNSPECIFIED.);
#2113=B_SPLINE_CURVE_WITH_KNOTS('',3,(#15277,#15278,#15279,#15280,#15281,
#15282,#15283,#15284,#15285,#15286,#15287,#15288,#15289),.UNSPECIFIED.,
 .F.,.F.,(4,3,3,3,4),(-3.84638326369226,-2.9925856033098,-1.9950570688732,
-0.997528534436601,0.),.UNSPECIFIED.);
#2114=B_SPLINE_CURVE_WITH_KNOTS('',3,(#15292,#15293,#15294,#15295,#15296,
#15297,#15298,#15299,#15300,#15301,#15302,#15303,#15304,#15305,#15306,#15307,
#15308,#15309,#15310),.UNSPECIFIED.,.F.,.F.,(4,3,3,3,3,3,4),(2.01461286527449,
2.9925856033098,3.9901141377464,4.987642672183,5.9851712066196,6.9826997410562,
7.59300756235149),.UNSPECIFIED.);
#2115=B_SPLINE_CURVE_WITH_KNOTS('',3,(#15316,#15317,#15318,#15319,#15320,
#15321),.UNSPECIFIED.,.F.,.F.,(4,1,1,4),(109.955742875643,110.61690491348,
111.614433447917,112.611961982353),.UNSPECIFIED.);
#2116=B_SPLINE_CURVE_WITH_KNOTS('',3,(#15324,#15325,#15326,#15327,#15328,
#15329,#15330),.UNSPECIFIED.,.F.,.F.,(4,1,1,1,4),(109.955742875643,110.16088031869,
111.158408853127,112.155937387564,113.133910125599),.UNSPECIFIED.);
#2117=B_SPLINE_CURVE_WITH_KNOTS('',3,(#15335,#15336,#15337,#15338,#15339,
#15340,#15341,#15342,#15343,#15344),.UNSPECIFIED.,.F.,.F.,(4,1,1,1,1,1,
1,4),(103.672557568463,104.63173370686,105.629262241297,106.626790775734,
107.62431931017,108.621847844607,109.619376379043,109.955742875643),
 .UNSPECIFIED.);
#2118=B_SPLINE_CURVE_WITH_KNOTS('',3,(#15345,#15346,#15347,#15348,#15349,
#15350,#15351,#15352,#15353,#15354),.UNSPECIFIED.,.F.,.F.,(4,1,1,1,1,1,
1,4),(103.672557568463,104.175709112071,105.173237646507,106.170766180944,
107.168294715381,108.165823249817,109.163351784254,109.955742875643),
 .UNSPECIFIED.);
#2119=B_SPLINE_CURVE_WITH_KNOTS('',3,(#15359,#15360,#15361,#15362,#15363,
#15364,#15365,#15366,#15367,#15368,#15369),.UNSPECIFIED.,.F.,.F.,(4,1,1,
1,1,1,1,1,4),(97.3893722612835,97.6490339658042,98.6465625002408,99.6440910346774,
100.641619569114,101.639148103551,102.636676637987,103.634205172424,103.672557568463),
 .UNSPECIFIED.);
#2120=B_SPLINE_CURVE_WITH_KNOTS('',3,(#15370,#15371,#15372,#15373,#15374,
#15375,#15376,#15377,#15378,#15379),.UNSPECIFIED.,.F.,.F.,(4,1,1,1,1,1,
1,4),(97.3893722612835,98.1905379054513,99.1880664398879,100.185594974324,
101.183123508761,102.180652043198,103.178180577634,103.672557568463),
 .UNSPECIFIED.);
#2121=B_SPLINE_CURVE_WITH_KNOTS('',3,(#15384,#15385,#15386,#15387,#15388,
#15389,#15390,#15391,#15392,#15393),.UNSPECIFIED.,.F.,.F.,(4,1,1,1,1,1,
1,4),(91.106186954104,91.6638627591846,92.6613912936212,93.6589198280578,
94.6564483624944,95.653976896931,96.6515054313676,97.3893722612835),
 .UNSPECIFIED.);
#2122=B_SPLINE_CURVE_WITH_KNOTS('',3,(#15394,#15395,#15396,#15397,#15398,
#15399,#15400,#15401,#15402,#15403,#15404),.UNSPECIFIED.,.F.,.F.,(4,1,1,
1,1,1,1,1,4),(91.106186954104,91.2078381643951,92.2053666988317,93.2028952332683,
94.2004237677049,95.1979523021415,96.1954808365781,97.1930093710147,97.3893722612835),
 .UNSPECIFIED.);
#2123=B_SPLINE_CURVE_WITH_KNOTS('',3,(#15409,#15410,#15411,#15412,#15413,
#15414,#15415,#15416,#15417,#15418),.UNSPECIFIED.,.F.,.F.,(4,1,1,1,1,1,
1,4),(84.8230016469244,85.678691552565,86.6762200870016,87.6737486214382,
88.6712771558748,89.6688056903114,90.666334224748,91.106186954104),
 .UNSPECIFIED.);
#2124=B_SPLINE_CURVE_WITH_KNOTS('',3,(#15419,#15420,#15421,#15422,#15423,
#15424,#15425,#15426,#15427,#15428),.UNSPECIFIED.,.F.,.F.,(4,1,1,1,1,1,
1,4),(84.8230016469244,85.2226669577755,86.2201954922121,87.2177240266487,
88.2152525610853,89.2127810955219,90.2103096299585,91.106186954104),
 .UNSPECIFIED.);
#2125=B_SPLINE_CURVE_WITH_KNOTS('',3,(#15433,#15434,#15435,#15436,#15437,
#15438,#15439,#15440,#15441,#15442,#15443),.UNSPECIFIED.,.F.,.F.,(4,1,1,
1,1,1,1,1,4),(78.5398163397448,78.6959918115088,79.6935203459454,80.691048880382,
81.6885774148186,82.6861059492552,83.6836344836918,84.6811630181284,84.8230016469244),
 .UNSPECIFIED.);
#2126=B_SPLINE_CURVE_WITH_KNOTS('',3,(#15444,#15445,#15446,#15447,#15448,
#15449,#15450,#15451,#15452,#15453),.UNSPECIFIED.,.F.,.F.,(4,1,1,1,1,1,
1,4),(78.5398163397448,79.2374957511559,80.2350242855925,81.2325528200291,
82.2300813544657,83.2276098889023,84.2251384233389,84.8230016469244),
 .UNSPECIFIED.);
#2127=B_SPLINE_CURVE_WITH_KNOTS('',3,(#15458,#15459,#15460,#15461,#15462,
#15463,#15464,#15465,#15466,#15467),.UNSPECIFIED.,.F.,.F.,(4,1,1,1,1,1,
1,4),(72.2566310325652,72.7108206048892,73.7083491393258,74.7058776737624,
75.703406208199,76.7009347426356,77.6984632770722,78.5398163397448),
 .UNSPECIFIED.);
#2128=B_SPLINE_CURVE_WITH_KNOTS('',3,(#15468,#15469,#15470,#15471,#15472,
#15473,#15474,#15475,#15476,#15477),.UNSPECIFIED.,.F.,.F.,(4,1,1,1,1,1,
1,4),(72.2566310325652,73.2523245445363,74.2498530789729,75.2473816134095,
76.2449101478461,77.2424386822827,78.2399672167193,78.5398163397448),
 .UNSPECIFIED.);
#2129=B_SPLINE_CURVE_WITH_KNOTS('',3,(#15482,#15483,#15484,#15485,#15486,
#15487,#15488,#15489,#15490,#15491),.UNSPECIFIED.,.F.,.F.,(4,1,1,1,1,1,
1,4),(65.9734457253856,66.7256493982696,67.7231779327062,68.7207064671428,
69.7182350015794,70.715763536016,71.7132920704526,72.2566310325652),
 .UNSPECIFIED.);
#2130=B_SPLINE_CURVE_WITH_KNOTS('',3,(#15492,#15493,#15494,#15495,#15496,
#15497,#15498,#15499,#15500,#15501,#15502),.UNSPECIFIED.,.F.,.F.,(4,1,1,
1,1,1,1,1,4),(65.9734457253856,66.2696248034801,67.2671533379167,68.2646818723533,
69.2622104067899,70.2597389412265,71.2572674756631,72.2547960100997,72.2566310325652),
 .UNSPECIFIED.);
#2131=B_SPLINE_CURVE_WITH_KNOTS('',3,(#15507,#15508,#15509,#15510,#15511,
#15512,#15513,#15514,#15515,#15516,#15517),.UNSPECIFIED.,.F.,.F.,(4,1,1,
1,1,1,1,1,4),(59.690260418206,59.7429496572134,60.74047819165,61.7380067260866,
62.7355352605232,63.7330637949598,64.7305923293964,65.728120863833,65.9734457253856),
 .UNSPECIFIED.);
#2132=B_SPLINE_CURVE_WITH_KNOTS('',3,(#15518,#15519,#15520,#15521,#15522,
#15523,#15524,#15525,#15526,#15527),.UNSPECIFIED.,.F.,.F.,(4,1,1,1,1,1,
1,4),(59.690260418206,60.2844535968605,61.2819821312971,62.2795106657337,
63.2770392001703,64.2745677346069,65.2720962690435,65.9734457253856),
 .UNSPECIFIED.);
#2133=B_SPLINE_CURVE_WITH_KNOTS('',3,(#15532,#15533,#15534,#15535,#15536,
#15537,#15538,#15539,#15540,#15541),.UNSPECIFIED.,.F.,.F.,(4,1,1,1,1,1,
1,4),(53.4070751110264,53.7577784505938,54.7553069850304,55.752835519467,
56.7503640539036,57.7478925883402,58.7454211227768,59.690260418206),
 .UNSPECIFIED.);
#2134=B_SPLINE_CURVE_WITH_KNOTS('',3,(#15542,#15543,#15544,#15545,#15546,
#15547,#15548,#15549,#15550,#15551),.UNSPECIFIED.,.F.,.F.,(4,1,1,1,1,1,
1,4),(53.4070751110264,54.2992823902409,55.2968109246775,56.2943394591141,
57.2918679935507,58.2893965279873,59.2869250624239,59.690260418206),
 .UNSPECIFIED.);
#2135=B_SPLINE_CURVE_WITH_KNOTS('',3,(#15556,#15557,#15558,#15559,#15560,
#15561,#15562,#15563,#15564,#15565),.UNSPECIFIED.,.F.,.F.,(4,1,1,1,1,1,
1,4),(47.1238898038468,47.7726072439742,48.7701357784108,49.7676643128474,
50.765192847284,51.7627213817206,52.7602499161572,53.4070751110264),
 .UNSPECIFIED.);
#2136=B_SPLINE_CURVE_WITH_KNOTS('',3,(#15566,#15567,#15568,#15569,#15570,
#15571,#15572,#15573,#15574,#15575,#15576),.UNSPECIFIED.,.F.,.F.,(4,1,1,
1,1,1,1,1,4),(47.1238898038468,47.3165826491847,48.3141111836213,49.3116397180579,
50.3091682524945,51.3066967869311,52.3042253213677,53.3017538558043,53.4070751110264),
 .UNSPECIFIED.);
#2137=B_SPLINE_CURVE_WITH_KNOTS('',3,(#15581,#15582,#15583,#15584,#15585,
#15586,#15587,#15588,#15589,#15590),.UNSPECIFIED.,.F.,.F.,(4,1,1,1,1,1,
1,4),(40.8407044966673,41.7874360373546,42.7849645717912,43.7824931062278,
44.7800216406644,45.777550175101,46.7750787095376,47.1238898038468),
 .UNSPECIFIED.);
#2138=B_SPLINE_CURVE_WITH_KNOTS('',3,(#15591,#15592,#15593,#15594,#15595,
#15596,#15597,#15598,#15599,#15600),.UNSPECIFIED.,.F.,.F.,(4,1,1,1,1,1,
1,4),(40.8407044966673,41.3314114425651,42.3289399770017,43.3264685114383,
44.3239970458749,45.3215255803115,46.3190541147481,47.1238898038468),
 .UNSPECIFIED.);
#2139=B_SPLINE_CURVE_WITH_KNOTS('',3,(#15605,#15606,#15607,#15608,#15609,
#15610,#15611,#15612,#15613,#15614,#15615),.UNSPECIFIED.,.F.,.F.,(4,1,1,
1,1,1,1,1,4),(34.5575191894876,34.8047362962984,35.802264830735,36.7997933651716,
37.7973218996082,38.7948504340448,39.7923789684814,40.789907502918,40.8407044966673),
 .UNSPECIFIED.);
#2140=B_SPLINE_CURVE_WITH_KNOTS('',3,(#15616,#15617,#15618,#15619,#15620,
#15621,#15622,#15623,#15624,#15625),.UNSPECIFIED.,.F.,.F.,(4,1,1,1,1,1,
1,4),(34.5575191894876,35.3462402359455,36.3437687703821,37.3412973048187,
38.3388258392553,39.3363543736919,40.3338829081285,40.8407044966673),
 .UNSPECIFIED.);
#2141=B_SPLINE_CURVE_WITH_KNOTS('',3,(#15630,#15631,#15632,#15633,#15634,
#15635,#15636,#15637,#15638,#15639),.UNSPECIFIED.,.F.,.F.,(4,1,1,1,1,1,
1,4),(28.2743338823081,28.8195650896788,29.8170936241154,30.814622158552,
31.8121506929886,32.8096792274252,33.8072077618618,34.5575191894876),
 .UNSPECIFIED.);
#2142=B_SPLINE_CURVE_WITH_KNOTS('',3,(#15640,#15641,#15642,#15643,#15644,
#15645,#15646,#15647,#15648,#15649,#15650),.UNSPECIFIED.,.F.,.F.,(4,1,1,
1,1,1,1,1,4),(28.2743338823081,28.3635404948893,29.3610690293259,30.3585975637625,
31.3561260981991,32.3536546326357,33.3511831670723,34.3487117015089,34.5575191894876),
 .UNSPECIFIED.);
#2143=B_SPLINE_CURVE_WITH_KNOTS('',3,(#15655,#15656,#15657,#15658,#15659,
#15660,#15661,#15662,#15663,#15664),.UNSPECIFIED.,.F.,.F.,(4,1,1,1,1,1,
1,4),(21.9911485751284,22.8343938830592,23.8319224174958,24.8294509519324,
25.826979486369,26.8245080208056,27.8220365552422,28.2743338823081),
 .UNSPECIFIED.);
#2144=B_SPLINE_CURVE_WITH_KNOTS('',3,(#15665,#15666,#15667,#15668,#15669,
#15670,#15671,#15672,#15673,#15674),.UNSPECIFIED.,.F.,.F.,(4,1,1,1,1,1,
1,4),(21.9911485751284,22.3783692882697,23.3758978227063,24.3734263571429,
25.3709548915795,26.3684834260161,27.3660119604527,28.2743338823081),
 .UNSPECIFIED.);
#2145=B_SPLINE_CURVE_WITH_KNOTS('',3,(#15680,#15681,#15682,#15683,#15684),
 .UNSPECIFIED.,.F.,.F.,(4,1,4),(14.3981410127769,15.3956695472135,15.7079632679489),
 .UNSPECIFIED.);
#2146=B_SPLINE_CURVE_WITH_KNOTS('',3,(#15687,#15688,#15689,#15690,#15691),
 .UNSPECIFIED.,.F.,.F.,(4,1,4),(13.8761928695311,14.8541656075664,15.7079632679489),
 .UNSPECIFIED.);
#2147=B_SPLINE_CURVE_WITH_KNOTS('',3,(#15697,#15698,#15699,#15700,#15701,
#15702,#15703,#15704,#15705,#15706,#15707,#15708,#15709,#15710,#15711,#15712,
#15713,#15714,#15715),.UNSPECIFIED.,.F.,.F.,(4,3,3,3,3,3,4),(95.5576018628658,
95.7627393059135,96.7602678403502,97.7577963747867,98.7553249092234,99.75285344366,
100.750381978096),.UNSPECIFIED.);
#2148=B_SPLINE_CURVE_WITH_KNOTS('',3,(#15719,#15720,#15721,#15722),
 .UNSPECIFIED.,.F.,.F.,(4,4),(-98.735769112822,-98.0941628713861),
 .UNSPECIFIED.);
#2149=B_SPLINE_CURVE_WITH_KNOTS('',3,(#15726,#15727,#15728,#15729,#15730,
#15731,#15732,#15733,#15734,#15735,#15736,#15737,#15738,#15739,#15740,#15741,
#15742,#15743,#15744,#15745,#15746,#15747),.UNSPECIFIED.,.F.,.F.,(4,3,3,
3,3,3,3,4),(-98.0941628713861,-97.7577963747868,-96.7602678403502,-95.7627393059136,
-94.765210771477,-93.7676822370404,-92.7701537026038,-91.8109775642066),
 .UNSPECIFIED.);
#2150=B_SPLINE_CURVE_WITH_KNOTS('',3,(#15752,#15753,#15754,#15755,#15756,
#15757,#15758,#15759,#15760,#15761,#15762,#15763,#15764,#15765,#15766,#15767,
#15768,#15769,#15770,#15771,#15772,#15773),.UNSPECIFIED.,.F.,.F.,(4,3,3,
3,3,3,3,4),(89.2744165556862,89.777568099294,90.7750966337306,91.7726251681672,
92.7701537026037,93.7676822370404,94.7652107714769,95.5576018628658),
 .UNSPECIFIED.);
#2151=B_SPLINE_CURVE_WITH_KNOTS('',3,(#15774,#15775,#15776,#15777,#15778,
#15779,#15780,#15781,#15782,#15783,#15784,#15785,#15786,#15787,#15788,#15789,
#15790,#15791,#15792,#15793,#15794,#15795,#15796,#15797,#15798),
 .UNSPECIFIED.,.F.,.F.,(4,3,3,3,3,3,3,3,4),(-91.8109775642066,-91.7726251681672,
-90.7750966337306,-89.777568099294,-88.7800395648574,-87.7825110304208,
-86.7849824959842,-85.7874539615476,-85.527792257027),.UNSPECIFIED.);
#2152=B_SPLINE_CURVE_WITH_KNOTS('',3,(#15803,#15804,#15805,#15806,#15807,
#15808,#15809,#15810,#15811,#15812,#15813,#15814,#15815,#15816,#15817,#15818,
#15819,#15820,#15821,#15822,#15823,#15824),.UNSPECIFIED.,.F.,.F.,(4,3,3,
3,3,3,3,4),(82.9912312485066,83.7923968926744,84.789925427111,85.7874539615476,
86.7849824959842,87.7825110304208,88.7800395648573,89.2744165556862),
 .UNSPECIFIED.);
#2153=B_SPLINE_CURVE_WITH_KNOTS('',3,(#15825,#15826,#15827,#15828,#15829,
#15830,#15831,#15832,#15833,#15834,#15835,#15836,#15837,#15838,#15839,#15840,
#15841,#15842,#15843,#15844,#15845,#15846),.UNSPECIFIED.,.F.,.F.,(4,3,3,
3,3,3,3,4),(-85.527792257027,-84.789925427111,-83.7923968926744,-82.7948683582378,
-81.7973398238012,-80.7998112893646,-79.802282754928,-79.2446069498474),
 .UNSPECIFIED.);
#2154=B_SPLINE_CURVE_WITH_KNOTS('',3,(#15851,#15852,#15853,#15854,#15855,
#15856,#15857,#15858,#15859,#15860,#15861,#15862,#15863,#15864,#15865,#15866,
#15867,#15868,#15869,#15870,#15871,#15872,#15873,#15874,#15875),
 .UNSPECIFIED.,.F.,.F.,(4,3,3,3,3,3,3,3,4),(76.708045941327,76.8096971516182,
77.8072256860548,78.8047542204914,79.802282754928,80.7998112893646,81.7973398238012,
82.7948683582378,82.9912312485066),.UNSPECIFIED.);
#2155=B_SPLINE_CURVE_WITH_KNOTS('',3,(#15876,#15877,#15878,#15879,#15880,
#15881,#15882,#15883,#15884,#15885,#15886,#15887,#15888,#15889,#15890,#15891,
#15892,#15893,#15894,#15895,#15896,#15897),.UNSPECIFIED.,.F.,.F.,(4,3,3,
3,3,3,3,4),(-79.2446069498474,-78.8047542204914,-77.8072256860548,-76.8096971516182,
-75.8121686171816,-74.814640082745,-73.8171115483084,-72.9614216426678),
 .UNSPECIFIED.);
#2156=B_SPLINE_CURVE_WITH_KNOTS('',3,(#15902,#15903,#15904,#15905,#15906,
#15907,#15908,#15909,#15910,#15911,#15912,#15913,#15914,#15915,#15916,#15917,
#15918,#15919,#15920,#15921,#15922,#15923),.UNSPECIFIED.,.F.,.F.,(4,3,3,
3,3,3,3,4),(70.4248606341474,70.8245259449986,71.8220544794352,72.8195830138718,
73.8171115483084,74.814640082745,75.8121686171816,76.708045941327),
 .UNSPECIFIED.);
#2157=B_SPLINE_CURVE_WITH_KNOTS('',3,(#15924,#15925,#15926,#15927,#15928,
#15929,#15930,#15931,#15932,#15933,#15934,#15935,#15936,#15937,#15938,#15939,
#15940,#15941,#15942,#15943,#15944,#15945,#15946,#15947,#15948),
 .UNSPECIFIED.,.F.,.F.,(4,3,3,3,3,3,3,3,4),(-72.9614216426678,-72.8195830138718,
-71.8220544794352,-70.8245259449986,-69.826997410562,-68.8294688761254,
-67.8319403416888,-66.8344118072522,-66.6782363354882),.UNSPECIFIED.);
#2158=B_SPLINE_CURVE_WITH_KNOTS('',3,(#15953,#15954,#15955,#15956,#15957,
#15958,#15959,#15960,#15961,#15962,#15963,#15964,#15965,#15966,#15967,#15968,
#15969,#15970,#15971,#15972,#15973,#15974),.UNSPECIFIED.,.F.,.F.,(4,3,3,
3,3,3,3,4),(64.1416753269678,64.839354738379,65.8368832728156,66.8344118072522,
67.8319403416888,68.8294688761254,69.826997410562,70.4248606341474),
 .UNSPECIFIED.);
#2159=B_SPLINE_CURVE_WITH_KNOTS('',3,(#15975,#15976,#15977,#15978,#15979,
#15980,#15981,#15982,#15983,#15984,#15985,#15986,#15987,#15988,#15989,#15990,
#15991,#15992,#15993,#15994,#15995,#15996),.UNSPECIFIED.,.F.,.F.,(4,3,3,
3,3,3,3,4),(-66.6782363354882,-65.8368832728156,-64.839354738379,-63.8418262039424,
-62.8442976695058,-61.8467691350692,-60.8492406006326,-60.3950510283086),
 .UNSPECIFIED.);
#2160=B_SPLINE_CURVE_WITH_KNOTS('',3,(#16001,#16002,#16003,#16004,#16005,
#16006,#16007,#16008,#16009,#16010,#16011,#16012,#16013,#16014,#16015,#16016,
#16017,#16018,#16019,#16020,#16021,#16022),.UNSPECIFIED.,.F.,.F.,(4,3,3,
3,3,3,3,4),(57.8584900197883,58.8541835317594,59.851712066196,60.8492406006326,
61.8467691350692,62.8442976695058,63.8418262039424,64.1416753269678),
 .UNSPECIFIED.);
#2161=B_SPLINE_CURVE_WITH_KNOTS('',3,(#16023,#16024,#16025,#16026,#16027,
#16028,#16029,#16030,#16031,#16032,#16033,#16034,#16035,#16036,#16037,#16038,
#16039,#16040,#16041,#16042,#16043,#16044),.UNSPECIFIED.,.F.,.F.,(4,3,3,
3,3,3,3,4),(-60.3950510283086,-59.851712066196,-58.8541835317594,-57.8566549973228,
-56.8591264628862,-55.8615979284496,-54.864069394013,-54.111865721129),
 .UNSPECIFIED.);
#2162=B_SPLINE_CURVE_WITH_KNOTS('',3,(#16049,#16050,#16051,#16052,#16053,
#16054,#16055,#16056,#16057,#16058,#16059,#16060,#16061,#16062,#16063,#16064,
#16065,#16066,#16067,#16068,#16069,#16070),.UNSPECIFIED.,.F.,.F.,(4,3,3,
3,3,3,3,4),(51.5753047126087,51.8714837907032,52.8690123251398,53.8665408595764,
54.864069394013,55.8615979284496,56.8591264628862,57.8584900197883),
 .UNSPECIFIED.);
#2163=B_SPLINE_CURVE_WITH_KNOTS('',3,(#16071,#16072,#16073,#16074,#16075,
#16076,#16077,#16078,#16079,#16080,#16081,#16082,#16083,#16084,#16085,#16086,
#16087,#16088,#16089,#16090,#16091,#16092,#16093,#16094,#16095),
 .UNSPECIFIED.,.F.,.F.,(4,3,3,3,3,3,3,3,4),(-54.111865721129,-53.8665408595764,
-52.8690123251398,-51.8714837907032,-50.8739552562666,-49.87642672183,-48.8788981873934,
-47.8813696529568,-47.8286804139494),.UNSPECIFIED.);
#2164=B_SPLINE_CURVE_WITH_KNOTS('',3,(#16100,#16101,#16102,#16103,#16104,
#16105,#16106,#16107,#16108,#16109,#16110,#16111,#16112,#16113,#16114,#16115,
#16116,#16117,#16118,#16119,#16120,#16121),.UNSPECIFIED.,.F.,.F.,(4,3,3,
3,3,3,3,4),(45.292119405429,45.8863125840836,46.8838411185202,47.8813696529568,
48.8788981873934,49.87642672183,50.8739552562666,51.5753047126087),
 .UNSPECIFIED.);
#2165=B_SPLINE_CURVE_WITH_KNOTS('',3,(#16122,#16123,#16124,#16125,#16126,
#16127,#16128,#16129,#16130,#16131,#16132,#16133,#16134,#16135,#16136,#16137,
#16138,#16139,#16140,#16141,#16142,#16143),.UNSPECIFIED.,.F.,.F.,(4,3,3,
3,3,3,3,4),(-47.8286804139494,-46.8838411185202,-45.8863125840836,-44.888784049647,
-43.8912555152104,-42.8937269807738,-41.8961984463372,-41.5454951067698),
 .UNSPECIFIED.);
#2166=B_SPLINE_CURVE_WITH_KNOTS('',3,(#16148,#16149,#16150,#16151,#16152,
#16153,#16154,#16155,#16156,#16157,#16158,#16159,#16160,#16161,#16162,#16163,
#16164,#16165,#16166,#16167,#16168,#16169),.UNSPECIFIED.,.F.,.F.,(4,3,3,
3,3,3,3,4),(39.0089340982495,39.901141377464,40.8986699119006,41.8961984463372,
42.8937269807738,43.8912555152104,44.888784049647,45.292119405429),
 .UNSPECIFIED.);
#2167=B_SPLINE_CURVE_WITH_KNOTS('',3,(#16170,#16171,#16172,#16173,#16174,
#16175,#16176,#16177,#16178,#16179,#16180,#16181,#16182,#16183,#16184,#16185,
#16186,#16187,#16188,#16189,#16190,#16191),.UNSPECIFIED.,.F.,.F.,(4,3,3,
3,3,3,3,4),(-41.5454951067698,-40.8986699119006,-39.901141377464,-38.9036128430274,
-37.9060843085908,-36.9085557741542,-35.9110272397176,-35.2623097995902),
 .UNSPECIFIED.);
#2168=B_SPLINE_CURVE_WITH_KNOTS('',3,(#16196,#16197,#16198,#16199,#16200,
#16201,#16202,#16203,#16204,#16205,#16206,#16207,#16208,#16209,#16210,#16211,
#16212,#16213,#16214,#16215,#16216,#16217,#16218,#16219,#16220),
 .UNSPECIFIED.,.F.,.F.,(4,3,3,3,3,3,3,3,4),(32.7257487910699,32.9184416364078,
33.9159701708444,34.913498705281,35.9110272397176,36.9085557741542,37.9060843085908,
38.9036128430274,39.0089340982495),.UNSPECIFIED.);
#2169=B_SPLINE_CURVE_WITH_KNOTS('',3,(#16221,#16222,#16223,#16224,#16225,
#16226,#16227,#16228,#16229,#16230,#16231,#16232,#16233,#16234,#16235,#16236,
#16237,#16238,#16239,#16240,#16241,#16242),.UNSPECIFIED.,.F.,.F.,(4,3,3,
3,3,3,3,4),(-35.2623097995902,-34.913498705281,-33.9159701708444,-32.9184416364078,
-31.9209131019712,-30.9233845675346,-29.925856033098,-28.9791244924106),
 .UNSPECIFIED.);
#2170=B_SPLINE_CURVE_WITH_KNOTS('',3,(#16247,#16248,#16249,#16250,#16251,
#16252,#16253,#16254,#16255,#16256,#16257,#16258,#16259,#16260,#16261,#16262,
#16263,#16264,#16265,#16266,#16267,#16268),.UNSPECIFIED.,.F.,.F.,(4,3,3,
3,3,3,3,4),(26.4425634838903,26.9332704297882,27.9307989642248,28.9283274986614,
29.925856033098,30.9233845675346,31.9209131019712,32.7257487910699),
 .UNSPECIFIED.);
#2171=B_SPLINE_CURVE_WITH_KNOTS('',3,(#16269,#16270,#16271,#16272,#16273,
#16274,#16275,#16276,#16277,#16278,#16279,#16280,#16281,#16282,#16283,#16284,
#16285,#16286,#16287,#16288,#16289,#16290,#16291,#16292,#16293),
 .UNSPECIFIED.,.F.,.F.,(4,3,3,3,3,3,3,3,4),(-28.9791244924106,-28.9283274986614,
-27.9307989642248,-26.9332704297882,-25.9357418953516,-24.938213360915,
-23.9406848264784,-22.9431562920418,-22.6959391852311),.UNSPECIFIED.);
#2172=B_SPLINE_CURVE_WITH_KNOTS('',3,(#16298,#16299,#16300,#16301,#16302,
#16303,#16304,#16305,#16306,#16307,#16308,#16309,#16310,#16311,#16312,#16313,
#16314,#16315,#16316,#16317,#16318,#16319),.UNSPECIFIED.,.F.,.F.,(4,3,3,
3,3,3,3,4),(20.1593781767107,20.9480992231686,21.9456277576052,22.9431562920418,
23.9406848264784,24.938213360915,25.9357418953516,26.4425634838903),
 .UNSPECIFIED.);
#2173=B_SPLINE_CURVE_WITH_KNOTS('',3,(#16320,#16321,#16322,#16323,#16324,
#16325,#16326,#16327,#16328,#16329,#16330,#16331,#16332,#16333,#16334,#16335,
#16336,#16337,#16338,#16339,#16340,#16341),.UNSPECIFIED.,.F.,.F.,(4,3,3,
3,3,3,3,4),(-22.6959391852311,-21.9456277576052,-20.9480992231686,-19.950570688732,
-18.9530421542954,-17.9555136198588,-16.9579850854222,-16.4127538780514),
 .UNSPECIFIED.);
#2174=B_SPLINE_CURVE_WITH_KNOTS('',3,(#16346,#16347,#16348,#16349,#16350,
#16351,#16352,#16353,#16354,#16355,#16356,#16357,#16358,#16359,#16360,#16361,
#16362,#16363,#16364,#16365,#16366,#16367,#16368,#16369,#16370),
 .UNSPECIFIED.,.F.,.F.,(4,3,3,3,3,3,3,3,4),(13.8761928695311,13.9653994821124,
14.962928016549,15.9604565509856,16.9579850854222,17.9555136198588,18.9530421542954,
19.950570688732,20.1593781767107),.UNSPECIFIED.);
#2175=B_SPLINE_CURVE_WITH_KNOTS('',3,(#16371,#16372,#16373,#16374,#16375,
#16376,#16377,#16378,#16379,#16380,#16381,#16382,#16383,#16384,#16385,#16386,
#16387,#16388,#16389,#16390,#16391,#16392),.UNSPECIFIED.,.F.,.F.,(4,3,3,
3,3,3,3,4),(-16.4127538780514,-15.9604565509856,-14.962928016549,-13.9653994821124,
-12.9678709476758,-11.9703424132392,-10.9728138788026,-10.1295685708719),
 .UNSPECIFIED.);
#2176=B_SPLINE_CURVE_WITH_KNOTS('',3,(#16398,#16399,#16400,#16401,#16402,
#16403,#16404,#16405,#16406,#16407,#16408,#16409,#16410),.UNSPECIFIED.,
 .F.,.F.,(4,3,3,3,4),(-3.8463832636923,-2.9925856033098,-1.9950570688732,
-0.997528534436595,0.),.UNSPECIFIED.);
#2177=B_SPLINE_CURVE_WITH_KNOTS('',3,(#16413,#16414,#16415,#16416,#16417,
#16418,#16419,#16420,#16421,#16422,#16423,#16424,#16425,#16426,#16427,#16428,
#16429,#16430,#16431),.UNSPECIFIED.,.F.,.F.,(4,3,3,3,3,3,4),(2.01461286527449,
2.9925856033098,3.9901141377464,4.98764267218299,5.98517120661959,6.98269974105619,
7.59300756235153),.UNSPECIFIED.);
#2178=B_SPLINE_CURVE_WITH_KNOTS('',3,(#16437,#16438,#16439,#16440,#16441,
#16442),.UNSPECIFIED.,.F.,.F.,(4,1,1,4),(109.955742875643,110.61690491348,
111.614433447917,112.611961982353),.UNSPECIFIED.);
#2179=B_SPLINE_CURVE_WITH_KNOTS('',3,(#16445,#16446,#16447,#16448,#16449,
#16450,#16451),.UNSPECIFIED.,.F.,.F.,(4,1,1,1,4),(109.955742875643,110.16088031869,
111.158408853127,112.155937387564,113.133910125599),.UNSPECIFIED.);
#2180=B_SPLINE_CURVE_WITH_KNOTS('',3,(#16456,#16457,#16458,#16459,#16460,
#16461,#16462,#16463,#16464,#16465),.UNSPECIFIED.,.F.,.F.,(4,1,1,1,1,1,
1,4),(103.672557568463,104.63173370686,105.629262241297,106.626790775734,
107.62431931017,108.621847844607,109.619376379043,109.955742875643),
 .UNSPECIFIED.);
#2181=B_SPLINE_CURVE_WITH_KNOTS('',3,(#16466,#16467,#16468,#16469,#16470,
#16471,#16472,#16473,#16474,#16475),.UNSPECIFIED.,.F.,.F.,(4,1,1,1,1,1,
1,4),(103.672557568463,104.175709112071,105.173237646507,106.170766180944,
107.168294715381,108.165823249817,109.163351784254,109.955742875643),
 .UNSPECIFIED.);
#2182=B_SPLINE_CURVE_WITH_KNOTS('',3,(#16480,#16481,#16482,#16483,#16484,
#16485,#16486,#16487,#16488,#16489,#16490),.UNSPECIFIED.,.F.,.F.,(4,1,1,
1,1,1,1,1,4),(97.3893722612836,97.6490339658042,98.6465625002408,99.6440910346774,
100.641619569114,101.639148103551,102.636676637987,103.634205172424,103.672557568463),
 .UNSPECIFIED.);
#2183=B_SPLINE_CURVE_WITH_KNOTS('',3,(#16491,#16492,#16493,#16494,#16495,
#16496,#16497,#16498,#16499,#16500),.UNSPECIFIED.,.F.,.F.,(4,1,1,1,1,1,
1,4),(97.3893722612836,98.1905379054512,99.1880664398878,100.185594974324,
101.183123508761,102.180652043198,103.178180577634,103.672557568463),
 .UNSPECIFIED.);
#2184=B_SPLINE_CURVE_WITH_KNOTS('',3,(#16505,#16506,#16507,#16508,#16509,
#16510,#16511,#16512,#16513,#16514),.UNSPECIFIED.,.F.,.F.,(4,1,1,1,1,1,
1,4),(91.106186954104,91.6638627591846,92.6613912936212,93.6589198280578,
94.6564483624944,95.653976896931,96.6515054313676,97.3893722612836),
 .UNSPECIFIED.);
#2185=B_SPLINE_CURVE_WITH_KNOTS('',3,(#16515,#16516,#16517,#16518,#16519,
#16520,#16521,#16522,#16523,#16524,#16525),.UNSPECIFIED.,.F.,.F.,(4,1,1,
1,1,1,1,1,4),(91.106186954104,91.207838164395,92.2053666988316,93.2028952332682,
94.2004237677048,95.1979523021414,96.195480836578,97.1930093710146,97.3893722612836),
 .UNSPECIFIED.);
#2186=B_SPLINE_CURVE_WITH_KNOTS('',3,(#16530,#16531,#16532,#16533,#16534,
#16535,#16536,#16537,#16538,#16539),.UNSPECIFIED.,.F.,.F.,(4,1,1,1,1,1,
1,4),(84.8230016469244,85.678691552565,86.6762200870016,87.6737486214382,
88.6712771558748,89.6688056903114,90.666334224748,91.106186954104),
 .UNSPECIFIED.);
#2187=B_SPLINE_CURVE_WITH_KNOTS('',3,(#16540,#16541,#16542,#16543,#16544,
#16545,#16546,#16547,#16548,#16549),.UNSPECIFIED.,.F.,.F.,(4,1,1,1,1,1,
1,4),(84.8230016469244,85.2226669577754,86.220195492212,87.2177240266486,
88.2152525610852,89.2127810955218,90.2103096299584,91.106186954104),
 .UNSPECIFIED.);
#2188=B_SPLINE_CURVE_WITH_KNOTS('',3,(#16554,#16555,#16556,#16557,#16558,
#16559,#16560,#16561,#16562,#16563,#16564),.UNSPECIFIED.,.F.,.F.,(4,1,1,
1,1,1,1,1,4),(78.5398163397448,78.6959918115088,79.6935203459454,80.691048880382,
81.6885774148186,82.6861059492552,83.6836344836918,84.6811630181284,84.8230016469244),
 .UNSPECIFIED.);
#2189=B_SPLINE_CURVE_WITH_KNOTS('',3,(#16565,#16566,#16567,#16568,#16569,
#16570,#16571,#16572,#16573,#16574),.UNSPECIFIED.,.F.,.F.,(4,1,1,1,1,1,
1,4),(78.5398163397448,79.2374957511558,80.2350242855924,81.232552820029,
82.2300813544656,83.2276098889022,84.2251384233388,84.8230016469244),
 .UNSPECIFIED.);
#2190=B_SPLINE_CURVE_WITH_KNOTS('',3,(#16579,#16580,#16581,#16582,#16583,
#16584,#16585,#16586,#16587,#16588),.UNSPECIFIED.,.F.,.F.,(4,1,1,1,1,1,
1,4),(72.2566310325652,72.7108206048892,73.7083491393258,74.7058776737624,
75.703406208199,76.7009347426356,77.6984632770722,78.5398163397448),
 .UNSPECIFIED.);
#2191=B_SPLINE_CURVE_WITH_KNOTS('',3,(#16589,#16590,#16591,#16592,#16593,
#16594,#16595,#16596,#16597,#16598),.UNSPECIFIED.,.F.,.F.,(4,1,1,1,1,1,
1,4),(72.2566310325652,73.2523245445362,74.2498530789728,75.2473816134094,
76.244910147846,77.2424386822826,78.2399672167192,78.5398163397448),
 .UNSPECIFIED.);
#2192=B_SPLINE_CURVE_WITH_KNOTS('',3,(#16603,#16604,#16605,#16606,#16607,
#16608,#16609,#16610,#16611,#16612),.UNSPECIFIED.,.F.,.F.,(4,1,1,1,1,1,
1,4),(65.9734457253856,66.7256493982696,67.7231779327062,68.7207064671428,
69.7182350015794,70.715763536016,71.7132920704526,72.2566310325652),
 .UNSPECIFIED.);
#2193=B_SPLINE_CURVE_WITH_KNOTS('',3,(#16613,#16614,#16615,#16616,#16617,
#16618,#16619,#16620,#16621,#16622,#16623),.UNSPECIFIED.,.F.,.F.,(4,1,1,
1,1,1,1,1,4),(65.9734457253856,66.26962480348,67.2671533379166,68.2646818723533,
69.2622104067898,70.2597389412264,71.257267475663,72.2547960100996,72.2566310325652),
 .UNSPECIFIED.);
#2194=B_SPLINE_CURVE_WITH_KNOTS('',3,(#16628,#16629,#16630,#16631,#16632,
#16633,#16634,#16635,#16636,#16637,#16638),.UNSPECIFIED.,.F.,.F.,(4,1,1,
1,1,1,1,1,4),(59.690260418206,59.7429496572134,60.74047819165,61.7380067260866,
62.7355352605232,63.7330637949598,64.7305923293964,65.728120863833,65.9734457253856),
 .UNSPECIFIED.);
#2195=B_SPLINE_CURVE_WITH_KNOTS('',3,(#16639,#16640,#16641,#16642,#16643,
#16644,#16645,#16646,#16647,#16648),.UNSPECIFIED.,.F.,.F.,(4,1,1,1,1,1,
1,4),(59.690260418206,60.2844535968604,61.281982131297,62.2795106657336,
63.2770392001703,64.2745677346068,65.2720962690434,65.9734457253856),
 .UNSPECIFIED.);
#2196=B_SPLINE_CURVE_WITH_KNOTS('',3,(#16653,#16654,#16655,#16656,#16657,
#16658,#16659,#16660,#16661,#16662),.UNSPECIFIED.,.F.,.F.,(4,1,1,1,1,1,
1,4),(53.4070751110264,53.7577784505938,54.7553069850304,55.752835519467,
56.7503640539036,57.7478925883402,58.7454211227768,59.690260418206),
 .UNSPECIFIED.);
#2197=B_SPLINE_CURVE_WITH_KNOTS('',3,(#16663,#16664,#16665,#16666,#16667,
#16668,#16669,#16670,#16671,#16672),.UNSPECIFIED.,.F.,.F.,(4,1,1,1,1,1,
1,4),(53.4070751110264,54.2992823902408,55.2968109246774,56.294339459114,
57.2918679935507,58.2893965279873,59.2869250624238,59.690260418206),
 .UNSPECIFIED.);
#2198=B_SPLINE_CURVE_WITH_KNOTS('',3,(#16677,#16678,#16679,#16680,#16681,
#16682,#16683,#16684,#16685,#16686),.UNSPECIFIED.,.F.,.F.,(4,1,1,1,1,1,
1,4),(47.1238898038469,47.7726072439742,48.7701357784108,49.7676643128474,
50.765192847284,51.7627213817206,52.7602499161572,53.4070751110264),
 .UNSPECIFIED.);
#2199=B_SPLINE_CURVE_WITH_KNOTS('',3,(#16687,#16688,#16689,#16690,#16691,
#16692,#16693,#16694,#16695,#16696,#16697),.UNSPECIFIED.,.F.,.F.,(4,1,1,
1,1,1,1,1,4),(47.1238898038469,47.3165826491847,48.3141111836213,49.3116397180578,
50.3091682524944,51.3066967869311,52.3042253213677,53.3017538558043,53.4070751110264),
 .UNSPECIFIED.);
#2200=B_SPLINE_CURVE_WITH_KNOTS('',3,(#16702,#16703,#16704,#16705,#16706,
#16707,#16708,#16709,#16710,#16711),.UNSPECIFIED.,.F.,.F.,(4,1,1,1,1,1,
1,4),(40.8407044966673,41.7874360373546,42.7849645717912,43.7824931062278,
44.7800216406644,45.777550175101,46.7750787095376,47.1238898038469),
 .UNSPECIFIED.);
#2201=B_SPLINE_CURVE_WITH_KNOTS('',3,(#16712,#16713,#16714,#16715,#16716,
#16717,#16718,#16719,#16720,#16721),.UNSPECIFIED.,.F.,.F.,(4,1,1,1,1,1,
1,4),(40.8407044966673,41.3314114425651,42.3289399770017,43.3264685114383,
44.3239970458749,45.3215255803115,46.3190541147481,47.1238898038469),
 .UNSPECIFIED.);
#2202=B_SPLINE_CURVE_WITH_KNOTS('',3,(#16726,#16727,#16728,#16729,#16730,
#16731,#16732,#16733,#16734,#16735,#16736),.UNSPECIFIED.,.F.,.F.,(4,1,1,
1,1,1,1,1,4),(34.5575191894876,34.8047362962984,35.802264830735,36.7997933651716,
37.7973218996082,38.7948504340448,39.7923789684814,40.789907502918,40.8407044966673),
 .UNSPECIFIED.);
#2203=B_SPLINE_CURVE_WITH_KNOTS('',3,(#16737,#16738,#16739,#16740,#16741,
#16742,#16743,#16744,#16745,#16746),.UNSPECIFIED.,.F.,.F.,(4,1,1,1,1,1,
1,4),(34.5575191894876,35.3462402359455,36.3437687703821,37.3412973048187,
38.3388258392553,39.3363543736919,40.3338829081285,40.8407044966673),
 .UNSPECIFIED.);
#2204=B_SPLINE_CURVE_WITH_KNOTS('',3,(#16751,#16752,#16753,#16754,#16755,
#16756,#16757,#16758,#16759,#16760),.UNSPECIFIED.,.F.,.F.,(4,1,1,1,1,1,
1,4),(28.2743338823081,28.8195650896788,29.8170936241154,30.814622158552,
31.8121506929886,32.8096792274252,33.8072077618618,34.5575191894876),
 .UNSPECIFIED.);
#2205=B_SPLINE_CURVE_WITH_KNOTS('',3,(#16761,#16762,#16763,#16764,#16765,
#16766,#16767,#16768,#16769,#16770,#16771),.UNSPECIFIED.,.F.,.F.,(4,1,1,
1,1,1,1,1,4),(28.2743338823081,28.3635404948893,29.3610690293259,30.3585975637625,
31.3561260981991,32.3536546326357,33.3511831670723,34.3487117015089,34.5575191894876),
 .UNSPECIFIED.);
#2206=B_SPLINE_CURVE_WITH_KNOTS('',3,(#16776,#16777,#16778,#16779,#16780,
#16781,#16782,#16783,#16784,#16785),.UNSPECIFIED.,.F.,.F.,(4,1,1,1,1,1,
1,4),(21.9911485751285,22.8343938830592,23.8319224174958,24.8294509519324,
25.826979486369,26.8245080208056,27.8220365552422,28.2743338823081),
 .UNSPECIFIED.);
#2207=B_SPLINE_CURVE_WITH_KNOTS('',3,(#16786,#16787,#16788,#16789,#16790,
#16791,#16792,#16793,#16794,#16795),.UNSPECIFIED.,.F.,.F.,(4,1,1,1,1,1,
1,4),(21.9911485751285,22.3783692882697,23.3758978227063,24.3734263571429,
25.3709548915795,26.3684834260161,27.3660119604527,28.2743338823081),
 .UNSPECIFIED.);
#2208=B_SPLINE_CURVE_WITH_KNOTS('',3,(#16801,#16802,#16803,#16804,#16805),
 .UNSPECIFIED.,.F.,.F.,(4,1,4),(14.3981410127769,15.3956695472135,15.7079632679489),
 .UNSPECIFIED.);
#2209=B_SPLINE_CURVE_WITH_KNOTS('',3,(#16808,#16809,#16810,#16811,#16812),
 .UNSPECIFIED.,.F.,.F.,(4,1,4),(13.8761928695311,14.8541656075664,15.7079632679489),
 .UNSPECIFIED.);
#2210=B_SPLINE_CURVE_WITH_KNOTS('',3,(#16818,#16819,#16820,#16821,#16822,
#16823,#16824,#16825,#16826,#16827,#16828,#16829,#16830,#16831,#16832,#16833,
#16834,#16835,#16836),.UNSPECIFIED.,.F.,.F.,(4,3,3,3,3,3,4),(95.5576018628658,
95.7627393059136,96.7602678403502,97.7577963747868,98.7553249092234,99.75285344366,
100.750381978097),.UNSPECIFIED.);
#2211=B_SPLINE_CURVE_WITH_KNOTS('',3,(#16840,#16841,#16842,#16843),
 .UNSPECIFIED.,.F.,.F.,(4,4),(-98.7357691128221,-98.0941628713862),
 .UNSPECIFIED.);
#2212=B_SPLINE_CURVE_WITH_KNOTS('',3,(#16847,#16848,#16849,#16850,#16851,
#16852,#16853,#16854,#16855,#16856,#16857,#16858,#16859,#16860,#16861,#16862,
#16863,#16864,#16865,#16866,#16867,#16868),.UNSPECIFIED.,.F.,.F.,(4,3,3,
3,3,3,3,4),(-98.0941628713862,-97.7577963747868,-96.7602678403502,-95.7627393059136,
-94.765210771477,-93.7676822370404,-92.7701537026038,-91.8109775642066),
 .UNSPECIFIED.);
#2213=B_SPLINE_CURVE_WITH_KNOTS('',3,(#16873,#16874,#16875,#16876,#16877,
#16878,#16879,#16880,#16881,#16882,#16883,#16884,#16885,#16886,#16887,#16888,
#16889,#16890,#16891,#16892,#16893,#16894),.UNSPECIFIED.,.F.,.F.,(4,3,3,
3,3,3,3,4),(89.2744165556863,89.777568099294,90.7750966337306,91.7726251681672,
92.7701537026038,93.7676822370404,94.765210771477,95.5576018628658),
 .UNSPECIFIED.);
#2214=B_SPLINE_CURVE_WITH_KNOTS('',3,(#16895,#16896,#16897,#16898,#16899,
#16900,#16901,#16902,#16903,#16904,#16905,#16906,#16907,#16908,#16909,#16910,
#16911,#16912,#16913,#16914,#16915,#16916,#16917,#16918,#16919),
 .UNSPECIFIED.,.F.,.F.,(4,3,3,3,3,3,3,3,4),(-91.8109775642066,-91.7726251681672,
-90.7750966337306,-89.777568099294,-88.7800395648574,-87.7825110304208,
-86.7849824959842,-85.7874539615476,-85.527792257027),.UNSPECIFIED.);
#2215=B_SPLINE_CURVE_WITH_KNOTS('',3,(#16924,#16925,#16926,#16927,#16928,
#16929,#16930,#16931,#16932,#16933,#16934,#16935,#16936,#16937,#16938,#16939,
#16940,#16941,#16942,#16943,#16944,#16945),.UNSPECIFIED.,.F.,.F.,(4,3,3,
3,3,3,3,4),(82.9912312485067,83.7923968926744,84.789925427111,85.7874539615476,
86.7849824959842,87.7825110304208,88.7800395648574,89.2744165556863),
 .UNSPECIFIED.);
#2216=B_SPLINE_CURVE_WITH_KNOTS('',3,(#16946,#16947,#16948,#16949,#16950,
#16951,#16952,#16953,#16954,#16955,#16956,#16957,#16958,#16959,#16960,#16961,
#16962,#16963,#16964,#16965,#16966,#16967),.UNSPECIFIED.,.F.,.F.,(4,3,3,
3,3,3,3,4),(-85.527792257027,-84.789925427111,-83.7923968926744,-82.7948683582378,
-81.7973398238012,-80.7998112893646,-79.802282754928,-79.2446069498474),
 .UNSPECIFIED.);
#2217=B_SPLINE_CURVE_WITH_KNOTS('',3,(#16972,#16973,#16974,#16975,#16976,
#16977,#16978,#16979,#16980,#16981,#16982,#16983,#16984,#16985,#16986,#16987,
#16988,#16989,#16990,#16991,#16992,#16993,#16994,#16995,#16996),
 .UNSPECIFIED.,.F.,.F.,(4,3,3,3,3,3,3,3,4),(76.7080459413271,76.8096971516182,
77.8072256860548,78.8047542204914,79.802282754928,80.7998112893646,81.7973398238012,
82.7948683582378,82.9912312485067),.UNSPECIFIED.);
#2218=B_SPLINE_CURVE_WITH_KNOTS('',3,(#16997,#16998,#16999,#17000,#17001,
#17002,#17003,#17004,#17005,#17006,#17007,#17008,#17009,#17010,#17011,#17012,
#17013,#17014,#17015,#17016,#17017,#17018),.UNSPECIFIED.,.F.,.F.,(4,3,3,
3,3,3,3,4),(-79.2446069498474,-78.8047542204914,-77.8072256860548,-76.8096971516182,
-75.8121686171816,-74.814640082745,-73.8171115483084,-72.9614216426678),
 .UNSPECIFIED.);
#2219=B_SPLINE_CURVE_WITH_KNOTS('',3,(#17023,#17024,#17025,#17026,#17027,
#17028,#17029,#17030,#17031,#17032,#17033,#17034,#17035,#17036,#17037,#17038,
#17039,#17040,#17041,#17042,#17043,#17044),.UNSPECIFIED.,.F.,.F.,(4,3,3,
3,3,3,3,4),(70.4248606341475,70.8245259449986,71.8220544794352,72.8195830138718,
73.8171115483084,74.814640082745,75.8121686171816,76.7080459413271),
 .UNSPECIFIED.);
#2220=B_SPLINE_CURVE_WITH_KNOTS('',3,(#17045,#17046,#17047,#17048,#17049,
#17050,#17051,#17052,#17053,#17054,#17055,#17056,#17057,#17058,#17059,#17060,
#17061,#17062,#17063,#17064,#17065,#17066,#17067,#17068,#17069),
 .UNSPECIFIED.,.F.,.F.,(4,3,3,3,3,3,3,3,4),(-72.9614216426678,-72.8195830138718,
-71.8220544794352,-70.8245259449986,-69.826997410562,-68.8294688761254,
-67.8319403416888,-66.8344118072522,-66.6782363354882),.UNSPECIFIED.);
#2221=B_SPLINE_CURVE_WITH_KNOTS('',3,(#17074,#17075,#17076,#17077,#17078,
#17079,#17080,#17081,#17082,#17083,#17084,#17085,#17086,#17087,#17088,#17089,
#17090,#17091,#17092,#17093,#17094,#17095),.UNSPECIFIED.,.F.,.F.,(4,3,3,
3,3,3,3,4),(64.1416753269679,64.839354738379,65.8368832728156,66.8344118072522,
67.8319403416888,68.8294688761254,69.826997410562,70.4248606341475),
 .UNSPECIFIED.);
#2222=B_SPLINE_CURVE_WITH_KNOTS('',3,(#17096,#17097,#17098,#17099,#17100,
#17101,#17102,#17103,#17104,#17105,#17106,#17107,#17108,#17109,#17110,#17111,
#17112,#17113,#17114,#17115,#17116,#17117),.UNSPECIFIED.,.F.,.F.,(4,3,3,
3,3,3,3,4),(-66.6782363354882,-65.8368832728156,-64.839354738379,-63.8418262039424,
-62.8442976695058,-61.8467691350692,-60.8492406006326,-60.3950510283086),
 .UNSPECIFIED.);
#2223=B_SPLINE_CURVE_WITH_KNOTS('',3,(#17122,#17123,#17124,#17125,#17126,
#17127,#17128,#17129,#17130,#17131,#17132,#17133,#17134,#17135,#17136,#17137,
#17138,#17139,#17140,#17141,#17142,#17143),.UNSPECIFIED.,.F.,.F.,(4,3,3,
3,3,3,3,4),(57.8584900197883,58.8541835317594,59.851712066196,60.8492406006326,
61.8467691350692,62.8442976695058,63.8418262039424,64.1416753269679),
 .UNSPECIFIED.);
#2224=B_SPLINE_CURVE_WITH_KNOTS('',3,(#17144,#17145,#17146,#17147,#17148,
#17149,#17150,#17151,#17152,#17153,#17154,#17155,#17156,#17157,#17158,#17159,
#17160,#17161,#17162,#17163,#17164,#17165),.UNSPECIFIED.,.F.,.F.,(4,3,3,
3,3,3,3,4),(-60.3950510283086,-59.851712066196,-58.8541835317594,-57.8566549973228,
-56.8591264628862,-55.8615979284496,-54.864069394013,-54.111865721129),
 .UNSPECIFIED.);
#2225=B_SPLINE_CURVE_WITH_KNOTS('',3,(#17170,#17171,#17172,#17173,#17174,
#17175,#17176,#17177,#17178,#17179,#17180,#17181,#17182,#17183,#17184,#17185,
#17186,#17187,#17188,#17189,#17190,#17191),.UNSPECIFIED.,.F.,.F.,(4,3,3,
3,3,3,3,4),(51.5753047126087,51.8714837907032,52.8690123251398,53.8665408595764,
54.864069394013,55.8615979284496,56.8591264628862,57.8584900197883),
 .UNSPECIFIED.);
#2226=B_SPLINE_CURVE_WITH_KNOTS('',3,(#17192,#17193,#17194,#17195,#17196,
#17197,#17198,#17199,#17200,#17201,#17202,#17203,#17204,#17205,#17206,#17207,
#17208,#17209,#17210,#17211,#17212,#17213,#17214,#17215,#17216),
 .UNSPECIFIED.,.F.,.F.,(4,3,3,3,3,3,3,3,4),(-54.111865721129,-53.8665408595764,
-52.8690123251398,-51.8714837907032,-50.8739552562666,-49.87642672183,-48.8788981873934,
-47.8813696529568,-47.8286804139494),.UNSPECIFIED.);
#2227=B_SPLINE_CURVE_WITH_KNOTS('',3,(#17221,#17222,#17223,#17224,#17225,
#17226,#17227,#17228,#17229,#17230,#17231,#17232,#17233,#17234,#17235,#17236,
#17237,#17238,#17239,#17240,#17241,#17242),.UNSPECIFIED.,.F.,.F.,(4,3,3,
3,3,3,3,4),(45.2921194054291,45.8863125840836,46.8838411185202,47.8813696529568,
48.8788981873934,49.87642672183,50.8739552562666,51.5753047126087),
 .UNSPECIFIED.);
#2228=B_SPLINE_CURVE_WITH_KNOTS('',3,(#17243,#17244,#17245,#17246,#17247,
#17248,#17249,#17250,#17251,#17252,#17253,#17254,#17255,#17256,#17257,#17258,
#17259,#17260,#17261,#17262,#17263,#17264),.UNSPECIFIED.,.F.,.F.,(4,3,3,
3,3,3,3,4),(-47.8286804139494,-46.8838411185202,-45.8863125840836,-44.888784049647,
-43.8912555152104,-42.8937269807738,-41.8961984463372,-41.5454951067699),
 .UNSPECIFIED.);
#2229=B_SPLINE_CURVE_WITH_KNOTS('',3,(#17269,#17270,#17271,#17272,#17273,
#17274,#17275,#17276,#17277,#17278,#17279,#17280,#17281,#17282,#17283,#17284,
#17285,#17286,#17287,#17288,#17289,#17290),.UNSPECIFIED.,.F.,.F.,(4,3,3,
3,3,3,3,4),(39.0089340982495,39.901141377464,40.8986699119006,41.8961984463372,
42.8937269807738,43.8912555152104,44.888784049647,45.2921194054291),
 .UNSPECIFIED.);
#2230=B_SPLINE_CURVE_WITH_KNOTS('',3,(#17291,#17292,#17293,#17294,#17295,
#17296,#17297,#17298,#17299,#17300,#17301,#17302,#17303,#17304,#17305,#17306,
#17307,#17308,#17309,#17310,#17311,#17312),.UNSPECIFIED.,.F.,.F.,(4,3,3,
3,3,3,3,4),(-41.5454951067699,-40.8986699119006,-39.901141377464,-38.9036128430274,
-37.9060843085908,-36.9085557741542,-35.9110272397176,-35.2623097995902),
 .UNSPECIFIED.);
#2231=B_SPLINE_CURVE_WITH_KNOTS('',3,(#17317,#17318,#17319,#17320,#17321,
#17322,#17323,#17324,#17325,#17326,#17327,#17328,#17329,#17330,#17331,#17332,
#17333,#17334,#17335,#17336,#17337,#17338,#17339,#17340,#17341),
 .UNSPECIFIED.,.F.,.F.,(4,3,3,3,3,3,3,3,4),(32.7257487910699,32.9184416364078,
33.9159701708444,34.913498705281,35.9110272397176,36.9085557741542,37.9060843085908,
38.9036128430274,39.0089340982495),.UNSPECIFIED.);
#2232=B_SPLINE_CURVE_WITH_KNOTS('',3,(#17342,#17343,#17344,#17345,#17346,
#17347,#17348,#17349,#17350,#17351,#17352,#17353,#17354,#17355,#17356,#17357,
#17358,#17359,#17360,#17361,#17362,#17363),.UNSPECIFIED.,.F.,.F.,(4,3,3,
3,3,3,3,4),(-35.2623097995902,-34.913498705281,-33.9159701708444,-32.9184416364078,
-31.9209131019712,-30.9233845675346,-29.925856033098,-28.9791244924107),
 .UNSPECIFIED.);
#2233=B_SPLINE_CURVE_WITH_KNOTS('',3,(#17368,#17369,#17370,#17371,#17372,
#17373,#17374,#17375,#17376,#17377,#17378,#17379,#17380,#17381,#17382,#17383,
#17384,#17385,#17386,#17387,#17388,#17389),.UNSPECIFIED.,.F.,.F.,(4,3,3,
3,3,3,3,4),(26.4425634838903,26.9332704297882,27.9307989642248,28.9283274986614,
29.925856033098,30.9233845675346,31.9209131019712,32.7257487910699),
 .UNSPECIFIED.);
#2234=B_SPLINE_CURVE_WITH_KNOTS('',3,(#17390,#17391,#17392,#17393,#17394,
#17395,#17396,#17397,#17398,#17399,#17400,#17401,#17402,#17403,#17404,#17405,
#17406,#17407,#17408,#17409,#17410,#17411,#17412,#17413,#17414),
 .UNSPECIFIED.,.F.,.F.,(4,3,3,3,3,3,3,3,4),(-28.9791244924107,-28.9283274986614,
-27.9307989642248,-26.9332704297882,-25.9357418953516,-24.938213360915,
-23.9406848264784,-22.9431562920418,-22.6959391852311),.UNSPECIFIED.);
#2235=B_SPLINE_CURVE_WITH_KNOTS('',3,(#17419,#17420,#17421,#17422,#17423,
#17424,#17425,#17426,#17427,#17428,#17429,#17430,#17431,#17432,#17433,#17434,
#17435,#17436,#17437,#17438,#17439,#17440),.UNSPECIFIED.,.F.,.F.,(4,3,3,
3,3,3,3,4),(20.1593781767108,20.9480992231686,21.9456277576052,22.9431562920418,
23.9406848264784,24.938213360915,25.9357418953516,26.4425634838903),
 .UNSPECIFIED.);
#2236=B_SPLINE_CURVE_WITH_KNOTS('',3,(#17441,#17442,#17443,#17444,#17445,
#17446,#17447,#17448,#17449,#17450,#17451,#17452,#17453,#17454,#17455,#17456,
#17457,#17458,#17459,#17460,#17461,#17462),.UNSPECIFIED.,.F.,.F.,(4,3,3,
3,3,3,3,4),(-22.6959391852311,-21.9456277576052,-20.9480992231686,-19.950570688732,
-18.9530421542954,-17.9555136198588,-16.9579850854222,-16.4127538780515),
 .UNSPECIFIED.);
#2237=B_SPLINE_CURVE_WITH_KNOTS('',3,(#17467,#17468,#17469,#17470,#17471,
#17472,#17473,#17474,#17475,#17476,#17477,#17478,#17479,#17480,#17481,#17482,
#17483,#17484,#17485,#17486,#17487,#17488,#17489,#17490,#17491),
 .UNSPECIFIED.,.F.,.F.,(4,3,3,3,3,3,3,3,4),(13.8761928695312,13.9653994821124,
14.962928016549,15.9604565509856,16.9579850854222,17.9555136198588,18.9530421542954,
19.950570688732,20.1593781767108),.UNSPECIFIED.);
#2238=B_SPLINE_CURVE_WITH_KNOTS('',3,(#17492,#17493,#17494,#17495,#17496,
#17497,#17498,#17499,#17500,#17501,#17502,#17503,#17504,#17505,#17506,#17507,
#17508,#17509,#17510,#17511,#17512,#17513),.UNSPECIFIED.,.F.,.F.,(4,3,3,
3,3,3,3,4),(-16.4127538780515,-15.9604565509856,-14.962928016549,-13.9653994821124,
-12.9678709476758,-11.9703424132392,-10.9728138788026,-10.1295685708719),
 .UNSPECIFIED.);
#2239=B_SPLINE_CURVE_WITH_KNOTS('',3,(#17519,#17520,#17521,#17522,#17523,
#17524,#17525,#17526,#17527,#17528,#17529,#17530,#17531),.UNSPECIFIED.,
 .F.,.F.,(4,3,3,3,4),(-3.84638326369234,-2.99258560330979,-1.9950570688732,
-0.997528534436597,0.),.UNSPECIFIED.);
#2240=B_SPLINE_CURVE_WITH_KNOTS('',3,(#17534,#17535,#17536,#17537,#17538,
#17539,#17540,#17541,#17542,#17543,#17544,#17545,#17546,#17547,#17548,#17549,
#17550,#17551,#17552),.UNSPECIFIED.,.F.,.F.,(4,3,3,3,3,3,4),(2.01461286527445,
2.9925856033098,3.9901141377464,4.987642672183,5.9851712066196,6.98269974105621,
7.59300756235157),.UNSPECIFIED.);
#2241=B_SPLINE_CURVE_WITH_KNOTS('',3,(#17558,#17559,#17560,#17561,#17562,
#17563),.UNSPECIFIED.,.F.,.F.,(4,1,1,4),(109.955742875643,110.61690491348,
111.614433447917,112.611961982353),.UNSPECIFIED.);
#2242=B_SPLINE_CURVE_WITH_KNOTS('',3,(#17566,#17567,#17568,#17569,#17570,
#17571,#17572),.UNSPECIFIED.,.F.,.F.,(4,1,1,1,4),(109.955742875643,110.16088031869,
111.158408853127,112.155937387564,113.133910125599),.UNSPECIFIED.);
#2243=B_SPLINE_CURVE_WITH_KNOTS('',3,(#17577,#17578,#17579,#17580,#17581,
#17582,#17583,#17584,#17585,#17586),.UNSPECIFIED.,.F.,.F.,(4,1,1,1,1,1,
1,4),(103.672557568463,104.63173370686,105.629262241297,106.626790775734,
107.62431931017,108.621847844607,109.619376379043,109.955742875643),
 .UNSPECIFIED.);
#2244=B_SPLINE_CURVE_WITH_KNOTS('',3,(#17587,#17588,#17589,#17590,#17591,
#17592,#17593,#17594,#17595,#17596),.UNSPECIFIED.,.F.,.F.,(4,1,1,1,1,1,
1,4),(103.672557568463,104.175709112071,105.173237646507,106.170766180944,
107.168294715381,108.165823249817,109.163351784254,109.955742875643),
 .UNSPECIFIED.);
#2245=B_SPLINE_CURVE_WITH_KNOTS('',3,(#17601,#17602,#17603,#17604,#17605,
#17606,#17607,#17608,#17609,#17610,#17611),.UNSPECIFIED.,.F.,.F.,(4,1,1,
1,1,1,1,1,4),(97.3893722612835,97.6490339658041,98.6465625002407,99.6440910346773,
100.641619569114,101.639148103551,102.636676637987,103.634205172424,103.672557568463),
 .UNSPECIFIED.);
#2246=B_SPLINE_CURVE_WITH_KNOTS('',3,(#17612,#17613,#17614,#17615,#17616,
#17617,#17618,#17619,#17620,#17621),.UNSPECIFIED.,.F.,.F.,(4,1,1,1,1,1,
1,4),(97.3893722612835,98.1905379054512,99.1880664398878,100.185594974324,
101.183123508761,102.180652043198,103.178180577634,103.672557568463),
 .UNSPECIFIED.);
#2247=B_SPLINE_CURVE_WITH_KNOTS('',3,(#17626,#17627,#17628,#17629,#17630,
#17631,#17632,#17633,#17634,#17635),.UNSPECIFIED.,.F.,.F.,(4,1,1,1,1,1,
1,4),(91.106186954104,91.6638627591845,92.6613912936211,93.6589198280577,
94.6564483624943,95.6539768969309,96.6515054313675,97.3893722612835),
 .UNSPECIFIED.);
#2248=B_SPLINE_CURVE_WITH_KNOTS('',3,(#17636,#17637,#17638,#17639,#17640,
#17641,#17642,#17643,#17644,#17645,#17646),.UNSPECIFIED.,.F.,.F.,(4,1,1,
1,1,1,1,1,4),(91.106186954104,91.207838164395,92.2053666988316,93.2028952332682,
94.2004237677048,95.1979523021414,96.195480836578,97.1930093710146,97.3893722612835),
 .UNSPECIFIED.);
#2249=B_SPLINE_CURVE_WITH_KNOTS('',3,(#17651,#17652,#17653,#17654,#17655,
#17656,#17657,#17658,#17659,#17660),.UNSPECIFIED.,.F.,.F.,(4,1,1,1,1,1,
1,4),(84.8230016469244,85.6786915525649,86.6762200870015,87.6737486214381,
88.6712771558747,89.6688056903113,90.6663342247479,91.106186954104),
 .UNSPECIFIED.);
#2250=B_SPLINE_CURVE_WITH_KNOTS('',3,(#17661,#17662,#17663,#17664,#17665,
#17666,#17667,#17668,#17669,#17670),.UNSPECIFIED.,.F.,.F.,(4,1,1,1,1,1,
1,4),(84.8230016469244,85.2226669577754,86.220195492212,87.2177240266486,
88.2152525610852,89.2127810955218,90.2103096299584,91.106186954104),
 .UNSPECIFIED.);
#2251=B_SPLINE_CURVE_WITH_KNOTS('',3,(#17675,#17676,#17677,#17678,#17679,
#17680,#17681,#17682,#17683,#17684,#17685),.UNSPECIFIED.,.F.,.F.,(4,1,1,
1,1,1,1,1,4),(78.5398163397448,78.6959918115087,79.6935203459453,80.6910488803819,
81.6885774148185,82.6861059492551,83.6836344836917,84.6811630181283,84.8230016469244),
 .UNSPECIFIED.);
#2252=B_SPLINE_CURVE_WITH_KNOTS('',3,(#17686,#17687,#17688,#17689,#17690,
#17691,#17692,#17693,#17694,#17695),.UNSPECIFIED.,.F.,.F.,(4,1,1,1,1,1,
1,4),(78.5398163397448,79.2374957511558,80.2350242855924,81.232552820029,
82.2300813544656,83.2276098889022,84.2251384233388,84.8230016469244),
 .UNSPECIFIED.);
#2253=B_SPLINE_CURVE_WITH_KNOTS('',3,(#17700,#17701,#17702,#17703,#17704,
#17705,#17706,#17707,#17708,#17709),.UNSPECIFIED.,.F.,.F.,(4,1,1,1,1,1,
1,4),(72.2566310325652,72.7108206048891,73.7083491393257,74.7058776737623,
75.7034062081989,76.7009347426355,77.6984632770721,78.5398163397448),
 .UNSPECIFIED.);
#2254=B_SPLINE_CURVE_WITH_KNOTS('',3,(#17710,#17711,#17712,#17713,#17714,
#17715,#17716,#17717,#17718,#17719),.UNSPECIFIED.,.F.,.F.,(4,1,1,1,1,1,
1,4),(72.2566310325652,73.2523245445362,74.2498530789728,75.2473816134094,
76.244910147846,77.2424386822826,78.2399672167192,78.5398163397448),
 .UNSPECIFIED.);
#2255=B_SPLINE_CURVE_WITH_KNOTS('',3,(#17724,#17725,#17726,#17727,#17728,
#17729,#17730,#17731,#17732,#17733),.UNSPECIFIED.,.F.,.F.,(4,1,1,1,1,1,
1,4),(65.9734457253856,66.7256493982695,67.7231779327061,68.7207064671427,
69.7182350015793,70.7157635360159,71.7132920704525,72.2566310325652),
 .UNSPECIFIED.);
#2256=B_SPLINE_CURVE_WITH_KNOTS('',3,(#17734,#17735,#17736,#17737,#17738,
#17739,#17740,#17741,#17742,#17743,#17744),.UNSPECIFIED.,.F.,.F.,(4,1,1,
1,1,1,1,1,4),(65.9734457253856,66.26962480348,67.2671533379166,68.2646818723532,
69.2622104067898,70.2597389412264,71.257267475663,72.2547960100996,72.2566310325652),
 .UNSPECIFIED.);
#2257=B_SPLINE_CURVE_WITH_KNOTS('',3,(#17749,#17750,#17751,#17752,#17753,
#17754,#17755,#17756,#17757,#17758,#17759),.UNSPECIFIED.,.F.,.F.,(4,1,1,
1,1,1,1,1,4),(59.690260418206,59.7429496572133,60.7404781916499,61.7380067260865,
62.7355352605231,63.7330637949597,64.7305923293963,65.7281208638329,65.9734457253856),
 .UNSPECIFIED.);
#2258=B_SPLINE_CURVE_WITH_KNOTS('',3,(#17760,#17761,#17762,#17763,#17764,
#17765,#17766,#17767,#17768,#17769),.UNSPECIFIED.,.F.,.F.,(4,1,1,1,1,1,
1,4),(59.690260418206,60.2844535968604,61.281982131297,62.2795106657336,
63.2770392001702,64.2745677346068,65.2720962690434,65.9734457253856),
 .UNSPECIFIED.);
#2259=B_SPLINE_CURVE_WITH_KNOTS('',3,(#17774,#17775,#17776,#17777,#17778,
#17779,#17780,#17781,#17782,#17783),.UNSPECIFIED.,.F.,.F.,(4,1,1,1,1,1,
1,4),(53.4070751110264,53.7577784505937,54.7553069850303,55.7528355194669,
56.7503640539035,57.7478925883401,58.7454211227767,59.690260418206),
 .UNSPECIFIED.);
#2260=B_SPLINE_CURVE_WITH_KNOTS('',3,(#17784,#17785,#17786,#17787,#17788,
#17789,#17790,#17791,#17792,#17793),.UNSPECIFIED.,.F.,.F.,(4,1,1,1,1,1,
1,4),(53.4070751110264,54.2992823902408,55.2968109246774,56.294339459114,
57.2918679935506,58.2893965279872,59.2869250624238,59.690260418206),
 .UNSPECIFIED.);
#2261=B_SPLINE_CURVE_WITH_KNOTS('',3,(#17798,#17799,#17800,#17801,#17802,
#17803,#17804,#17805,#17806,#17807),.UNSPECIFIED.,.F.,.F.,(4,1,1,1,1,1,
1,4),(47.1238898038468,47.7726072439741,48.7701357784107,49.7676643128473,
50.7651928472839,51.7627213817205,52.7602499161571,53.4070751110264),
 .UNSPECIFIED.);
#2262=B_SPLINE_CURVE_WITH_KNOTS('',3,(#17808,#17809,#17810,#17811,#17812,
#17813,#17814,#17815,#17816,#17817,#17818),.UNSPECIFIED.,.F.,.F.,(4,1,1,
1,1,1,1,1,4),(47.1238898038468,47.3165826491846,48.3141111836212,49.3116397180578,
50.3091682524944,51.306696786931,52.3042253213676,53.3017538558042,53.4070751110264),
 .UNSPECIFIED.);
#2263=B_SPLINE_CURVE_WITH_KNOTS('',3,(#17823,#17824,#17825,#17826,#17827,
#17828,#17829,#17830,#17831,#17832),.UNSPECIFIED.,.F.,.F.,(4,1,1,1,1,1,
1,4),(40.8407044966673,41.7874360373545,42.7849645717911,43.7824931062277,
44.7800216406643,45.7775501751009,46.7750787095375,47.1238898038468),
 .UNSPECIFIED.);
#2264=B_SPLINE_CURVE_WITH_KNOTS('',3,(#17833,#17834,#17835,#17836,#17837,
#17838,#17839,#17840,#17841,#17842),.UNSPECIFIED.,.F.,.F.,(4,1,1,1,1,1,
1,4),(40.8407044966673,41.331411442565,42.3289399770016,43.3264685114382,
44.3239970458748,45.3215255803114,46.319054114748,47.1238898038468),
 .UNSPECIFIED.);
#2265=B_SPLINE_CURVE_WITH_KNOTS('',3,(#17847,#17848,#17849,#17850,#17851,
#17852,#17853,#17854,#17855,#17856,#17857),.UNSPECIFIED.,.F.,.F.,(4,1,1,
1,1,1,1,1,4),(34.5575191894877,34.8047362962984,35.8022648307349,36.7997933651715,
37.7973218996081,38.7948504340447,39.7923789684813,40.7899075029179,40.8407044966673),
 .UNSPECIFIED.);
#2266=B_SPLINE_CURVE_WITH_KNOTS('',3,(#17858,#17859,#17860,#17861,#17862,
#17863,#17864,#17865,#17866,#17867),.UNSPECIFIED.,.F.,.F.,(4,1,1,1,1,1,
1,4),(34.5575191894876,35.3462402359454,36.343768770382,37.3412973048186,
38.3388258392552,39.3363543736918,40.3338829081284,40.8407044966673),
 .UNSPECIFIED.);
#2267=B_SPLINE_CURVE_WITH_KNOTS('',3,(#17872,#17873,#17874,#17875,#17876,
#17877,#17878,#17879,#17880,#17881),.UNSPECIFIED.,.F.,.F.,(4,1,1,1,1,1,
1,4),(28.2743338823081,28.8195650896787,29.8170936241154,30.8146221585519,
31.8121506929885,32.8096792274251,33.8072077618617,34.5575191894877),
 .UNSPECIFIED.);
#2268=B_SPLINE_CURVE_WITH_KNOTS('',3,(#17882,#17883,#17884,#17885,#17886,
#17887,#17888,#17889,#17890,#17891,#17892),.UNSPECIFIED.,.F.,.F.,(4,1,1,
1,1,1,1,1,4),(28.2743338823081,28.3635404948892,29.3610690293258,30.3585975637624,
31.356126098199,32.3536546326356,33.3511831670722,34.3487117015088,34.5575191894876),
 .UNSPECIFIED.);
#2269=B_SPLINE_CURVE_WITH_KNOTS('',3,(#17897,#17898,#17899,#17900,#17901,
#17902,#17903,#17904,#17905,#17906),.UNSPECIFIED.,.F.,.F.,(4,1,1,1,1,1,
1,4),(21.9911485751285,22.8343938830591,23.8319224174958,24.8294509519324,
25.8269794863689,26.8245080208056,27.8220365552421,28.2743338823081),
 .UNSPECIFIED.);
#2270=B_SPLINE_CURVE_WITH_KNOTS('',3,(#17907,#17908,#17909,#17910,#17911,
#17912,#17913,#17914,#17915,#17916),.UNSPECIFIED.,.F.,.F.,(4,1,1,1,1,1,
1,4),(21.9911485751284,22.3783692882696,23.3758978227062,24.3734263571428,
25.3709548915794,26.368483426016,27.3660119604526,28.2743338823081),
 .UNSPECIFIED.);
#2271=B_SPLINE_CURVE_WITH_KNOTS('',3,(#17922,#17923,#17924,#17925,#17926),
 .UNSPECIFIED.,.F.,.F.,(4,1,4),(14.3981410127768,15.3956695472134,15.7079632679489),
 .UNSPECIFIED.);
#2272=B_SPLINE_CURVE_WITH_KNOTS('',3,(#17929,#17930,#17931,#17932,#17933),
 .UNSPECIFIED.,.F.,.F.,(4,1,4),(13.876192869531,14.8541656075664,15.7079632679489),
 .UNSPECIFIED.);
#2273=B_SPLINE_CURVE_WITH_KNOTS('',3,(#17939,#17940,#17941,#17942),
 .UNSPECIFIED.,.F.,.F.,(4,4),(95.5573427486709,96.2647245007222),
 .UNSPECIFIED.);
#2274=B_SPLINE_CURVE_WITH_KNOTS('',3,(#17946,#17947,#17948,#17949,#17950,
#17951,#17952,#17953,#17954,#17955,#17956,#17957,#17958,#17959,#17960,#17961,
#17962,#17963,#17964),.UNSPECIFIED.,.F.,.F.,(4,2,2,2,3,2,2,2,4),(1.16162179993387,
1.25828720239456,1.35495260485525,1.45189083571687,1.54882906657849,1.64576729744011,
1.74270552830173,1.83937093076242,1.93603633322311),.UNSPECIFIED.);
#2275=B_SPLINE_CURVE_WITH_KNOTS('',3,(#17967,#17968,#17969,#17970,#17971,
#17972,#17973,#17974,#17975,#17976),.UNSPECIFIED.,.F.,.F.,(4,3,3,4),(-94.2477796076938,
-93.2874649800814,-92.2950451398677,-91.8135687061554),.UNSPECIFIED.);
#2276=B_SPLINE_CURVE_WITH_KNOTS('',3,(#17981,#17982,#17983,#17984,#17985,
#17986,#17987,#17988,#17989,#17990,#17991,#17992,#17993,#17994,#17995,#17996,
#17997,#17998,#17999,#18000,#18001,#18002,#18003,#18004,#18005),
 .UNSPECIFIED.,.F.,.F.,(4,3,3,3,3,3,3,3,4),(89.2741574414913,89.3177856192268,
90.3102054594404,91.3026252996541,92.2950451398677,93.2874649800813,94.279884820295,
95.2723046605086,95.5573427486709),.UNSPECIFIED.);
#2277=B_SPLINE_CURVE_WITH_KNOTS('',3,(#18006,#18007,#18008,#18009,#18010,
#18011,#18012,#18013,#18014,#18015,#18016,#18017,#18018,#18019,#18020,#18021,
#18022,#18023,#18024,#18025,#18026,#18027),.UNSPECIFIED.,.F.,.F.,(4,3,3,
3,3,3,3,4),(-91.8135687061554,-91.3026252996541,-90.3102054594405,-89.3177856192269,
-88.3253657790132,-87.3329459387996,-86.340526098586,-85.5303833989758),
 .UNSPECIFIED.);
#2278=B_SPLINE_CURVE_WITH_KNOTS('',3,(#18032,#18033,#18034,#18035,#18036,
#18037,#18038,#18039,#18040,#18041,#18042,#18043,#18044,#18045,#18046,#18047,
#18048,#18049,#18050,#18051,#18052,#18053),.UNSPECIFIED.,.F.,.F.,(4,3,3,
3,3,3,3,4),(82.9909721343117,83.363266577945,84.3556864181587,85.3481062583723,
86.3405260985859,87.3329459387996,88.3253657790132,89.2741574414913),
 .UNSPECIFIED.);
#2279=B_SPLINE_CURVE_WITH_KNOTS('',3,(#18054,#18055,#18056,#18057,#18058,
#18059,#18060,#18061,#18062,#18063,#18064,#18065,#18066,#18067,#18068,#18069,
#18070,#18071,#18072,#18073,#18074,#18075,#18076,#18077,#18078),
 .UNSPECIFIED.,.F.,.F.,(4,3,3,3,3,3,3,3,4),(-85.5303833989758,-85.3481062583723,
-84.3556864181587,-83.3632665779451,-82.3708467377314,-81.3784268975178,
-80.3860070573042,-79.3935872170905,-79.2471980917962),.UNSPECIFIED.);
#2280=B_SPLINE_CURVE_WITH_KNOTS('',3,(#18083,#18084,#18085,#18086,#18087,
#18088,#18089,#18090,#18091,#18092,#18093,#18094,#18095,#18096,#18097,#18098,
#18099,#18100,#18101,#18102,#18103,#18104),.UNSPECIFIED.,.F.,.F.,(4,3,3,
3,3,3,3,4),(76.7077868271321,77.4087475366632,78.4011673768769,79.3935872170905,
80.3860070573041,81.3784268975178,82.3708467377314,82.9909721343117),
 .UNSPECIFIED.);
#2281=B_SPLINE_CURVE_WITH_KNOTS('',3,(#18105,#18106,#18107,#18108,#18109,
#18110,#18111,#18112,#18113,#18114,#18115,#18116,#18117,#18118,#18119,#18120,
#18121,#18122,#18123,#18124,#18125,#18126),.UNSPECIFIED.,.F.,.F.,(4,3,3,
3,3,3,3,4),(-79.2471980917962,-78.4011673768769,-77.4087475366633,-76.4163276964496,
-75.423907856236,-74.4314880160224,-73.4390681758088,-72.9640127846167),
 .UNSPECIFIED.);
#2282=B_SPLINE_CURVE_WITH_KNOTS('',3,(#18131,#18132,#18133,#18134,#18135,
#18136,#18137,#18138,#18139,#18140,#18141,#18142,#18143,#18144,#18145,#18146,
#18147,#18148,#18149,#18150,#18151,#18152,#18153,#18154,#18155),
 .UNSPECIFIED.,.F.,.F.,(4,3,3,3,3,3,3,3,4),(70.4246015199525,70.4618086551678,
71.4542284953814,72.4466483355951,73.4390681758087,74.4314880160223,75.423907856236,
76.4163276964496,76.7077868271321),.UNSPECIFIED.);
#2283=B_SPLINE_CURVE_WITH_KNOTS('',3,(#18156,#18157,#18158,#18159,#18160,
#18161,#18162,#18163,#18164,#18165,#18166,#18167,#18168,#18169,#18170,#18171,
#18172,#18173,#18174,#18175,#18176,#18177),.UNSPECIFIED.,.F.,.F.,(4,3,3,
3,3,3,3,4),(-72.9640127846167,-72.4466483355951,-71.4542284953815,-70.4618086551678,
-69.4693888149542,-68.4769689747406,-67.4845491345269,-66.680827477437),
 .UNSPECIFIED.);
#2284=B_SPLINE_CURVE_WITH_KNOTS('',3,(#18182,#18183,#18184,#18185,#18186,
#18187,#18188,#18189,#18190,#18191,#18192,#18193,#18194,#18195,#18196,#18197,
#18198,#18199,#18200,#18201,#18202,#18203),.UNSPECIFIED.,.F.,.F.,(4,3,3,
3,3,3,3,4),(64.1414162127729,64.507289613886,65.4997094540997,66.4921292943133,
67.4845491345269,68.4769689747405,69.4693888149542,70.4246015199525),
 .UNSPECIFIED.);
#2285=B_SPLINE_CURVE_WITH_KNOTS('',3,(#18204,#18205,#18206,#18207,#18208,
#18209,#18210,#18211,#18212,#18213,#18214,#18215,#18216,#18217,#18218,#18219,
#18220,#18221,#18222,#18223,#18224,#18225,#18226,#18227,#18228),
 .UNSPECIFIED.,.F.,.F.,(4,3,3,3,3,3,3,3,4),(-66.680827477437,-66.4921292943133,
-65.4997094540997,-64.5072896138861,-63.5148697736724,-62.5224499334588,
-61.5300300932452,-60.5376102530315,-60.3976421702575),.UNSPECIFIED.);
#2286=B_SPLINE_CURVE_WITH_KNOTS('',3,(#18233,#18234,#18235,#18236,#18237,
#18238,#18239,#18240,#18241,#18242,#18243,#18244,#18245,#18246,#18247,#18248,
#18249,#18250,#18251,#18252,#18253,#18254),.UNSPECIFIED.,.F.,.F.,(4,3,3,
3,3,3,3,4),(57.8582309055933,58.5527705726042,59.5451904128179,60.5376102530315,
61.5300300932451,62.5224499334588,63.5148697736724,64.1414162127729),
 .UNSPECIFIED.);
#2287=B_SPLINE_CURVE_WITH_KNOTS('',3,(#18255,#18256,#18257,#18258,#18259,
#18260,#18261,#18262,#18263,#18264,#18265,#18266,#18267,#18268,#18269,#18270,
#18271,#18272,#18273,#18274,#18275,#18276),.UNSPECIFIED.,.F.,.F.,(4,3,3,
3,3,3,3,4),(-60.3976421702575,-59.5451904128179,-58.5527705726043,-57.5603507323906,
-56.567930892177,-55.5755110519634,-54.5830912117497,-54.1144568630778),
 .UNSPECIFIED.);
#2288=B_SPLINE_CURVE_WITH_KNOTS('',3,(#18281,#18282,#18283,#18284,#18285,
#18286,#18287,#18288,#18289,#18290,#18291,#18292,#18293,#18294,#18295,#18296,
#18297,#18298,#18299,#18300,#18301,#18302,#18303,#18304,#18305),
 .UNSPECIFIED.,.F.,.F.,(4,3,3,3,3,3,3,3,4),(51.5750455984138,51.6058316911088,
52.5982515313225,53.5906713715361,54.5830912117497,55.5755110519634,56.567930892177,
57.5603507323906,57.8582309055933),.UNSPECIFIED.);
#2289=B_SPLINE_CURVE_WITH_KNOTS('',3,(#18306,#18307,#18308,#18309,#18310,
#18311,#18312,#18313,#18314,#18315,#18316,#18317,#18318,#18319,#18320,#18321,
#18322,#18323,#18324,#18325,#18326,#18327),.UNSPECIFIED.,.F.,.F.,(4,3,3,
3,3,3,3,4),(-54.1144568630778,-53.5906713715361,-52.5982515313225,-51.6058316911089,
-50.6134118508952,-49.6209920106816,-48.6285721704679,-47.8312715558983),
 .UNSPECIFIED.);
#2290=B_SPLINE_CURVE_WITH_KNOTS('',3,(#18332,#18333,#18334,#18335,#18336,
#18337,#18338,#18339,#18340,#18341,#18342,#18343,#18344,#18345,#18346,#18347,
#18348,#18349,#18350,#18351,#18352,#18353),.UNSPECIFIED.,.F.,.F.,(4,3,3,
3,3,3,3,4),(45.2918602912342,45.651312649827,46.6437324900407,47.6361523302543,
48.6285721704679,49.6209920106816,50.6134118508952,51.5750455984138),
 .UNSPECIFIED.);
#2291=B_SPLINE_CURVE_WITH_KNOTS('',3,(#18354,#18355,#18356,#18357,#18358,
#18359,#18360,#18361,#18362,#18363,#18364,#18365,#18366,#18367,#18368,#18369,
#18370,#18371,#18372,#18373,#18374,#18375,#18376,#18377,#18378),
 .UNSPECIFIED.,.F.,.F.,(4,3,3,3,3,3,3,3,4),(-47.8312715558983,-47.6361523302543,
-46.6437324900407,-45.651312649827,-44.6588928096134,-43.6664729693998,
-42.6740531291861,-41.6816332889725,-41.5480862487187),.UNSPECIFIED.);
#2292=B_SPLINE_CURVE_WITH_KNOTS('',3,(#18383,#18384,#18385,#18386,#18387,
#18388,#18389,#18390,#18391,#18392,#18393,#18394,#18395,#18396,#18397,#18398,
#18399,#18400,#18401,#18402,#18403,#18404),.UNSPECIFIED.,.F.,.F.,(4,3,3,
3,3,3,3,4),(39.0086749840546,39.6967936085453,40.6892134487589,41.6816332889725,
42.6740531291861,43.6664729693998,44.6588928096134,45.2918602912342),
 .UNSPECIFIED.);
#2293=B_SPLINE_CURVE_WITH_KNOTS('',3,(#18405,#18406,#18407,#18408,#18409,
#18410,#18411,#18412,#18413,#18414,#18415,#18416,#18417,#18418,#18419,#18420,
#18421,#18422,#18423,#18424,#18425,#18426),.UNSPECIFIED.,.F.,.F.,(4,3,3,
3,3,3,3,4),(-41.5480862487187,-40.6892134487589,-39.6967936085453,-38.7043737683316,
-37.711953928118,-36.7195340879044,-35.7271142476907,-35.2649009415391),
 .UNSPECIFIED.);
#2294=B_SPLINE_CURVE_WITH_KNOTS('',3,(#18431,#18432,#18433,#18434,#18435,
#18436,#18437,#18438,#18439,#18440,#18441,#18442,#18443,#18444,#18445,#18446,
#18447,#18448,#18449,#18450,#18451,#18452,#18453,#18454,#18455),
 .UNSPECIFIED.,.F.,.F.,(4,3,3,3,3,3,3,3,4),(32.725489676875,32.7498547270498,
33.7422745672635,34.7346944074771,35.7271142476907,36.7195340879043,37.711953928118,
38.7043737683316,39.0086749840546),.UNSPECIFIED.);
#2295=B_SPLINE_CURVE_WITH_KNOTS('',3,(#18456,#18457,#18458,#18459,#18460,
#18461,#18462,#18463,#18464,#18465,#18466,#18467,#18468,#18469,#18470,#18471,
#18472,#18473,#18474,#18475,#18476,#18477),.UNSPECIFIED.,.F.,.F.,(4,3,3,
3,3,3,3,4),(-35.2649009415391,-34.7346944074771,-33.7422745672635,-32.7498547270498,
-31.7574348868362,-30.7650150466226,-29.7725952064089,-28.9817156343595),
 .UNSPECIFIED.);
#2296=B_SPLINE_CURVE_WITH_KNOTS('',3,(#18482,#18483,#18484,#18485,#18486,
#18487,#18488,#18489,#18490,#18491,#18492,#18493,#18494,#18495,#18496,#18497,
#18498,#18499,#18500,#18501,#18502,#18503),.UNSPECIFIED.,.F.,.F.,(4,3,3,
3,3,3,3,4),(26.4423043696954,26.795335685768,27.7877555259817,28.7801753661953,
29.7725952064089,30.7650150466226,31.7574348868362,32.725489676875),
 .UNSPECIFIED.);
#2297=B_SPLINE_CURVE_WITH_KNOTS('',3,(#18504,#18505,#18506,#18507,#18508,
#18509,#18510,#18511,#18512,#18513,#18514,#18515,#18516,#18517,#18518,#18519,
#18520,#18521,#18522,#18523,#18524,#18525,#18526,#18527,#18528),
 .UNSPECIFIED.,.F.,.F.,(4,3,3,3,3,3,3,3,4),(-28.9817156343595,-28.7801753661953,
-27.7877555259817,-26.7953356857681,-25.8029158455544,-24.8104960053408,
-23.8180761651272,-22.8256563249135,-22.6985303271799),.UNSPECIFIED.);
#2298=B_SPLINE_CURVE_WITH_KNOTS('',3,(#18533,#18534,#18535,#18536,#18537,
#18538,#18539,#18540,#18541,#18542,#18543,#18544,#18545,#18546,#18547,#18548,
#18549,#18550,#18551,#18552,#18553,#18554),.UNSPECIFIED.,.F.,.F.,(4,3,3,
3,3,3,3,4),(20.1591190625158,20.8408166444862,21.8332364846999,22.8256563249135,
23.8180761651271,24.8104960053408,25.8029158455544,26.4423043696954),
 .UNSPECIFIED.);
#2299=B_SPLINE_CURVE_WITH_KNOTS('',3,(#18555,#18556,#18557,#18558,#18559,
#18560,#18561,#18562,#18563,#18564,#18565,#18566,#18567,#18568,#18569,#18570,
#18571,#18572,#18573,#18574,#18575,#18576),.UNSPECIFIED.,.F.,.F.,(4,3,3,
3,3,3,3,4),(-22.6985303271799,-21.8332364846999,-20.8408166444863,-19.8483968042726,
-18.855976964059,-17.8635571238454,-16.8711372836317,-16.4153450200003),
 .UNSPECIFIED.);
#2300=B_SPLINE_CURVE_WITH_KNOTS('',3,(#18581,#18582,#18583,#18584,#18585,
#18586,#18587,#18588,#18589,#18590,#18591,#18592,#18593,#18594,#18595,#18596,
#18597,#18598,#18599,#18600,#18601,#18602,#18603,#18604,#18605),
 .UNSPECIFIED.,.F.,.F.,(4,3,3,3,3,3,3,3,4),(13.8759337553362,13.8938777629908,
14.8862976032045,15.8787174434181,16.8711372836317,17.8635571238454,18.855976964059,
19.8483968042726,20.1591190625158),.UNSPECIFIED.);
#2301=B_SPLINE_CURVE_WITH_KNOTS('',3,(#18606,#18607,#18608,#18609,#18610,
#18611,#18612,#18613,#18614,#18615,#18616,#18617,#18618,#18619,#18620,#18621,
#18622,#18623,#18624,#18625,#18626,#18627),.UNSPECIFIED.,.F.,.F.,(4,3,3,
3,3,3,3,4),(-16.4153450200003,-15.8787174434181,-14.8862976032045,-13.8938777629908,
-12.9014579227772,-11.9090380825636,-10.9166182423499,-10.1321597128207),
 .UNSPECIFIED.);
#2302=B_SPLINE_CURVE_WITH_KNOTS('',3,(#18633,#18634,#18635,#18636,#18637,
#18638,#18639,#18640,#18641,#18642,#18643,#18644,#18645),.UNSPECIFIED.,
 .F.,.F.,(4,3,3,3,4),(-3.84897440564114,-2.9772595206409,-1.98483968042726,
-0.992419840213632,0.),.UNSPECIFIED.);
#2303=B_SPLINE_CURVE_WITH_KNOTS('',3,(#18648,#18649,#18650,#18651,#18652,
#18653,#18654,#18655,#18656,#18657,#18658,#18659,#18660,#18661,#18662,#18663,
#18664,#18665,#18666),.UNSPECIFIED.,.F.,.F.,(4,3,3,3,3,3,4),(2.01694489302841,
2.97725952064089,3.96967936085453,4.96209920106816,5.95451904128179,6.94693888149542,
7.59274844815661),.UNSPECIFIED.);
#2304=B_SPLINE_CURVE_WITH_KNOTS('',3,(#18672,#18673,#18674,#18675),
 .UNSPECIFIED.,.F.,.F.,(4,4),(95.5573427486709,96.2647245007222),
 .UNSPECIFIED.);
#2305=B_SPLINE_CURVE_WITH_KNOTS('',3,(#18679,#18680,#18681,#18682,#18683,
#18684,#18685,#18686,#18687,#18688,#18689,#18690,#18691,#18692,#18693,#18694,
#18695,#18696,#18697),.UNSPECIFIED.,.F.,.F.,(4,2,2,2,3,2,2,2,4),(1.16162179993387,
1.25828720239456,1.35495260485525,1.45189083571687,1.54882906657849,1.64576729744011,
1.74270552830173,1.83937093076242,1.93603633322311),.UNSPECIFIED.);
#2306=B_SPLINE_CURVE_WITH_KNOTS('',3,(#18700,#18701,#18702,#18703,#18704,
#18705,#18706,#18707,#18708,#18709),.UNSPECIFIED.,.F.,.F.,(4,3,3,4),(-94.2477796076938,
-93.2874649800814,-92.2950451398677,-91.8135687061554),.UNSPECIFIED.);
#2307=B_SPLINE_CURVE_WITH_KNOTS('',3,(#18714,#18715,#18716,#18717,#18718,
#18719,#18720,#18721,#18722,#18723,#18724,#18725,#18726,#18727,#18728,#18729,
#18730,#18731,#18732,#18733,#18734,#18735,#18736,#18737,#18738),
 .UNSPECIFIED.,.F.,.F.,(4,3,3,3,3,3,3,3,4),(89.2741574414913,89.3177856192268,
90.3102054594404,91.3026252996541,92.2950451398677,93.2874649800813,94.279884820295,
95.2723046605086,95.5573427486709),.UNSPECIFIED.);
#2308=B_SPLINE_CURVE_WITH_KNOTS('',3,(#18739,#18740,#18741,#18742,#18743,
#18744,#18745,#18746,#18747,#18748,#18749,#18750,#18751,#18752,#18753,#18754,
#18755,#18756,#18757,#18758,#18759,#18760),.UNSPECIFIED.,.F.,.F.,(4,3,3,
3,3,3,3,4),(-91.8135687061554,-91.3026252996541,-90.3102054594405,-89.3177856192269,
-88.3253657790132,-87.3329459387996,-86.340526098586,-85.5303833989758),
 .UNSPECIFIED.);
#2309=B_SPLINE_CURVE_WITH_KNOTS('',3,(#18765,#18766,#18767,#18768,#18769,
#18770,#18771,#18772,#18773,#18774,#18775,#18776,#18777,#18778,#18779,#18780,
#18781,#18782,#18783,#18784,#18785,#18786),.UNSPECIFIED.,.F.,.F.,(4,3,3,
3,3,3,3,4),(82.9909721343117,83.363266577945,84.3556864181587,85.3481062583723,
86.3405260985859,87.3329459387996,88.3253657790132,89.2741574414913),
 .UNSPECIFIED.);
#2310=B_SPLINE_CURVE_WITH_KNOTS('',3,(#18787,#18788,#18789,#18790,#18791,
#18792,#18793,#18794,#18795,#18796,#18797,#18798,#18799,#18800,#18801,#18802,
#18803,#18804,#18805,#18806,#18807,#18808,#18809,#18810,#18811),
 .UNSPECIFIED.,.F.,.F.,(4,3,3,3,3,3,3,3,4),(-85.5303833989758,-85.3481062583723,
-84.3556864181587,-83.3632665779451,-82.3708467377314,-81.3784268975178,
-80.3860070573042,-79.3935872170905,-79.2471980917962),.UNSPECIFIED.);
#2311=B_SPLINE_CURVE_WITH_KNOTS('',3,(#18816,#18817,#18818,#18819,#18820,
#18821,#18822,#18823,#18824,#18825,#18826,#18827,#18828,#18829,#18830,#18831,
#18832,#18833,#18834,#18835,#18836,#18837),.UNSPECIFIED.,.F.,.F.,(4,3,3,
3,3,3,3,4),(76.7077868271321,77.4087475366632,78.4011673768769,79.3935872170905,
80.3860070573041,81.3784268975178,82.3708467377314,82.9909721343117),
 .UNSPECIFIED.);
#2312=B_SPLINE_CURVE_WITH_KNOTS('',3,(#18838,#18839,#18840,#18841,#18842,
#18843,#18844,#18845,#18846,#18847,#18848,#18849,#18850,#18851,#18852,#18853,
#18854,#18855,#18856,#18857,#18858,#18859),.UNSPECIFIED.,.F.,.F.,(4,3,3,
3,3,3,3,4),(-79.2471980917962,-78.4011673768769,-77.4087475366633,-76.4163276964496,
-75.423907856236,-74.4314880160224,-73.4390681758088,-72.9640127846167),
 .UNSPECIFIED.);
#2313=B_SPLINE_CURVE_WITH_KNOTS('',3,(#18864,#18865,#18866,#18867,#18868,
#18869,#18870,#18871,#18872,#18873,#18874,#18875,#18876,#18877,#18878,#18879,
#18880,#18881,#18882,#18883,#18884,#18885,#18886,#18887,#18888),
 .UNSPECIFIED.,.F.,.F.,(4,3,3,3,3,3,3,3,4),(70.4246015199525,70.4618086551678,
71.4542284953814,72.4466483355951,73.4390681758087,74.4314880160223,75.423907856236,
76.4163276964496,76.7077868271321),.UNSPECIFIED.);
#2314=B_SPLINE_CURVE_WITH_KNOTS('',3,(#18889,#18890,#18891,#18892,#18893,
#18894,#18895,#18896,#18897,#18898,#18899,#18900,#18901,#18902,#18903,#18904,
#18905,#18906,#18907,#18908,#18909,#18910),.UNSPECIFIED.,.F.,.F.,(4,3,3,
3,3,3,3,4),(-72.9640127846167,-72.4466483355951,-71.4542284953815,-70.4618086551678,
-69.4693888149542,-68.4769689747406,-67.4845491345269,-66.680827477437),
 .UNSPECIFIED.);
#2315=B_SPLINE_CURVE_WITH_KNOTS('',3,(#18915,#18916,#18917,#18918,#18919,
#18920,#18921,#18922,#18923,#18924,#18925,#18926,#18927,#18928,#18929,#18930,
#18931,#18932,#18933,#18934,#18935,#18936),.UNSPECIFIED.,.F.,.F.,(4,3,3,
3,3,3,3,4),(64.1414162127729,64.507289613886,65.4997094540997,66.4921292943133,
67.4845491345269,68.4769689747405,69.4693888149542,70.4246015199525),
 .UNSPECIFIED.);
#2316=B_SPLINE_CURVE_WITH_KNOTS('',3,(#18937,#18938,#18939,#18940,#18941,
#18942,#18943,#18944,#18945,#18946,#18947,#18948,#18949,#18950,#18951,#18952,
#18953,#18954,#18955,#18956,#18957,#18958,#18959,#18960,#18961),
 .UNSPECIFIED.,.F.,.F.,(4,3,3,3,3,3,3,3,4),(-66.680827477437,-66.4921292943133,
-65.4997094540997,-64.5072896138861,-63.5148697736724,-62.5224499334588,
-61.5300300932452,-60.5376102530315,-60.3976421702575),.UNSPECIFIED.);
#2317=B_SPLINE_CURVE_WITH_KNOTS('',3,(#18966,#18967,#18968,#18969,#18970,
#18971,#18972,#18973,#18974,#18975,#18976,#18977,#18978,#18979,#18980,#18981,
#18982,#18983,#18984,#18985,#18986,#18987),.UNSPECIFIED.,.F.,.F.,(4,3,3,
3,3,3,3,4),(57.8582309055933,58.5527705726042,59.5451904128179,60.5376102530315,
61.5300300932451,62.5224499334588,63.5148697736724,64.1414162127729),
 .UNSPECIFIED.);
#2318=B_SPLINE_CURVE_WITH_KNOTS('',3,(#18988,#18989,#18990,#18991,#18992,
#18993,#18994,#18995,#18996,#18997,#18998,#18999,#19000,#19001,#19002,#19003,
#19004,#19005,#19006,#19007,#19008,#19009),.UNSPECIFIED.,.F.,.F.,(4,3,3,
3,3,3,3,4),(-60.3976421702575,-59.5451904128179,-58.5527705726043,-57.5603507323906,
-56.567930892177,-55.5755110519634,-54.5830912117497,-54.1144568630778),
 .UNSPECIFIED.);
#2319=B_SPLINE_CURVE_WITH_KNOTS('',3,(#19014,#19015,#19016,#19017,#19018,
#19019,#19020,#19021,#19022,#19023,#19024,#19025,#19026,#19027,#19028,#19029,
#19030,#19031,#19032,#19033,#19034,#19035,#19036,#19037,#19038),
 .UNSPECIFIED.,.F.,.F.,(4,3,3,3,3,3,3,3,4),(51.5750455984138,51.6058316911088,
52.5982515313225,53.5906713715361,54.5830912117497,55.5755110519634,56.567930892177,
57.5603507323906,57.8582309055933),.UNSPECIFIED.);
#2320=B_SPLINE_CURVE_WITH_KNOTS('',3,(#19039,#19040,#19041,#19042,#19043,
#19044,#19045,#19046,#19047,#19048,#19049,#19050,#19051,#19052,#19053,#19054,
#19055,#19056,#19057,#19058,#19059,#19060),.UNSPECIFIED.,.F.,.F.,(4,3,3,
3,3,3,3,4),(-54.1144568630778,-53.5906713715361,-52.5982515313225,-51.6058316911089,
-50.6134118508952,-49.6209920106816,-48.6285721704679,-47.8312715558983),
 .UNSPECIFIED.);
#2321=B_SPLINE_CURVE_WITH_KNOTS('',3,(#19065,#19066,#19067,#19068,#19069,
#19070,#19071,#19072,#19073,#19074,#19075,#19076,#19077,#19078,#19079,#19080,
#19081,#19082,#19083,#19084,#19085,#19086),.UNSPECIFIED.,.F.,.F.,(4,3,3,
3,3,3,3,4),(45.2918602912342,45.651312649827,46.6437324900407,47.6361523302543,
48.6285721704679,49.6209920106816,50.6134118508952,51.5750455984138),
 .UNSPECIFIED.);
#2322=B_SPLINE_CURVE_WITH_KNOTS('',3,(#19087,#19088,#19089,#19090,#19091,
#19092,#19093,#19094,#19095,#19096,#19097,#19098,#19099,#19100,#19101,#19102,
#19103,#19104,#19105,#19106,#19107,#19108,#19109,#19110,#19111),
 .UNSPECIFIED.,.F.,.F.,(4,3,3,3,3,3,3,3,4),(-47.8312715558983,-47.6361523302543,
-46.6437324900407,-45.651312649827,-44.6588928096134,-43.6664729693998,
-42.6740531291861,-41.6816332889725,-41.5480862487187),.UNSPECIFIED.);
#2323=B_SPLINE_CURVE_WITH_KNOTS('',3,(#19116,#19117,#19118,#19119,#19120,
#19121,#19122,#19123,#19124,#19125,#19126,#19127,#19128,#19129,#19130,#19131,
#19132,#19133,#19134,#19135,#19136,#19137),.UNSPECIFIED.,.F.,.F.,(4,3,3,
3,3,3,3,4),(39.0086749840546,39.6967936085453,40.6892134487589,41.6816332889725,
42.6740531291861,43.6664729693998,44.6588928096134,45.2918602912342),
 .UNSPECIFIED.);
#2324=B_SPLINE_CURVE_WITH_KNOTS('',3,(#19138,#19139,#19140,#19141,#19142,
#19143,#19144,#19145,#19146,#19147,#19148,#19149,#19150,#19151,#19152,#19153,
#19154,#19155,#19156,#19157,#19158,#19159),.UNSPECIFIED.,.F.,.F.,(4,3,3,
3,3,3,3,4),(-41.5480862487187,-40.6892134487589,-39.6967936085453,-38.7043737683316,
-37.711953928118,-36.7195340879044,-35.7271142476907,-35.2649009415391),
 .UNSPECIFIED.);
#2325=B_SPLINE_CURVE_WITH_KNOTS('',3,(#19164,#19165,#19166,#19167,#19168,
#19169,#19170,#19171,#19172,#19173,#19174,#19175,#19176,#19177,#19178,#19179,
#19180,#19181,#19182,#19183,#19184,#19185,#19186,#19187,#19188),
 .UNSPECIFIED.,.F.,.F.,(4,3,3,3,3,3,3,3,4),(32.725489676875,32.7498547270498,
33.7422745672635,34.7346944074771,35.7271142476907,36.7195340879043,37.711953928118,
38.7043737683316,39.0086749840546),.UNSPECIFIED.);
#2326=B_SPLINE_CURVE_WITH_KNOTS('',3,(#19189,#19190,#19191,#19192,#19193,
#19194,#19195,#19196,#19197,#19198,#19199,#19200,#19201,#19202,#19203,#19204,
#19205,#19206,#19207,#19208,#19209,#19210),.UNSPECIFIED.,.F.,.F.,(4,3,3,
3,3,3,3,4),(-35.2649009415391,-34.7346944074771,-33.7422745672635,-32.7498547270498,
-31.7574348868362,-30.7650150466226,-29.7725952064089,-28.9817156343595),
 .UNSPECIFIED.);
#2327=B_SPLINE_CURVE_WITH_KNOTS('',3,(#19215,#19216,#19217,#19218,#19219,
#19220,#19221,#19222,#19223,#19224,#19225,#19226,#19227,#19228,#19229,#19230,
#19231,#19232,#19233,#19234,#19235,#19236),.UNSPECIFIED.,.F.,.F.,(4,3,3,
3,3,3,3,4),(26.4423043696954,26.795335685768,27.7877555259817,28.7801753661953,
29.7725952064089,30.7650150466226,31.7574348868362,32.725489676875),
 .UNSPECIFIED.);
#2328=B_SPLINE_CURVE_WITH_KNOTS('',3,(#19237,#19238,#19239,#19240,#19241,
#19242,#19243,#19244,#19245,#19246,#19247,#19248,#19249,#19250,#19251,#19252,
#19253,#19254,#19255,#19256,#19257,#19258,#19259,#19260,#19261),
 .UNSPECIFIED.,.F.,.F.,(4,3,3,3,3,3,3,3,4),(-28.9817156343595,-28.7801753661953,
-27.7877555259817,-26.7953356857681,-25.8029158455544,-24.8104960053408,
-23.8180761651272,-22.8256563249135,-22.6985303271799),.UNSPECIFIED.);
#2329=B_SPLINE_CURVE_WITH_KNOTS('',3,(#19266,#19267,#19268,#19269,#19270,
#19271,#19272,#19273,#19274,#19275,#19276,#19277,#19278,#19279,#19280,#19281,
#19282,#19283,#19284,#19285,#19286,#19287),.UNSPECIFIED.,.F.,.F.,(4,3,3,
3,3,3,3,4),(20.1591190625158,20.8408166444862,21.8332364846999,22.8256563249135,
23.8180761651271,24.8104960053408,25.8029158455544,26.4423043696954),
 .UNSPECIFIED.);
#2330=B_SPLINE_CURVE_WITH_KNOTS('',3,(#19288,#19289,#19290,#19291,#19292,
#19293,#19294,#19295,#19296,#19297,#19298,#19299,#19300,#19301,#19302,#19303,
#19304,#19305,#19306,#19307,#19308,#19309),.UNSPECIFIED.,.F.,.F.,(4,3,3,
3,3,3,3,4),(-22.6985303271799,-21.8332364846999,-20.8408166444863,-19.8483968042726,
-18.855976964059,-17.8635571238454,-16.8711372836317,-16.4153450200003),
 .UNSPECIFIED.);
#2331=B_SPLINE_CURVE_WITH_KNOTS('',3,(#19314,#19315,#19316,#19317,#19318,
#19319,#19320,#19321,#19322,#19323,#19324,#19325,#19326,#19327,#19328,#19329,
#19330,#19331,#19332,#19333,#19334,#19335,#19336,#19337,#19338),
 .UNSPECIFIED.,.F.,.F.,(4,3,3,3,3,3,3,3,4),(13.8759337553362,13.8938777629908,
14.8862976032045,15.8787174434181,16.8711372836317,17.8635571238454,18.855976964059,
19.8483968042726,20.1591190625158),.UNSPECIFIED.);
#2332=B_SPLINE_CURVE_WITH_KNOTS('',3,(#19339,#19340,#19341,#19342,#19343,
#19344,#19345,#19346,#19347,#19348,#19349,#19350,#19351,#19352,#19353,#19354,
#19355,#19356,#19357,#19358,#19359,#19360),.UNSPECIFIED.,.F.,.F.,(4,3,3,
3,3,3,3,4),(-16.4153450200003,-15.8787174434181,-14.8862976032045,-13.8938777629908,
-12.9014579227772,-11.9090380825636,-10.9166182423499,-10.1321597128207),
 .UNSPECIFIED.);
#2333=B_SPLINE_CURVE_WITH_KNOTS('',3,(#19366,#19367,#19368,#19369,#19370,
#19371,#19372,#19373,#19374,#19375,#19376,#19377,#19378),.UNSPECIFIED.,
 .F.,.F.,(4,3,3,3,4),(-3.84897440564114,-2.9772595206409,-1.98483968042726,
-0.992419840213632,0.),.UNSPECIFIED.);
#2334=B_SPLINE_CURVE_WITH_KNOTS('',3,(#19381,#19382,#19383,#19384,#19385,
#19386,#19387,#19388,#19389,#19390,#19391,#19392,#19393,#19394,#19395,#19396,
#19397,#19398,#19399),.UNSPECIFIED.,.F.,.F.,(4,3,3,3,3,3,4),(2.01694489302841,
2.97725952064089,3.96967936085453,4.96209920106816,5.95451904128179,6.94693888149542,
7.59274844815661),.UNSPECIFIED.);
#2335=B_SPLINE_CURVE_WITH_KNOTS('',3,(#19405,#19406,#19407,#19408,#19409,
#19410,#19411,#19412),.UNSPECIFIED.,.F.,.F.,(4,1,1,1,1,4),(103.672557568463,
104.154034002175,105.146453842389,106.138873682603,107.131293522816,108.12371336303),
 .UNSPECIFIED.);
#2336=B_SPLINE_CURVE_WITH_KNOTS('',3,(#19415,#19416,#19417,#19418,#19419,
#19420,#19421,#19422,#19423),.UNSPECIFIED.,.F.,.F.,(4,1,1,1,1,1,4),(103.672557568463,
103.716185746199,104.708605586412,105.701025426626,106.693445266839,107.685865107053,
108.646179734666),.UNSPECIFIED.);
#2337=B_SPLINE_CURVE_WITH_KNOTS('',3,(#19428,#19429,#19430,#19431,#19432,
#19433,#19434,#19435,#19436,#19437),.UNSPECIFIED.,.F.,.F.,(4,1,1,1,1,1,
1,4),(97.3893722612836,98.1995149608937,99.1919348011073,100.184354641321,
101.176774481535,102.169194321748,103.161614161962,103.672557568463),
 .UNSPECIFIED.);
#2338=B_SPLINE_CURVE_WITH_KNOTS('',3,(#19438,#19439,#19440,#19441,#19442,
#19443,#19444,#19445,#19446,#19447),.UNSPECIFIED.,.F.,.F.,(4,1,1,1,1,1,
1,4),(97.3893722612836,97.7616667049168,98.7540865451304,99.7465063853441,
100.738926225558,101.731346065771,102.723765905985,103.672557568463),
 .UNSPECIFIED.);
#2339=B_SPLINE_CURVE_WITH_KNOTS('',3,(#19452,#19453,#19454,#19455,#19456,
#19457,#19458,#19459,#19460,#19461,#19462),.UNSPECIFIED.,.F.,.F.,(4,1,1,
1,1,1,1,1,4),(91.106186954104,91.2525760793983,92.2449959196119,93.2374157598255,
94.2298356000392,95.2222554402528,96.2146752804664,97.2070951206801,97.3893722612836),
 .UNSPECIFIED.);
#2340=B_SPLINE_CURVE_WITH_KNOTS('',3,(#19463,#19464,#19465,#19466,#19467,
#19468,#19469,#19470,#19471,#19472),.UNSPECIFIED.,.F.,.F.,(4,1,1,1,1,1,
1,4),(91.106186954104,91.807147663635,92.7995675038486,93.7919873440623,
94.7844071842759,95.7768270244895,96.7692468647032,97.3893722612836),
 .UNSPECIFIED.);
#2341=B_SPLINE_CURVE_WITH_KNOTS('',3,(#19477,#19478,#19479,#19480,#19481,
#19482,#19483,#19484,#19485,#19486),.UNSPECIFIED.,.F.,.F.,(4,1,1,1,1,1,
1,4),(84.8230016469244,85.2980570381165,86.2904768783301,87.2828967185437,
88.2753165587574,89.267736398971,90.2601562391846,91.106186954104),
 .UNSPECIFIED.);
#2342=B_SPLINE_CURVE_WITH_KNOTS('',3,(#19487,#19488,#19489,#19490,#19491,
#19492,#19493,#19494,#19495,#19496,#19497),.UNSPECIFIED.,.F.,.F.,(4,1,1,
1,1,1,1,1,4),(84.8230016469244,84.8602087821396,85.8526286223532,86.8450484625669,
87.8374683027805,88.8298881429941,89.8223079832078,90.8147278234214,91.106186954104),
 .UNSPECIFIED.);
#2343=B_SPLINE_CURVE_WITH_KNOTS('',3,(#19502,#19503,#19504,#19505,#19506,
#19507,#19508,#19509,#19510,#19511),.UNSPECIFIED.,.F.,.F.,(4,1,1,1,1,1,
1,4),(78.5398163397448,79.3435379968347,80.3359578370483,81.328377677262,
82.3207975174756,83.3132173576892,84.3056371979029,84.8230016469244),
 .UNSPECIFIED.);
#2344=B_SPLINE_CURVE_WITH_KNOTS('',3,(#19512,#19513,#19514,#19515,#19516,
#19517,#19518,#19519,#19520,#19521),.UNSPECIFIED.,.F.,.F.,(4,1,1,1,1,1,
1,4),(78.5398163397448,78.9056897408578,79.8981095810714,80.8905294212851,
81.8829492614987,82.8753691017123,83.867788941926,84.8230016469244),
 .UNSPECIFIED.);
#2345=B_SPLINE_CURVE_WITH_KNOTS('',3,(#19526,#19527,#19528,#19529,#19530,
#19531,#19532,#19533,#19534,#19535,#19536),.UNSPECIFIED.,.F.,.F.,(4,1,1,
1,1,1,1,1,4),(72.2566310325652,72.3965991153393,73.3890189555529,74.3814387957665,
75.3738586359802,76.3662784761938,77.3586983164074,78.3511181566211,78.5398163397448),
 .UNSPECIFIED.);
#2346=B_SPLINE_CURVE_WITH_KNOTS('',3,(#19537,#19538,#19539,#19540,#19541,
#19542,#19543,#19544,#19545,#19546),.UNSPECIFIED.,.F.,.F.,(4,1,1,1,1,1,
1,4),(72.2566310325652,72.951170699576,73.9435905397896,74.9360103800033,
75.9284302202169,76.9208500604305,77.9132699006442,78.5398163397448),
 .UNSPECIFIED.);
#2347=B_SPLINE_CURVE_WITH_KNOTS('',3,(#19551,#19552,#19553,#19554,#19555,
#19556,#19557,#19558,#19559,#19560),.UNSPECIFIED.,.F.,.F.,(4,1,1,1,1,1,
1,4),(65.9734457253856,66.4420800740575,67.4344999142711,68.4269197544847,
69.4193395946984,70.411759434912,71.4041792751256,72.2566310325652),
 .UNSPECIFIED.);
#2348=B_SPLINE_CURVE_WITH_KNOTS('',3,(#19561,#19562,#19563,#19564,#19565,
#19566,#19567,#19568,#19569,#19570,#19571),.UNSPECIFIED.,.F.,.F.,(4,1,1,
1,1,1,1,1,4),(65.9734457253856,66.0042318180806,66.9966516582942,67.9890714985079,
68.9814913387215,69.9739111789351,70.9663310191488,71.9587508593624,72.2566310325652),
 .UNSPECIFIED.);
#2349=B_SPLINE_CURVE_WITH_KNOTS('',3,(#19576,#19577,#19578,#19579,#19580,
#19581,#19582,#19583,#19584,#19585),.UNSPECIFIED.,.F.,.F.,(4,1,1,1,1,1,
1,4),(59.690260418206,60.4875610327757,61.4799808729893,62.4724007132029,
63.4648205534166,64.4572403936302,65.4496602338438,65.9734457253856),
 .UNSPECIFIED.);
#2350=B_SPLINE_CURVE_WITH_KNOTS('',3,(#19586,#19587,#19588,#19589,#19590,
#19591,#19592,#19593,#19594,#19595),.UNSPECIFIED.,.F.,.F.,(4,1,1,1,1,1,
1,4),(59.690260418206,60.0497127767988,61.0421326170124,62.0345524572261,
63.0269722974397,64.0193921376533,65.011811977867,65.9734457253856),
 .UNSPECIFIED.);
#2351=B_SPLINE_CURVE_WITH_KNOTS('',3,(#19600,#19601,#19602,#19603,#19604,
#19605,#19606,#19607,#19608,#19609,#19610),.UNSPECIFIED.,.F.,.F.,(4,1,1,
1,1,1,1,1,4),(53.4070751110264,53.5406221512803,54.5330419914939,55.5254618317075,
56.5178816719212,57.5103015121348,58.5027213523484,59.4951411925621,59.690260418206),
 .UNSPECIFIED.);
#2352=B_SPLINE_CURVE_WITH_KNOTS('',3,(#19611,#19612,#19613,#19614,#19615,
#19616,#19617,#19618,#19619,#19620),.UNSPECIFIED.,.F.,.F.,(4,1,1,1,1,1,
1,4),(53.4070751110264,54.095193735517,55.0876135757306,56.0800334159443,
57.0724532561579,58.0648730963715,59.0572929365852,59.690260418206),
 .UNSPECIFIED.);
#2353=B_SPLINE_CURVE_WITH_KNOTS('',3,(#19625,#19626,#19627,#19628,#19629,
#19630,#19631,#19632,#19633,#19634),.UNSPECIFIED.,.F.,.F.,(4,1,1,1,1,1,
1,4),(47.1238898038468,47.5861031099985,48.5785229502121,49.5709427904257,
50.5633626306394,51.555782470853,52.5482023110666,53.4070751110264),
 .UNSPECIFIED.);
#2354=B_SPLINE_CURVE_WITH_KNOTS('',3,(#19635,#19636,#19637,#19638,#19639,
#19640,#19641,#19642,#19643,#19644,#19645),.UNSPECIFIED.,.F.,.F.,(4,1,1,
1,1,1,1,1,4),(47.1238898038468,47.1482548540216,48.1406746942352,49.1330945344489,
50.1255143746625,51.1179342148761,52.1103540550898,53.1027738953034,53.4070751110264),
 .UNSPECIFIED.);
#2355=B_SPLINE_CURVE_WITH_KNOTS('',3,(#19650,#19651,#19652,#19653,#19654,
#19655,#19656,#19657,#19658,#19659),.UNSPECIFIED.,.F.,.F.,(4,1,1,1,1,1,
1,4),(40.8407044966672,41.6315840687167,42.6240039089303,43.6164237491439,
44.6088435893576,45.6012634295712,46.5936832697848,47.1238898038468),
 .UNSPECIFIED.);
#2356=B_SPLINE_CURVE_WITH_KNOTS('',3,(#19660,#19661,#19662,#19663,#19664,
#19665,#19666,#19667,#19668,#19669),.UNSPECIFIED.,.F.,.F.,(4,1,1,1,1,1,
1,4),(40.8407044966672,41.1937358127398,42.1861556529534,43.1785754931671,
44.1709953333807,45.1634151735943,46.155835013808,47.1238898038468),
 .UNSPECIFIED.);
#2357=B_SPLINE_CURVE_WITH_KNOTS('',3,(#19674,#19675,#19676,#19677,#19678,
#19679,#19680,#19681,#19682,#19683,#19684),.UNSPECIFIED.,.F.,.F.,(4,1,1,
1,1,1,1,1,4),(34.5575191894876,34.6846451872213,35.6770650274349,36.6694848676485,
37.6619047078622,38.6543245480758,39.6467443882894,40.639164228503,40.8407044966672),
 .UNSPECIFIED.);
#2358=B_SPLINE_CURVE_WITH_KNOTS('',3,(#19685,#19686,#19687,#19688,#19689,
#19690,#19691,#19692,#19693,#19694),.UNSPECIFIED.,.F.,.F.,(4,1,1,1,1,1,
1,4),(34.5575191894876,35.239216771458,36.2316366116717,37.2240564518853,
38.2164762920989,39.2088961323126,40.2013159725262,40.8407044966672),
 .UNSPECIFIED.);
#2359=B_SPLINE_CURVE_WITH_KNOTS('',3,(#19699,#19700,#19701,#19702,#19703,
#19704,#19705,#19706,#19707,#19708),.UNSPECIFIED.,.F.,.F.,(4,1,1,1,1,1,
1,4),(28.274333882308,28.7301261459395,29.7225459861531,30.7149658263667,
31.7073856665804,32.699805506794,33.6922253470076,34.5575191894876),
 .UNSPECIFIED.);
#2360=B_SPLINE_CURVE_WITH_KNOTS('',3,(#19709,#19710,#19711,#19712,#19713,
#19714,#19715,#19716,#19717,#19718,#19719),.UNSPECIFIED.,.F.,.F.,(4,1,1,
1,1,1,1,1,4),(28.274333882308,28.2922778899626,29.2846977301762,30.2771175703899,
31.2695374106035,32.2619572508171,33.2543770910308,34.2467969312444,34.5575191894876),
 .UNSPECIFIED.);
#2361=B_SPLINE_CURVE_WITH_KNOTS('',3,(#19724,#19725,#19726,#19727,#19728,
#19729,#19730,#19731,#19732,#19733),.UNSPECIFIED.,.F.,.F.,(4,1,1,1,1,1,
1,4),(21.9911485751285,22.7756071046577,23.7680269448713,24.7604467850849,
25.7528666252986,26.7452864655122,27.7377063057258,28.274333882308),
 .UNSPECIFIED.);
#2362=B_SPLINE_CURVE_WITH_KNOTS('',3,(#19734,#19735,#19736,#19737,#19738,
#19739,#19740,#19741,#19742,#19743),.UNSPECIFIED.,.F.,.F.,(4,1,1,1,1,1,
1,4),(21.9911485751285,22.3377588486808,23.3301786888945,24.3225985291081,
25.3150183693217,26.3074382095353,27.299858049749,28.274333882308),
 .UNSPECIFIED.);
#2363=B_SPLINE_CURVE_WITH_KNOTS('',3,(#19749,#19750,#19751,#19752,#19753),
 .UNSPECIFIED.,.F.,.F.,(4,1,4),(14.3984001269718,15.3908199671854,15.7079632679489),
 .UNSPECIFIED.);
#2364=B_SPLINE_CURVE_WITH_KNOTS('',3,(#19756,#19757,#19758,#19759,#19760),
 .UNSPECIFIED.,.F.,.F.,(4,1,4),(13.8759337553362,14.8362483829486,15.7079632679489),
 .UNSPECIFIED.);
#2365=B_SPLINE_CURVE_WITH_KNOTS('',3,(#19766,#19767,#19768,#19769,#19770,
#19771,#19772,#19773),.UNSPECIFIED.,.F.,.F.,(4,1,1,1,1,4),(103.672557568463,
104.154034002175,105.146453842389,106.138873682603,107.131293522816,108.12371336303),
 .UNSPECIFIED.);
#2366=B_SPLINE_CURVE_WITH_KNOTS('',3,(#19776,#19777,#19778,#19779,#19780,
#19781,#19782,#19783,#19784),.UNSPECIFIED.,.F.,.F.,(4,1,1,1,1,1,4),(103.672557568463,
103.716185746199,104.708605586412,105.701025426626,106.693445266839,107.685865107053,
108.646179734666),.UNSPECIFIED.);
#2367=B_SPLINE_CURVE_WITH_KNOTS('',3,(#19789,#19790,#19791,#19792,#19793,
#19794,#19795,#19796,#19797,#19798),.UNSPECIFIED.,.F.,.F.,(4,1,1,1,1,1,
1,4),(97.3893722612836,98.1995149608937,99.1919348011073,100.184354641321,
101.176774481535,102.169194321748,103.161614161962,103.672557568463),
 .UNSPECIFIED.);
#2368=B_SPLINE_CURVE_WITH_KNOTS('',3,(#19799,#19800,#19801,#19802,#19803,
#19804,#19805,#19806,#19807,#19808),.UNSPECIFIED.,.F.,.F.,(4,1,1,1,1,1,
1,4),(97.3893722612836,97.7616667049168,98.7540865451304,99.7465063853441,
100.738926225558,101.731346065771,102.723765905985,103.672557568463),
 .UNSPECIFIED.);
#2369=B_SPLINE_CURVE_WITH_KNOTS('',3,(#19813,#19814,#19815,#19816,#19817,
#19818,#19819,#19820,#19821,#19822,#19823),.UNSPECIFIED.,.F.,.F.,(4,1,1,
1,1,1,1,1,4),(91.106186954104,91.2525760793983,92.2449959196119,93.2374157598255,
94.2298356000392,95.2222554402528,96.2146752804664,97.2070951206801,97.3893722612836),
 .UNSPECIFIED.);
#2370=B_SPLINE_CURVE_WITH_KNOTS('',3,(#19824,#19825,#19826,#19827,#19828,
#19829,#19830,#19831,#19832,#19833),.UNSPECIFIED.,.F.,.F.,(4,1,1,1,1,1,
1,4),(91.106186954104,91.807147663635,92.7995675038486,93.7919873440623,
94.7844071842759,95.7768270244895,96.7692468647032,97.3893722612836),
 .UNSPECIFIED.);
#2371=B_SPLINE_CURVE_WITH_KNOTS('',3,(#19838,#19839,#19840,#19841,#19842,
#19843,#19844,#19845,#19846,#19847),.UNSPECIFIED.,.F.,.F.,(4,1,1,1,1,1,
1,4),(84.8230016469244,85.2980570381165,86.2904768783301,87.2828967185437,
88.2753165587574,89.267736398971,90.2601562391846,91.106186954104),
 .UNSPECIFIED.);
#2372=B_SPLINE_CURVE_WITH_KNOTS('',3,(#19848,#19849,#19850,#19851,#19852,
#19853,#19854,#19855,#19856,#19857,#19858),.UNSPECIFIED.,.F.,.F.,(4,1,1,
1,1,1,1,1,4),(84.8230016469244,84.8602087821396,85.8526286223532,86.8450484625669,
87.8374683027805,88.8298881429941,89.8223079832078,90.8147278234214,91.106186954104),
 .UNSPECIFIED.);
#2373=B_SPLINE_CURVE_WITH_KNOTS('',3,(#19863,#19864,#19865,#19866,#19867,
#19868,#19869,#19870,#19871,#19872),.UNSPECIFIED.,.F.,.F.,(4,1,1,1,1,1,
1,4),(78.5398163397448,79.3435379968347,80.3359578370483,81.328377677262,
82.3207975174756,83.3132173576892,84.3056371979029,84.8230016469244),
 .UNSPECIFIED.);
#2374=B_SPLINE_CURVE_WITH_KNOTS('',3,(#19873,#19874,#19875,#19876,#19877,
#19878,#19879,#19880,#19881,#19882),.UNSPECIFIED.,.F.,.F.,(4,1,1,1,1,1,
1,4),(78.5398163397448,78.9056897408578,79.8981095810714,80.8905294212851,
81.8829492614987,82.8753691017123,83.867788941926,84.8230016469244),
 .UNSPECIFIED.);
#2375=B_SPLINE_CURVE_WITH_KNOTS('',3,(#19887,#19888,#19889,#19890,#19891,
#19892,#19893,#19894,#19895,#19896,#19897),.UNSPECIFIED.,.F.,.F.,(4,1,1,
1,1,1,1,1,4),(72.2566310325652,72.3965991153393,73.3890189555529,74.3814387957665,
75.3738586359802,76.3662784761938,77.3586983164074,78.3511181566211,78.5398163397448),
 .UNSPECIFIED.);
#2376=B_SPLINE_CURVE_WITH_KNOTS('',3,(#19898,#19899,#19900,#19901,#19902,
#19903,#19904,#19905,#19906,#19907),.UNSPECIFIED.,.F.,.F.,(4,1,1,1,1,1,
1,4),(72.2566310325652,72.951170699576,73.9435905397896,74.9360103800033,
75.9284302202169,76.9208500604305,77.9132699006442,78.5398163397448),
 .UNSPECIFIED.);
#2377=B_SPLINE_CURVE_WITH_KNOTS('',3,(#19912,#19913,#19914,#19915,#19916,
#19917,#19918,#19919,#19920,#19921),.UNSPECIFIED.,.F.,.F.,(4,1,1,1,1,1,
1,4),(65.9734457253856,66.4420800740575,67.4344999142711,68.4269197544847,
69.4193395946984,70.411759434912,71.4041792751256,72.2566310325652),
 .UNSPECIFIED.);
#2378=B_SPLINE_CURVE_WITH_KNOTS('',3,(#19922,#19923,#19924,#19925,#19926,
#19927,#19928,#19929,#19930,#19931,#19932),.UNSPECIFIED.,.F.,.F.,(4,1,1,
1,1,1,1,1,4),(65.9734457253856,66.0042318180806,66.9966516582942,67.9890714985079,
68.9814913387215,69.9739111789351,70.9663310191488,71.9587508593624,72.2566310325652),
 .UNSPECIFIED.);
#2379=B_SPLINE_CURVE_WITH_KNOTS('',3,(#19937,#19938,#19939,#19940,#19941,
#19942,#19943,#19944,#19945,#19946),.UNSPECIFIED.,.F.,.F.,(4,1,1,1,1,1,
1,4),(59.690260418206,60.4875610327757,61.4799808729893,62.4724007132029,
63.4648205534166,64.4572403936302,65.4496602338438,65.9734457253856),
 .UNSPECIFIED.);
#2380=B_SPLINE_CURVE_WITH_KNOTS('',3,(#19947,#19948,#19949,#19950,#19951,
#19952,#19953,#19954,#19955,#19956),.UNSPECIFIED.,.F.,.F.,(4,1,1,1,1,1,
1,4),(59.690260418206,60.0497127767988,61.0421326170124,62.0345524572261,
63.0269722974397,64.0193921376533,65.011811977867,65.9734457253856),
 .UNSPECIFIED.);
#2381=B_SPLINE_CURVE_WITH_KNOTS('',3,(#19961,#19962,#19963,#19964,#19965,
#19966,#19967,#19968,#19969,#19970,#19971),.UNSPECIFIED.,.F.,.F.,(4,1,1,
1,1,1,1,1,4),(53.4070751110264,53.5406221512803,54.5330419914939,55.5254618317075,
56.5178816719212,57.5103015121348,58.5027213523484,59.4951411925621,59.690260418206),
 .UNSPECIFIED.);
#2382=B_SPLINE_CURVE_WITH_KNOTS('',3,(#19972,#19973,#19974,#19975,#19976,
#19977,#19978,#19979,#19980,#19981),.UNSPECIFIED.,.F.,.F.,(4,1,1,1,1,1,
1,4),(53.4070751110264,54.095193735517,55.0876135757306,56.0800334159443,
57.0724532561579,58.0648730963715,59.0572929365852,59.690260418206),
 .UNSPECIFIED.);
#2383=B_SPLINE_CURVE_WITH_KNOTS('',3,(#19986,#19987,#19988,#19989,#19990,
#19991,#19992,#19993,#19994,#19995),.UNSPECIFIED.,.F.,.F.,(4,1,1,1,1,1,
1,4),(47.1238898038468,47.5861031099985,48.5785229502121,49.5709427904257,
50.5633626306394,51.555782470853,52.5482023110666,53.4070751110264),
 .UNSPECIFIED.);
#2384=B_SPLINE_CURVE_WITH_KNOTS('',3,(#19996,#19997,#19998,#19999,#20000,
#20001,#20002,#20003,#20004,#20005,#20006),.UNSPECIFIED.,.F.,.F.,(4,1,1,
1,1,1,1,1,4),(47.1238898038468,47.1482548540216,48.1406746942352,49.1330945344489,
50.1255143746625,51.1179342148761,52.1103540550898,53.1027738953034,53.4070751110264),
 .UNSPECIFIED.);
#2385=B_SPLINE_CURVE_WITH_KNOTS('',3,(#20011,#20012,#20013,#20014,#20015,
#20016,#20017,#20018,#20019,#20020),.UNSPECIFIED.,.F.,.F.,(4,1,1,1,1,1,
1,4),(40.8407044966672,41.6315840687167,42.6240039089303,43.6164237491439,
44.6088435893576,45.6012634295712,46.5936832697848,47.1238898038468),
 .UNSPECIFIED.);
#2386=B_SPLINE_CURVE_WITH_KNOTS('',3,(#20021,#20022,#20023,#20024,#20025,
#20026,#20027,#20028,#20029,#20030),.UNSPECIFIED.,.F.,.F.,(4,1,1,1,1,1,
1,4),(40.8407044966672,41.1937358127398,42.1861556529534,43.1785754931671,
44.1709953333807,45.1634151735943,46.155835013808,47.1238898038468),
 .UNSPECIFIED.);
#2387=B_SPLINE_CURVE_WITH_KNOTS('',3,(#20035,#20036,#20037,#20038,#20039,
#20040,#20041,#20042,#20043,#20044,#20045),.UNSPECIFIED.,.F.,.F.,(4,1,1,
1,1,1,1,1,4),(34.5575191894876,34.6846451872213,35.6770650274349,36.6694848676485,
37.6619047078622,38.6543245480758,39.6467443882894,40.639164228503,40.8407044966672),
 .UNSPECIFIED.);
#2388=B_SPLINE_CURVE_WITH_KNOTS('',3,(#20046,#20047,#20048,#20049,#20050,
#20051,#20052,#20053,#20054,#20055),.UNSPECIFIED.,.F.,.F.,(4,1,1,1,1,1,
1,4),(34.5575191894876,35.239216771458,36.2316366116717,37.2240564518853,
38.2164762920989,39.2088961323126,40.2013159725262,40.8407044966672),
 .UNSPECIFIED.);
#2389=B_SPLINE_CURVE_WITH_KNOTS('',3,(#20060,#20061,#20062,#20063,#20064,
#20065,#20066,#20067,#20068,#20069),.UNSPECIFIED.,.F.,.F.,(4,1,1,1,1,1,
1,4),(28.274333882308,28.7301261459395,29.7225459861531,30.7149658263667,
31.7073856665804,32.699805506794,33.6922253470076,34.5575191894876),
 .UNSPECIFIED.);
#2390=B_SPLINE_CURVE_WITH_KNOTS('',3,(#20070,#20071,#20072,#20073,#20074,
#20075,#20076,#20077,#20078,#20079,#20080),.UNSPECIFIED.,.F.,.F.,(4,1,1,
1,1,1,1,1,4),(28.274333882308,28.2922778899626,29.2846977301762,30.2771175703899,
31.2695374106035,32.2619572508171,33.2543770910308,34.2467969312444,34.5575191894876),
 .UNSPECIFIED.);
#2391=B_SPLINE_CURVE_WITH_KNOTS('',3,(#20085,#20086,#20087,#20088,#20089,
#20090,#20091,#20092,#20093,#20094),.UNSPECIFIED.,.F.,.F.,(4,1,1,1,1,1,
1,4),(21.9911485751285,22.7756071046577,23.7680269448713,24.7604467850849,
25.7528666252986,26.7452864655122,27.7377063057258,28.274333882308),
 .UNSPECIFIED.);
#2392=B_SPLINE_CURVE_WITH_KNOTS('',3,(#20095,#20096,#20097,#20098,#20099,
#20100,#20101,#20102,#20103,#20104),.UNSPECIFIED.,.F.,.F.,(4,1,1,1,1,1,
1,4),(21.9911485751285,22.3377588486808,23.3301786888945,24.3225985291081,
25.3150183693217,26.3074382095353,27.299858049749,28.274333882308),
 .UNSPECIFIED.);
#2393=B_SPLINE_CURVE_WITH_KNOTS('',3,(#20110,#20111,#20112,#20113,#20114),
 .UNSPECIFIED.,.F.,.F.,(4,1,4),(14.3984001269718,15.3908199671854,15.7079632679489),
 .UNSPECIFIED.);
#2394=B_SPLINE_CURVE_WITH_KNOTS('',3,(#20117,#20118,#20119,#20120,#20121),
 .UNSPECIFIED.,.F.,.F.,(4,1,4),(13.8759337553362,14.8362483829486,15.7079632679489),
 .UNSPECIFIED.);
#2395=B_SPLINE_CURVE_WITH_KNOTS('',3,(#20127,#20128,#20129,#20130),
 .UNSPECIFIED.,.F.,.F.,(4,4),(95.5573427486709,96.2647245007222),
 .UNSPECIFIED.);
#2396=B_SPLINE_CURVE_WITH_KNOTS('',3,(#20138,#20139,#20140,#20141,#20142,
#20143,#20144,#20145,#20146,#20147),.UNSPECIFIED.,.F.,.F.,(4,3,3,4),(-94.2477796076938,
-93.2874649800814,-92.2950451398677,-91.8135687061554),.UNSPECIFIED.);
#2397=B_SPLINE_CURVE_WITH_KNOTS('',3,(#20152,#20153,#20154,#20155,#20156,
#20157,#20158,#20159,#20160,#20161,#20162,#20163,#20164,#20165,#20166,#20167,
#20168,#20169,#20170,#20171,#20172,#20173,#20174,#20175,#20176),
 .UNSPECIFIED.,.F.,.F.,(4,3,3,3,3,3,3,3,4),(89.2741574414913,89.3177856192268,
90.3102054594404,91.3026252996541,92.2950451398677,93.2874649800813,94.279884820295,
95.2723046605086,95.5573427486709),.UNSPECIFIED.);
#2398=B_SPLINE_CURVE_WITH_KNOTS('',3,(#20177,#20178,#20179,#20180,#20181,
#20182,#20183,#20184,#20185,#20186,#20187,#20188,#20189,#20190,#20191,#20192,
#20193,#20194,#20195,#20196,#20197,#20198),.UNSPECIFIED.,.F.,.F.,(4,3,3,
3,3,3,3,4),(-91.8135687061554,-91.3026252996541,-90.3102054594405,-89.3177856192269,
-88.3253657790132,-87.3329459387996,-86.340526098586,-85.5303833989758),
 .UNSPECIFIED.);
#2399=B_SPLINE_CURVE_WITH_KNOTS('',3,(#20203,#20204,#20205,#20206,#20207,
#20208,#20209,#20210,#20211,#20212,#20213,#20214,#20215,#20216,#20217,#20218,
#20219,#20220,#20221,#20222,#20223,#20224),.UNSPECIFIED.,.F.,.F.,(4,3,3,
3,3,3,3,4),(82.9909721343117,83.363266577945,84.3556864181587,85.3481062583723,
86.3405260985859,87.3329459387996,88.3253657790132,89.2741574414913),
 .UNSPECIFIED.);
#2400=B_SPLINE_CURVE_WITH_KNOTS('',3,(#20225,#20226,#20227,#20228,#20229,
#20230,#20231,#20232,#20233,#20234,#20235,#20236,#20237,#20238,#20239,#20240,
#20241,#20242,#20243,#20244,#20245,#20246,#20247,#20248,#20249),
 .UNSPECIFIED.,.F.,.F.,(4,3,3,3,3,3,3,3,4),(-85.5303833989758,-85.3481062583723,
-84.3556864181587,-83.3632665779451,-82.3708467377314,-81.3784268975178,
-80.3860070573042,-79.3935872170905,-79.2471980917962),.UNSPECIFIED.);
#2401=B_SPLINE_CURVE_WITH_KNOTS('',3,(#20254,#20255,#20256,#20257,#20258,
#20259,#20260,#20261,#20262,#20263,#20264,#20265,#20266,#20267,#20268,#20269,
#20270,#20271,#20272,#20273,#20274,#20275),.UNSPECIFIED.,.F.,.F.,(4,3,3,
3,3,3,3,4),(76.7077868271321,77.4087475366632,78.4011673768769,79.3935872170905,
80.3860070573041,81.3784268975178,82.3708467377314,82.9909721343117),
 .UNSPECIFIED.);
#2402=B_SPLINE_CURVE_WITH_KNOTS('',3,(#20276,#20277,#20278,#20279,#20280,
#20281,#20282,#20283,#20284,#20285,#20286,#20287,#20288,#20289,#20290,#20291,
#20292,#20293,#20294,#20295,#20296,#20297),.UNSPECIFIED.,.F.,.F.,(4,3,3,
3,3,3,3,4),(-79.2471980917962,-78.4011673768769,-77.4087475366633,-76.4163276964496,
-75.423907856236,-74.4314880160224,-73.4390681758088,-72.9640127846167),
 .UNSPECIFIED.);
#2403=B_SPLINE_CURVE_WITH_KNOTS('',3,(#20302,#20303,#20304,#20305,#20306,
#20307,#20308,#20309,#20310,#20311,#20312,#20313,#20314,#20315,#20316,#20317,
#20318,#20319,#20320,#20321,#20322,#20323,#20324,#20325,#20326),
 .UNSPECIFIED.,.F.,.F.,(4,3,3,3,3,3,3,3,4),(70.4246015199525,70.4618086551678,
71.4542284953814,72.4466483355951,73.4390681758087,74.4314880160223,75.423907856236,
76.4163276964496,76.7077868271321),.UNSPECIFIED.);
#2404=B_SPLINE_CURVE_WITH_KNOTS('',3,(#20327,#20328,#20329,#20330,#20331,
#20332,#20333,#20334,#20335,#20336,#20337,#20338,#20339,#20340,#20341,#20342,
#20343,#20344,#20345,#20346,#20347,#20348),.UNSPECIFIED.,.F.,.F.,(4,3,3,
3,3,3,3,4),(-72.9640127846167,-72.4466483355951,-71.4542284953815,-70.4618086551678,
-69.4693888149542,-68.4769689747406,-67.4845491345269,-66.680827477437),
 .UNSPECIFIED.);
#2405=B_SPLINE_CURVE_WITH_KNOTS('',3,(#20353,#20354,#20355,#20356,#20357,
#20358,#20359,#20360,#20361,#20362,#20363,#20364,#20365,#20366,#20367,#20368,
#20369,#20370,#20371,#20372,#20373,#20374),.UNSPECIFIED.,.F.,.F.,(4,3,3,
3,3,3,3,4),(64.1414162127729,64.507289613886,65.4997094540997,66.4921292943133,
67.4845491345269,68.4769689747405,69.4693888149542,70.4246015199525),
 .UNSPECIFIED.);
#2406=B_SPLINE_CURVE_WITH_KNOTS('',3,(#20375,#20376,#20377,#20378,#20379,
#20380,#20381,#20382,#20383,#20384,#20385,#20386,#20387,#20388,#20389,#20390,
#20391,#20392,#20393,#20394,#20395,#20396,#20397,#20398,#20399),
 .UNSPECIFIED.,.F.,.F.,(4,3,3,3,3,3,3,3,4),(-66.680827477437,-66.4921292943133,
-65.4997094540997,-64.5072896138861,-63.5148697736724,-62.5224499334588,
-61.5300300932452,-60.5376102530315,-60.3976421702575),.UNSPECIFIED.);
#2407=B_SPLINE_CURVE_WITH_KNOTS('',3,(#20404,#20405,#20406,#20407,#20408,
#20409,#20410,#20411,#20412,#20413,#20414,#20415,#20416,#20417,#20418,#20419,
#20420,#20421,#20422,#20423,#20424,#20425),.UNSPECIFIED.,.F.,.F.,(4,3,3,
3,3,3,3,4),(57.8582309055933,58.5527705726042,59.5451904128179,60.5376102530315,
61.5300300932451,62.5224499334588,63.5148697736724,64.1414162127729),
 .UNSPECIFIED.);
#2408=B_SPLINE_CURVE_WITH_KNOTS('',3,(#20426,#20427,#20428,#20429,#20430,
#20431,#20432,#20433,#20434,#20435,#20436,#20437,#20438,#20439,#20440,#20441,
#20442,#20443,#20444,#20445,#20446,#20447),.UNSPECIFIED.,.F.,.F.,(4,3,3,
3,3,3,3,4),(-60.3976421702575,-59.5451904128179,-58.5527705726043,-57.5603507323906,
-56.567930892177,-55.5755110519634,-54.5830912117497,-54.1144568630778),
 .UNSPECIFIED.);
#2409=B_SPLINE_CURVE_WITH_KNOTS('',3,(#20452,#20453,#20454,#20455,#20456,
#20457,#20458,#20459,#20460,#20461,#20462,#20463,#20464,#20465,#20466,#20467,
#20468,#20469,#20470,#20471,#20472,#20473,#20474,#20475,#20476),
 .UNSPECIFIED.,.F.,.F.,(4,3,3,3,3,3,3,3,4),(51.5750455984138,51.6058316911088,
52.5982515313225,53.5906713715361,54.5830912117497,55.5755110519634,56.567930892177,
57.5603507323906,57.8582309055933),.UNSPECIFIED.);
#2410=B_SPLINE_CURVE_WITH_KNOTS('',3,(#20477,#20478,#20479,#20480,#20481,
#20482,#20483,#20484,#20485,#20486,#20487,#20488,#20489,#20490,#20491,#20492,
#20493,#20494,#20495,#20496,#20497,#20498),.UNSPECIFIED.,.F.,.F.,(4,3,3,
3,3,3,3,4),(-54.1144568630778,-53.5906713715361,-52.5982515313225,-51.6058316911089,
-50.6134118508952,-49.6209920106816,-48.628572170468,-47.8312715558983),
 .UNSPECIFIED.);
#2411=B_SPLINE_CURVE_WITH_KNOTS('',3,(#20503,#20504,#20505,#20506,#20507,
#20508,#20509,#20510,#20511,#20512,#20513,#20514,#20515,#20516,#20517,#20518,
#20519,#20520,#20521,#20522,#20523,#20524),.UNSPECIFIED.,.F.,.F.,(4,3,3,
3,3,3,3,4),(45.2918602912342,45.651312649827,46.6437324900407,47.6361523302543,
48.6285721704679,49.6209920106816,50.6134118508952,51.5750455984138),
 .UNSPECIFIED.);
#2412=B_SPLINE_CURVE_WITH_KNOTS('',3,(#20525,#20526,#20527,#20528,#20529,
#20530,#20531,#20532,#20533,#20534,#20535,#20536,#20537,#20538,#20539,#20540,
#20541,#20542,#20543,#20544,#20545,#20546,#20547,#20548,#20549),
 .UNSPECIFIED.,.F.,.F.,(4,3,3,3,3,3,3,3,4),(-47.8312715558983,-47.6361523302543,
-46.6437324900407,-45.6513126498271,-44.6588928096134,-43.6664729693998,
-42.6740531291862,-41.6816332889725,-41.5480862487187),.UNSPECIFIED.);
#2413=B_SPLINE_CURVE_WITH_KNOTS('',3,(#20554,#20555,#20556,#20557,#20558,
#20559,#20560,#20561,#20562,#20563,#20564,#20565,#20566,#20567,#20568,#20569,
#20570,#20571,#20572,#20573,#20574,#20575),.UNSPECIFIED.,.F.,.F.,(4,3,3,
3,3,3,3,4),(39.0086749840546,39.6967936085453,40.6892134487589,41.6816332889725,
42.6740531291861,43.6664729693998,44.6588928096134,45.2918602912342),
 .UNSPECIFIED.);
#2414=B_SPLINE_CURVE_WITH_KNOTS('',3,(#20576,#20577,#20578,#20579,#20580,
#20581,#20582,#20583,#20584,#20585,#20586,#20587,#20588,#20589,#20590,#20591,
#20592,#20593,#20594,#20595,#20596,#20597),.UNSPECIFIED.,.F.,.F.,(4,3,3,
3,3,3,3,4),(-41.5480862487187,-40.6892134487589,-39.6967936085453,-38.7043737683316,
-37.711953928118,-36.7195340879044,-35.7271142476907,-35.2649009415391),
 .UNSPECIFIED.);
#2415=B_SPLINE_CURVE_WITH_KNOTS('',3,(#20602,#20603,#20604,#20605,#20606,
#20607,#20608,#20609,#20610,#20611,#20612,#20613,#20614,#20615,#20616,#20617,
#20618,#20619,#20620,#20621,#20622,#20623,#20624,#20625,#20626),
 .UNSPECIFIED.,.F.,.F.,(4,3,3,3,3,3,3,3,4),(32.725489676875,32.7498547270498,
33.7422745672635,34.7346944074771,35.7271142476907,36.7195340879043,37.711953928118,
38.7043737683316,39.0086749840546),.UNSPECIFIED.);
#2416=B_SPLINE_CURVE_WITH_KNOTS('',3,(#20627,#20628,#20629,#20630,#20631,
#20632,#20633,#20634,#20635,#20636,#20637,#20638,#20639,#20640,#20641,#20642,
#20643,#20644,#20645,#20646,#20647,#20648),.UNSPECIFIED.,.F.,.F.,(4,3,3,
3,3,3,3,4),(-35.2649009415391,-34.7346944074771,-33.7422745672635,-32.7498547270498,
-31.7574348868362,-30.7650150466226,-29.772595206409,-28.9817156343595),
 .UNSPECIFIED.);
#2417=B_SPLINE_CURVE_WITH_KNOTS('',3,(#20653,#20654,#20655,#20656,#20657,
#20658,#20659,#20660,#20661,#20662,#20663,#20664,#20665,#20666,#20667,#20668,
#20669,#20670,#20671,#20672,#20673,#20674),.UNSPECIFIED.,.F.,.F.,(4,3,3,
3,3,3,3,4),(26.4423043696954,26.795335685768,27.7877555259817,28.7801753661953,
29.7725952064089,30.7650150466226,31.7574348868362,32.725489676875),
 .UNSPECIFIED.);
#2418=B_SPLINE_CURVE_WITH_KNOTS('',3,(#20675,#20676,#20677,#20678,#20679,
#20680,#20681,#20682,#20683,#20684,#20685,#20686,#20687,#20688,#20689,#20690,
#20691,#20692,#20693,#20694,#20695,#20696,#20697,#20698,#20699),
 .UNSPECIFIED.,.F.,.F.,(4,3,3,3,3,3,3,3,4),(-28.9817156343595,-28.7801753661953,
-27.7877555259817,-26.7953356857681,-25.8029158455544,-24.8104960053408,
-23.8180761651272,-22.8256563249135,-22.6985303271799),.UNSPECIFIED.);
#2419=B_SPLINE_CURVE_WITH_KNOTS('',3,(#20704,#20705,#20706,#20707,#20708,
#20709,#20710,#20711,#20712,#20713,#20714,#20715,#20716,#20717,#20718,#20719,
#20720,#20721,#20722,#20723,#20724,#20725),.UNSPECIFIED.,.F.,.F.,(4,3,3,
3,3,3,3,4),(20.1591190625158,20.8408166444862,21.8332364846999,22.8256563249135,
23.8180761651271,24.8104960053408,25.8029158455544,26.4423043696954),
 .UNSPECIFIED.);
#2420=B_SPLINE_CURVE_WITH_KNOTS('',3,(#20726,#20727,#20728,#20729,#20730,
#20731,#20732,#20733,#20734,#20735,#20736,#20737,#20738,#20739,#20740,#20741,
#20742,#20743,#20744,#20745,#20746,#20747),.UNSPECIFIED.,.F.,.F.,(4,3,3,
3,3,3,3,4),(-22.6985303271799,-21.8332364846999,-20.8408166444863,-19.8483968042726,
-18.855976964059,-17.8635571238454,-16.8711372836317,-16.4153450200003),
 .UNSPECIFIED.);
#2421=B_SPLINE_CURVE_WITH_KNOTS('',3,(#20752,#20753,#20754,#20755,#20756,
#20757,#20758,#20759,#20760,#20761,#20762,#20763,#20764,#20765,#20766,#20767,
#20768,#20769,#20770,#20771,#20772,#20773,#20774,#20775,#20776),
 .UNSPECIFIED.,.F.,.F.,(4,3,3,3,3,3,3,3,4),(13.8759337553362,13.8938777629908,
14.8862976032045,15.8787174434181,16.8711372836317,17.8635571238454,18.855976964059,
19.8483968042726,20.1591190625158),.UNSPECIFIED.);
#2422=B_SPLINE_CURVE_WITH_KNOTS('',3,(#20777,#20778,#20779,#20780,#20781,
#20782,#20783,#20784,#20785,#20786,#20787,#20788,#20789,#20790,#20791,#20792,
#20793,#20794,#20795,#20796,#20797,#20798),.UNSPECIFIED.,.F.,.F.,(4,3,3,
3,3,3,3,4),(-16.4153450200003,-15.8787174434181,-14.8862976032045,-13.8938777629908,
-12.9014579227772,-11.9090380825636,-10.9166182423499,-10.1321597128207),
 .UNSPECIFIED.);
#2423=B_SPLINE_CURVE_WITH_KNOTS('',3,(#20804,#20805,#20806,#20807,#20808,
#20809,#20810,#20811,#20812,#20813,#20814,#20815,#20816),.UNSPECIFIED.,
 .F.,.F.,(4,3,3,3,4),(-3.84897440564114,-2.9772595206409,-1.98483968042726,
-0.992419840213632,0.),.UNSPECIFIED.);
#2424=B_SPLINE_CURVE_WITH_KNOTS('',3,(#20819,#20820,#20821,#20822,#20823,
#20824,#20825,#20826,#20827,#20828,#20829,#20830,#20831,#20832,#20833,#20834,
#20835,#20836,#20837),.UNSPECIFIED.,.F.,.F.,(4,3,3,3,3,3,4),(2.01694489302841,
2.97725952064089,3.96967936085453,4.96209920106816,5.95451904128179,6.94693888149542,
7.59274844815661),.UNSPECIFIED.);
#2425=B_SPLINE_CURVE_WITH_KNOTS('',3,(#20843,#20844,#20845,#20846,#20847,
#20848,#20849,#20850),.UNSPECIFIED.,.F.,.F.,(4,1,1,1,1,4),(103.672557568463,
104.154034002175,105.146453842389,106.138873682603,107.131293522816,108.12371336303),
 .UNSPECIFIED.);
#2426=B_SPLINE_CURVE_WITH_KNOTS('',3,(#20853,#20854,#20855,#20856,#20857,
#20858,#20859,#20860,#20861),.UNSPECIFIED.,.F.,.F.,(4,1,1,1,1,1,4),(103.672557568463,
103.716185746199,104.708605586412,105.701025426626,106.693445266839,107.685865107053,
108.646179734666),.UNSPECIFIED.);
#2427=B_SPLINE_CURVE_WITH_KNOTS('',3,(#20866,#20867,#20868,#20869,#20870,
#20871,#20872,#20873,#20874,#20875),.UNSPECIFIED.,.F.,.F.,(4,1,1,1,1,1,
1,4),(97.3893722612836,98.1995149608937,99.1919348011073,100.184354641321,
101.176774481535,102.169194321748,103.161614161962,103.672557568463),
 .UNSPECIFIED.);
#2428=B_SPLINE_CURVE_WITH_KNOTS('',3,(#20876,#20877,#20878,#20879,#20880,
#20881,#20882,#20883,#20884,#20885),.UNSPECIFIED.,.F.,.F.,(4,1,1,1,1,1,
1,4),(97.3893722612836,97.7616667049168,98.7540865451304,99.7465063853441,
100.738926225558,101.731346065771,102.723765905985,103.672557568463),
 .UNSPECIFIED.);
#2429=B_SPLINE_CURVE_WITH_KNOTS('',3,(#20890,#20891,#20892,#20893,#20894,
#20895,#20896,#20897,#20898,#20899,#20900),.UNSPECIFIED.,.F.,.F.,(4,1,1,
1,1,1,1,1,4),(91.106186954104,91.2525760793983,92.2449959196119,93.2374157598255,
94.2298356000392,95.2222554402528,96.2146752804664,97.2070951206801,97.3893722612836),
 .UNSPECIFIED.);
#2430=B_SPLINE_CURVE_WITH_KNOTS('',3,(#20901,#20902,#20903,#20904,#20905,
#20906,#20907,#20908,#20909,#20910),.UNSPECIFIED.,.F.,.F.,(4,1,1,1,1,1,
1,4),(91.106186954104,91.807147663635,92.7995675038486,93.7919873440623,
94.7844071842759,95.7768270244895,96.7692468647032,97.3893722612836),
 .UNSPECIFIED.);
#2431=B_SPLINE_CURVE_WITH_KNOTS('',3,(#20915,#20916,#20917,#20918,#20919,
#20920,#20921,#20922,#20923,#20924),.UNSPECIFIED.,.F.,.F.,(4,1,1,1,1,1,
1,4),(84.8230016469244,85.2980570381165,86.2904768783301,87.2828967185437,
88.2753165587574,89.267736398971,90.2601562391846,91.106186954104),
 .UNSPECIFIED.);
#2432=B_SPLINE_CURVE_WITH_KNOTS('',3,(#20925,#20926,#20927,#20928,#20929,
#20930,#20931,#20932,#20933,#20934,#20935),.UNSPECIFIED.,.F.,.F.,(4,1,1,
1,1,1,1,1,4),(84.8230016469244,84.8602087821396,85.8526286223532,86.8450484625669,
87.8374683027805,88.8298881429941,89.8223079832078,90.8147278234214,91.106186954104),
 .UNSPECIFIED.);
#2433=B_SPLINE_CURVE_WITH_KNOTS('',3,(#20940,#20941,#20942,#20943,#20944,
#20945,#20946,#20947,#20948,#20949),.UNSPECIFIED.,.F.,.F.,(4,1,1,1,1,1,
1,4),(78.5398163397448,79.3435379968347,80.3359578370483,81.328377677262,
82.3207975174756,83.3132173576892,84.3056371979029,84.8230016469244),
 .UNSPECIFIED.);
#2434=B_SPLINE_CURVE_WITH_KNOTS('',3,(#20950,#20951,#20952,#20953,#20954,
#20955,#20956,#20957,#20958,#20959),.UNSPECIFIED.,.F.,.F.,(4,1,1,1,1,1,
1,4),(78.5398163397448,78.9056897408578,79.8981095810714,80.8905294212851,
81.8829492614987,82.8753691017123,83.867788941926,84.8230016469244),
 .UNSPECIFIED.);
#2435=B_SPLINE_CURVE_WITH_KNOTS('',3,(#20964,#20965,#20966,#20967,#20968,
#20969,#20970,#20971,#20972,#20973,#20974),.UNSPECIFIED.,.F.,.F.,(4,1,1,
1,1,1,1,1,4),(72.2566310325652,72.3965991153393,73.3890189555529,74.3814387957665,
75.3738586359802,76.3662784761938,77.3586983164074,78.3511181566211,78.5398163397448),
 .UNSPECIFIED.);
#2436=B_SPLINE_CURVE_WITH_KNOTS('',3,(#20975,#20976,#20977,#20978,#20979,
#20980,#20981,#20982,#20983,#20984),.UNSPECIFIED.,.F.,.F.,(4,1,1,1,1,1,
1,4),(72.2566310325652,72.951170699576,73.9435905397896,74.9360103800033,
75.9284302202169,76.9208500604305,77.9132699006442,78.5398163397448),
 .UNSPECIFIED.);
#2437=B_SPLINE_CURVE_WITH_KNOTS('',3,(#20989,#20990,#20991,#20992,#20993,
#20994,#20995,#20996,#20997,#20998),.UNSPECIFIED.,.F.,.F.,(4,1,1,1,1,1,
1,4),(65.9734457253856,66.4420800740575,67.4344999142711,68.4269197544847,
69.4193395946984,70.411759434912,71.4041792751256,72.2566310325652),
 .UNSPECIFIED.);
#2438=B_SPLINE_CURVE_WITH_KNOTS('',3,(#20999,#21000,#21001,#21002,#21003,
#21004,#21005,#21006,#21007,#21008,#21009),.UNSPECIFIED.,.F.,.F.,(4,1,1,
1,1,1,1,1,4),(65.9734457253856,66.0042318180806,66.9966516582942,67.9890714985079,
68.9814913387215,69.9739111789351,70.9663310191488,71.9587508593624,72.2566310325652),
 .UNSPECIFIED.);
#2439=B_SPLINE_CURVE_WITH_KNOTS('',3,(#21014,#21015,#21016,#21017,#21018,
#21019,#21020,#21021,#21022,#21023),.UNSPECIFIED.,.F.,.F.,(4,1,1,1,1,1,
1,4),(59.690260418206,60.4875610327757,61.4799808729893,62.4724007132029,
63.4648205534166,64.4572403936302,65.4496602338438,65.9734457253856),
 .UNSPECIFIED.);
#2440=B_SPLINE_CURVE_WITH_KNOTS('',3,(#21024,#21025,#21026,#21027,#21028,
#21029,#21030,#21031,#21032,#21033),.UNSPECIFIED.,.F.,.F.,(4,1,1,1,1,1,
1,4),(59.690260418206,60.0497127767988,61.0421326170124,62.0345524572261,
63.0269722974397,64.0193921376533,65.011811977867,65.9734457253856),
 .UNSPECIFIED.);
#2441=B_SPLINE_CURVE_WITH_KNOTS('',3,(#21038,#21039,#21040,#21041,#21042,
#21043,#21044,#21045,#21046,#21047,#21048),.UNSPECIFIED.,.F.,.F.,(4,1,1,
1,1,1,1,1,4),(53.4070751110264,53.5406221512803,54.5330419914939,55.5254618317075,
56.5178816719212,57.5103015121348,58.5027213523484,59.4951411925621,59.690260418206),
 .UNSPECIFIED.);
#2442=B_SPLINE_CURVE_WITH_KNOTS('',3,(#21049,#21050,#21051,#21052,#21053,
#21054,#21055,#21056,#21057,#21058),.UNSPECIFIED.,.F.,.F.,(4,1,1,1,1,1,
1,4),(53.4070751110264,54.095193735517,55.0876135757306,56.0800334159443,
57.0724532561579,58.0648730963715,59.0572929365852,59.690260418206),
 .UNSPECIFIED.);
#2443=B_SPLINE_CURVE_WITH_KNOTS('',3,(#21063,#21064,#21065,#21066,#21067,
#21068,#21069,#21070,#21071,#21072),.UNSPECIFIED.,.F.,.F.,(4,1,1,1,1,1,
1,4),(47.1238898038468,47.5861031099985,48.5785229502121,49.5709427904257,
50.5633626306394,51.555782470853,52.5482023110666,53.4070751110264),
 .UNSPECIFIED.);
#2444=B_SPLINE_CURVE_WITH_KNOTS('',3,(#21073,#21074,#21075,#21076,#21077,
#21078,#21079,#21080,#21081,#21082,#21083),.UNSPECIFIED.,.F.,.F.,(4,1,1,
1,1,1,1,1,4),(47.1238898038468,47.1482548540216,48.1406746942352,49.1330945344489,
50.1255143746625,51.1179342148761,52.1103540550898,53.1027738953034,53.4070751110264),
 .UNSPECIFIED.);
#2445=B_SPLINE_CURVE_WITH_KNOTS('',3,(#21088,#21089,#21090,#21091,#21092,
#21093,#21094,#21095,#21096,#21097),.UNSPECIFIED.,.F.,.F.,(4,1,1,1,1,1,
1,4),(40.8407044966672,41.6315840687167,42.6240039089303,43.6164237491439,
44.6088435893576,45.6012634295712,46.5936832697848,47.1238898038468),
 .UNSPECIFIED.);
#2446=B_SPLINE_CURVE_WITH_KNOTS('',3,(#21098,#21099,#21100,#21101,#21102,
#21103,#21104,#21105,#21106,#21107),.UNSPECIFIED.,.F.,.F.,(4,1,1,1,1,1,
1,4),(40.8407044966672,41.1937358127398,42.1861556529534,43.1785754931671,
44.1709953333807,45.1634151735943,46.155835013808,47.1238898038468),
 .UNSPECIFIED.);
#2447=B_SPLINE_CURVE_WITH_KNOTS('',3,(#21112,#21113,#21114,#21115,#21116,
#21117,#21118,#21119,#21120,#21121,#21122),.UNSPECIFIED.,.F.,.F.,(4,1,1,
1,1,1,1,1,4),(34.5575191894876,34.6846451872213,35.6770650274349,36.6694848676485,
37.6619047078622,38.6543245480758,39.6467443882894,40.639164228503,40.8407044966672),
 .UNSPECIFIED.);
#2448=B_SPLINE_CURVE_WITH_KNOTS('',3,(#21123,#21124,#21125,#21126,#21127,
#21128,#21129,#21130,#21131,#21132),.UNSPECIFIED.,.F.,.F.,(4,1,1,1,1,1,
1,4),(34.5575191894876,35.239216771458,36.2316366116717,37.2240564518853,
38.2164762920989,39.2088961323126,40.2013159725262,40.8407044966672),
 .UNSPECIFIED.);
#2449=B_SPLINE_CURVE_WITH_KNOTS('',3,(#21137,#21138,#21139,#21140,#21141,
#21142,#21143,#21144,#21145,#21146),.UNSPECIFIED.,.F.,.F.,(4,1,1,1,1,1,
1,4),(28.274333882308,28.7301261459395,29.7225459861531,30.7149658263667,
31.7073856665804,32.699805506794,33.6922253470076,34.5575191894876),
 .UNSPECIFIED.);
#2450=B_SPLINE_CURVE_WITH_KNOTS('',3,(#21147,#21148,#21149,#21150,#21151,
#21152,#21153,#21154,#21155,#21156,#21157),.UNSPECIFIED.,.F.,.F.,(4,1,1,
1,1,1,1,1,4),(28.274333882308,28.2922778899626,29.2846977301762,30.2771175703899,
31.2695374106035,32.2619572508171,33.2543770910308,34.2467969312444,34.5575191894876),
 .UNSPECIFIED.);
#2451=B_SPLINE_CURVE_WITH_KNOTS('',3,(#21162,#21163,#21164,#21165,#21166,
#21167,#21168,#21169,#21170,#21171),.UNSPECIFIED.,.F.,.F.,(4,1,1,1,1,1,
1,4),(21.9911485751285,22.7756071046577,23.7680269448713,24.7604467850849,
25.7528666252986,26.7452864655122,27.7377063057258,28.274333882308),
 .UNSPECIFIED.);
#2452=B_SPLINE_CURVE_WITH_KNOTS('',3,(#21172,#21173,#21174,#21175,#21176,
#21177,#21178,#21179,#21180,#21181),.UNSPECIFIED.,.F.,.F.,(4,1,1,1,1,1,
1,4),(21.9911485751285,22.3377588486808,23.3301786888945,24.3225985291081,
25.3150183693217,26.3074382095353,27.299858049749,28.274333882308),
 .UNSPECIFIED.);
#2453=B_SPLINE_CURVE_WITH_KNOTS('',3,(#21187,#21188,#21189,#21190,#21191),
 .UNSPECIFIED.,.F.,.F.,(4,1,4),(14.3984001269718,15.3908199671854,15.7079632679489),
 .UNSPECIFIED.);
#2454=B_SPLINE_CURVE_WITH_KNOTS('',3,(#21194,#21195,#21196,#21197,#21198),
 .UNSPECIFIED.,.F.,.F.,(4,1,4),(13.8759337553362,14.8362483829486,15.7079632679489),
 .UNSPECIFIED.);
#2455=B_SPLINE_CURVE_WITH_KNOTS('',3,(#21204,#21205,#21206,#21207),
 .UNSPECIFIED.,.F.,.F.,(4,4),(95.5573427486709,96.2647245007222),
 .UNSPECIFIED.);
#2456=B_SPLINE_CURVE_WITH_KNOTS('',3,(#21215,#21216,#21217,#21218,#21219,
#21220,#21221,#21222,#21223,#21224),.UNSPECIFIED.,.F.,.F.,(4,3,3,4),(-94.2477796076938,
-93.2874649800814,-92.2950451398678,-91.8135687061554),.UNSPECIFIED.);
#2457=B_SPLINE_CURVE_WITH_KNOTS('',3,(#21229,#21230,#21231,#21232,#21233,
#21234,#21235,#21236,#21237,#21238,#21239,#21240,#21241,#21242,#21243,#21244,
#21245,#21246,#21247,#21248,#21249,#21250,#21251,#21252,#21253),
 .UNSPECIFIED.,.F.,.F.,(4,3,3,3,3,3,3,3,4),(89.2741574414913,89.3177856192268,
90.3102054594404,91.3026252996541,92.2950451398677,93.2874649800813,94.279884820295,
95.2723046605086,95.5573427486709),.UNSPECIFIED.);
#2458=B_SPLINE_CURVE_WITH_KNOTS('',3,(#21254,#21255,#21256,#21257,#21258,
#21259,#21260,#21261,#21262,#21263,#21264,#21265,#21266,#21267,#21268,#21269,
#21270,#21271,#21272,#21273,#21274,#21275),.UNSPECIFIED.,.F.,.F.,(4,3,3,
3,3,3,3,4),(-91.8135687061554,-91.3026252996541,-90.3102054594405,-89.3177856192269,
-88.3253657790132,-87.3329459387996,-86.340526098586,-85.5303833989758),
 .UNSPECIFIED.);
#2459=B_SPLINE_CURVE_WITH_KNOTS('',3,(#21280,#21281,#21282,#21283,#21284,
#21285,#21286,#21287,#21288,#21289,#21290,#21291,#21292,#21293,#21294,#21295,
#21296,#21297,#21298,#21299,#21300,#21301),.UNSPECIFIED.,.F.,.F.,(4,3,3,
3,3,3,3,4),(82.9909721343117,83.363266577945,84.3556864181587,85.3481062583723,
86.3405260985859,87.3329459387996,88.3253657790132,89.2741574414913),
 .UNSPECIFIED.);
#2460=B_SPLINE_CURVE_WITH_KNOTS('',3,(#21302,#21303,#21304,#21305,#21306,
#21307,#21308,#21309,#21310,#21311,#21312,#21313,#21314,#21315,#21316,#21317,
#21318,#21319,#21320,#21321,#21322,#21323,#21324,#21325,#21326),
 .UNSPECIFIED.,.F.,.F.,(4,3,3,3,3,3,3,3,4),(-85.5303833989758,-85.3481062583723,
-84.3556864181587,-83.3632665779451,-82.3708467377314,-81.3784268975178,
-80.3860070573042,-79.3935872170905,-79.2471980917962),.UNSPECIFIED.);
#2461=B_SPLINE_CURVE_WITH_KNOTS('',3,(#21331,#21332,#21333,#21334,#21335,
#21336,#21337,#21338,#21339,#21340,#21341,#21342,#21343,#21344,#21345,#21346,
#21347,#21348,#21349,#21350,#21351,#21352),.UNSPECIFIED.,.F.,.F.,(4,3,3,
3,3,3,3,4),(76.7077868271321,77.4087475366632,78.4011673768769,79.3935872170905,
80.3860070573041,81.3784268975178,82.3708467377314,82.9909721343117),
 .UNSPECIFIED.);
#2462=B_SPLINE_CURVE_WITH_KNOTS('',3,(#21353,#21354,#21355,#21356,#21357,
#21358,#21359,#21360,#21361,#21362,#21363,#21364,#21365,#21366,#21367,#21368,
#21369,#21370,#21371,#21372,#21373,#21374),.UNSPECIFIED.,.F.,.F.,(4,3,3,
3,3,3,3,4),(-79.2471980917962,-78.4011673768769,-77.4087475366633,-76.4163276964496,
-75.423907856236,-74.4314880160224,-73.4390681758088,-72.9640127846167),
 .UNSPECIFIED.);
#2463=B_SPLINE_CURVE_WITH_KNOTS('',3,(#21379,#21380,#21381,#21382,#21383,
#21384,#21385,#21386,#21387,#21388,#21389,#21390,#21391,#21392,#21393,#21394,
#21395,#21396,#21397,#21398,#21399,#21400,#21401,#21402,#21403),
 .UNSPECIFIED.,.F.,.F.,(4,3,3,3,3,3,3,3,4),(70.4246015199525,70.4618086551678,
71.4542284953814,72.4466483355951,73.4390681758087,74.4314880160223,75.423907856236,
76.4163276964496,76.7077868271321),.UNSPECIFIED.);
#2464=B_SPLINE_CURVE_WITH_KNOTS('',3,(#21404,#21405,#21406,#21407,#21408,
#21409,#21410,#21411,#21412,#21413,#21414,#21415,#21416,#21417,#21418,#21419,
#21420,#21421,#21422,#21423,#21424,#21425),.UNSPECIFIED.,.F.,.F.,(4,3,3,
3,3,3,3,4),(-72.9640127846167,-72.4466483355951,-71.4542284953815,-70.4618086551678,
-69.4693888149542,-68.4769689747406,-67.4845491345269,-66.680827477437),
 .UNSPECIFIED.);
#2465=B_SPLINE_CURVE_WITH_KNOTS('',3,(#21430,#21431,#21432,#21433,#21434,
#21435,#21436,#21437,#21438,#21439,#21440,#21441,#21442,#21443,#21444,#21445,
#21446,#21447,#21448,#21449,#21450,#21451),.UNSPECIFIED.,.F.,.F.,(4,3,3,
3,3,3,3,4),(64.1414162127729,64.507289613886,65.4997094540997,66.4921292943133,
67.4845491345269,68.4769689747405,69.4693888149542,70.4246015199525),
 .UNSPECIFIED.);
#2466=B_SPLINE_CURVE_WITH_KNOTS('',3,(#21452,#21453,#21454,#21455,#21456,
#21457,#21458,#21459,#21460,#21461,#21462,#21463,#21464,#21465,#21466,#21467,
#21468,#21469,#21470,#21471,#21472,#21473,#21474,#21475,#21476),
 .UNSPECIFIED.,.F.,.F.,(4,3,3,3,3,3,3,3,4),(-66.680827477437,-66.4921292943133,
-65.4997094540997,-64.5072896138861,-63.5148697736724,-62.5224499334588,
-61.5300300932452,-60.5376102530315,-60.3976421702575),.UNSPECIFIED.);
#2467=B_SPLINE_CURVE_WITH_KNOTS('',3,(#21481,#21482,#21483,#21484,#21485,
#21486,#21487,#21488,#21489,#21490,#21491,#21492,#21493,#21494,#21495,#21496,
#21497,#21498,#21499,#21500,#21501,#21502),.UNSPECIFIED.,.F.,.F.,(4,3,3,
3,3,3,3,4),(57.8582309055933,58.5527705726042,59.5451904128179,60.5376102530315,
61.5300300932451,62.5224499334588,63.5148697736724,64.1414162127729),
 .UNSPECIFIED.);
#2468=B_SPLINE_CURVE_WITH_KNOTS('',3,(#21503,#21504,#21505,#21506,#21507,
#21508,#21509,#21510,#21511,#21512,#21513,#21514,#21515,#21516,#21517,#21518,
#21519,#21520,#21521,#21522,#21523,#21524),.UNSPECIFIED.,.F.,.F.,(4,3,3,
3,3,3,3,4),(-60.3976421702575,-59.5451904128179,-58.5527705726043,-57.5603507323906,
-56.567930892177,-55.5755110519634,-54.5830912117497,-54.1144568630779),
 .UNSPECIFIED.);
#2469=B_SPLINE_CURVE_WITH_KNOTS('',3,(#21529,#21530,#21531,#21532,#21533,
#21534,#21535,#21536,#21537,#21538,#21539,#21540,#21541,#21542,#21543,#21544,
#21545,#21546,#21547,#21548,#21549,#21550,#21551,#21552,#21553),
 .UNSPECIFIED.,.F.,.F.,(4,3,3,3,3,3,3,3,4),(51.5750455984138,51.6058316911088,
52.5982515313225,53.5906713715361,54.5830912117497,55.5755110519634,56.567930892177,
57.5603507323906,57.8582309055933),.UNSPECIFIED.);
#2470=B_SPLINE_CURVE_WITH_KNOTS('',3,(#21554,#21555,#21556,#21557,#21558,
#21559,#21560,#21561,#21562,#21563,#21564,#21565,#21566,#21567,#21568,#21569,
#21570,#21571,#21572,#21573,#21574,#21575),.UNSPECIFIED.,.F.,.F.,(4,3,3,
3,3,3,3,4),(-54.1144568630779,-53.5906713715361,-52.5982515313225,-51.6058316911088,
-50.6134118508952,-49.6209920106816,-48.6285721704679,-47.8312715558983),
 .UNSPECIFIED.);
#2471=B_SPLINE_CURVE_WITH_KNOTS('',3,(#21580,#21581,#21582,#21583,#21584,
#21585,#21586,#21587,#21588,#21589,#21590,#21591,#21592,#21593,#21594,#21595,
#21596,#21597,#21598,#21599,#21600,#21601),.UNSPECIFIED.,.F.,.F.,(4,3,3,
3,3,3,3,4),(45.2918602912342,45.651312649827,46.6437324900407,47.6361523302543,
48.6285721704679,49.6209920106816,50.6134118508952,51.5750455984138),
 .UNSPECIFIED.);
#2472=B_SPLINE_CURVE_WITH_KNOTS('',3,(#21602,#21603,#21604,#21605,#21606,
#21607,#21608,#21609,#21610,#21611,#21612,#21613,#21614,#21615,#21616,#21617,
#21618,#21619,#21620,#21621,#21622,#21623,#21624,#21625,#21626),
 .UNSPECIFIED.,.F.,.F.,(4,3,3,3,3,3,3,3,4),(-47.8312715558983,-47.6361523302543,
-46.6437324900407,-45.651312649827,-44.6588928096134,-43.6664729693998,
-42.6740531291862,-41.6816332889725,-41.5480862487187),.UNSPECIFIED.);
#2473=B_SPLINE_CURVE_WITH_KNOTS('',3,(#21631,#21632,#21633,#21634,#21635,
#21636,#21637,#21638,#21639,#21640,#21641,#21642,#21643,#21644,#21645,#21646,
#21647,#21648,#21649,#21650,#21651,#21652),.UNSPECIFIED.,.F.,.F.,(4,3,3,
3,3,3,3,4),(39.0086749840546,39.6967936085453,40.6892134487589,41.6816332889725,
42.6740531291861,43.6664729693998,44.6588928096134,45.2918602912342),
 .UNSPECIFIED.);
#2474=B_SPLINE_CURVE_WITH_KNOTS('',3,(#21653,#21654,#21655,#21656,#21657,
#21658,#21659,#21660,#21661,#21662,#21663,#21664,#21665,#21666,#21667,#21668,
#21669,#21670,#21671,#21672,#21673,#21674),.UNSPECIFIED.,.F.,.F.,(4,3,3,
3,3,3,3,4),(-41.5480862487187,-40.6892134487589,-39.6967936085453,-38.7043737683316,
-37.711953928118,-36.7195340879044,-35.7271142476907,-35.2649009415391),
 .UNSPECIFIED.);
#2475=B_SPLINE_CURVE_WITH_KNOTS('',3,(#21679,#21680,#21681,#21682,#21683,
#21684,#21685,#21686,#21687,#21688,#21689,#21690,#21691,#21692,#21693,#21694,
#21695,#21696,#21697,#21698,#21699,#21700,#21701,#21702,#21703),
 .UNSPECIFIED.,.F.,.F.,(4,3,3,3,3,3,3,3,4),(32.725489676875,32.7498547270498,
33.7422745672635,34.7346944074771,35.7271142476907,36.7195340879043,37.711953928118,
38.7043737683316,39.0086749840546),.UNSPECIFIED.);
#2476=B_SPLINE_CURVE_WITH_KNOTS('',3,(#21704,#21705,#21706,#21707,#21708,
#21709,#21710,#21711,#21712,#21713,#21714,#21715,#21716,#21717,#21718,#21719,
#21720,#21721,#21722,#21723,#21724,#21725),.UNSPECIFIED.,.F.,.F.,(4,3,3,
3,3,3,3,4),(-35.2649009415391,-34.7346944074771,-33.7422745672635,-32.7498547270498,
-31.7574348868362,-30.7650150466226,-29.7725952064089,-28.9817156343595),
 .UNSPECIFIED.);
#2477=B_SPLINE_CURVE_WITH_KNOTS('',3,(#21730,#21731,#21732,#21733,#21734,
#21735,#21736,#21737,#21738,#21739,#21740,#21741,#21742,#21743,#21744,#21745,
#21746,#21747,#21748,#21749,#21750,#21751),.UNSPECIFIED.,.F.,.F.,(4,3,3,
3,3,3,3,4),(26.4423043696954,26.795335685768,27.7877555259817,28.7801753661953,
29.7725952064089,30.7650150466226,31.7574348868362,32.725489676875),
 .UNSPECIFIED.);
#2478=B_SPLINE_CURVE_WITH_KNOTS('',3,(#21752,#21753,#21754,#21755,#21756,
#21757,#21758,#21759,#21760,#21761,#21762,#21763,#21764,#21765,#21766,#21767,
#21768,#21769,#21770,#21771,#21772,#21773,#21774,#21775,#21776),
 .UNSPECIFIED.,.F.,.F.,(4,3,3,3,3,3,3,3,4),(-28.9817156343595,-28.7801753661953,
-27.7877555259817,-26.7953356857681,-25.8029158455544,-24.8104960053408,
-23.8180761651272,-22.8256563249135,-22.6985303271799),.UNSPECIFIED.);
#2479=B_SPLINE_CURVE_WITH_KNOTS('',3,(#21781,#21782,#21783,#21784,#21785,
#21786,#21787,#21788,#21789,#21790,#21791,#21792,#21793,#21794,#21795,#21796,
#21797,#21798,#21799,#21800,#21801,#21802),.UNSPECIFIED.,.F.,.F.,(4,3,3,
3,3,3,3,4),(20.1591190625158,20.8408166444863,21.8332364846999,22.8256563249135,
23.8180761651272,24.8104960053408,25.8029158455544,26.4423043696954),
 .UNSPECIFIED.);
#2480=B_SPLINE_CURVE_WITH_KNOTS('',3,(#21803,#21804,#21805,#21806,#21807,
#21808,#21809,#21810,#21811,#21812,#21813,#21814,#21815,#21816,#21817,#21818,
#21819,#21820,#21821,#21822,#21823,#21824),.UNSPECIFIED.,.F.,.F.,(4,3,3,
3,3,3,3,4),(-22.6985303271799,-21.8332364846999,-20.8408166444863,-19.8483968042726,
-18.855976964059,-17.8635571238454,-16.8711372836317,-16.4153450200003),
 .UNSPECIFIED.);
#2481=B_SPLINE_CURVE_WITH_KNOTS('',3,(#21829,#21830,#21831,#21832,#21833,
#21834,#21835,#21836,#21837,#21838,#21839,#21840,#21841,#21842,#21843,#21844,
#21845,#21846,#21847,#21848,#21849,#21850,#21851,#21852,#21853),
 .UNSPECIFIED.,.F.,.F.,(4,3,3,3,3,3,3,3,4),(13.8759337553362,13.8938777629908,
14.8862976032045,15.8787174434181,16.8711372836317,17.8635571238454,18.855976964059,
19.8483968042726,20.1591190625158),.UNSPECIFIED.);
#2482=B_SPLINE_CURVE_WITH_KNOTS('',3,(#21854,#21855,#21856,#21857,#21858,
#21859,#21860,#21861,#21862,#21863,#21864,#21865,#21866,#21867,#21868,#21869,
#21870,#21871,#21872,#21873,#21874,#21875),.UNSPECIFIED.,.F.,.F.,(4,3,3,
3,3,3,3,4),(-16.4153450200003,-15.8787174434181,-14.8862976032045,-13.8938777629908,
-12.9014579227772,-11.9090380825636,-10.9166182423499,-10.1321597128207),
 .UNSPECIFIED.);
#2483=B_SPLINE_CURVE_WITH_KNOTS('',3,(#21881,#21882,#21883,#21884,#21885,
#21886,#21887,#21888,#21889,#21890,#21891,#21892,#21893),.UNSPECIFIED.,
 .F.,.F.,(4,3,3,3,4),(-3.84897440564114,-2.9772595206409,-1.98483968042726,
-0.992419840213631,0.),.UNSPECIFIED.);
#2484=B_SPLINE_CURVE_WITH_KNOTS('',3,(#21896,#21897,#21898,#21899,#21900,
#21901,#21902,#21903,#21904,#21905,#21906,#21907,#21908,#21909,#21910,#21911,
#21912,#21913,#21914),.UNSPECIFIED.,.F.,.F.,(4,3,3,3,3,3,4),(2.01694489302841,
2.97725952064089,3.96967936085452,4.96209920106815,5.95451904128178,6.94693888149541,
7.59274844815661),.UNSPECIFIED.);
#2485=B_SPLINE_CURVE_WITH_KNOTS('',3,(#21920,#21921,#21922,#21923,#21924,
#21925,#21926,#21927),.UNSPECIFIED.,.F.,.F.,(4,1,1,1,1,4),(103.672557568463,
104.154034002175,105.146453842389,106.138873682603,107.131293522816,108.12371336303),
 .UNSPECIFIED.);
#2486=B_SPLINE_CURVE_WITH_KNOTS('',3,(#21930,#21931,#21932,#21933,#21934,
#21935,#21936,#21937,#21938),.UNSPECIFIED.,.F.,.F.,(4,1,1,1,1,1,4),(103.672557568463,
103.716185746199,104.708605586412,105.701025426626,106.693445266839,107.685865107053,
108.646179734666),.UNSPECIFIED.);
#2487=B_SPLINE_CURVE_WITH_KNOTS('',3,(#21943,#21944,#21945,#21946,#21947,
#21948,#21949,#21950,#21951,#21952),.UNSPECIFIED.,.F.,.F.,(4,1,1,1,1,1,
1,4),(97.3893722612836,98.1995149608937,99.1919348011073,100.184354641321,
101.176774481535,102.169194321748,103.161614161962,103.672557568463),
 .UNSPECIFIED.);
#2488=B_SPLINE_CURVE_WITH_KNOTS('',3,(#21953,#21954,#21955,#21956,#21957,
#21958,#21959,#21960,#21961,#21962),.UNSPECIFIED.,.F.,.F.,(4,1,1,1,1,1,
1,4),(97.3893722612836,97.7616667049168,98.7540865451304,99.7465063853441,
100.738926225558,101.731346065771,102.723765905985,103.672557568463),
 .UNSPECIFIED.);
#2489=B_SPLINE_CURVE_WITH_KNOTS('',3,(#21967,#21968,#21969,#21970,#21971,
#21972,#21973,#21974,#21975,#21976,#21977),.UNSPECIFIED.,.F.,.F.,(4,1,1,
1,1,1,1,1,4),(91.106186954104,91.2525760793983,92.2449959196119,93.2374157598255,
94.2298356000392,95.2222554402528,96.2146752804664,97.2070951206801,97.3893722612836),
 .UNSPECIFIED.);
#2490=B_SPLINE_CURVE_WITH_KNOTS('',3,(#21978,#21979,#21980,#21981,#21982,
#21983,#21984,#21985,#21986,#21987),.UNSPECIFIED.,.F.,.F.,(4,1,1,1,1,1,
1,4),(91.106186954104,91.807147663635,92.7995675038486,93.7919873440623,
94.7844071842759,95.7768270244895,96.7692468647032,97.3893722612836),
 .UNSPECIFIED.);
#2491=B_SPLINE_CURVE_WITH_KNOTS('',3,(#21992,#21993,#21994,#21995,#21996,
#21997,#21998,#21999,#22000,#22001),.UNSPECIFIED.,.F.,.F.,(4,1,1,1,1,1,
1,4),(84.8230016469244,85.2980570381165,86.2904768783301,87.2828967185437,
88.2753165587574,89.267736398971,90.2601562391846,91.106186954104),
 .UNSPECIFIED.);
#2492=B_SPLINE_CURVE_WITH_KNOTS('',3,(#22002,#22003,#22004,#22005,#22006,
#22007,#22008,#22009,#22010,#22011,#22012),.UNSPECIFIED.,.F.,.F.,(4,1,1,
1,1,1,1,1,4),(84.8230016469244,84.8602087821396,85.8526286223532,86.8450484625669,
87.8374683027805,88.8298881429941,89.8223079832078,90.8147278234214,91.106186954104),
 .UNSPECIFIED.);
#2493=B_SPLINE_CURVE_WITH_KNOTS('',3,(#22017,#22018,#22019,#22020,#22021,
#22022,#22023,#22024,#22025,#22026),.UNSPECIFIED.,.F.,.F.,(4,1,1,1,1,1,
1,4),(78.5398163397448,79.3435379968347,80.3359578370483,81.328377677262,
82.3207975174756,83.3132173576892,84.3056371979029,84.8230016469244),
 .UNSPECIFIED.);
#2494=B_SPLINE_CURVE_WITH_KNOTS('',3,(#22027,#22028,#22029,#22030,#22031,
#22032,#22033,#22034,#22035,#22036),.UNSPECIFIED.,.F.,.F.,(4,1,1,1,1,1,
1,4),(78.5398163397448,78.9056897408578,79.8981095810714,80.8905294212851,
81.8829492614987,82.8753691017123,83.867788941926,84.8230016469244),
 .UNSPECIFIED.);
#2495=B_SPLINE_CURVE_WITH_KNOTS('',3,(#22041,#22042,#22043,#22044,#22045,
#22046,#22047,#22048,#22049,#22050,#22051),.UNSPECIFIED.,.F.,.F.,(4,1,1,
1,1,1,1,1,4),(72.2566310325652,72.3965991153393,73.3890189555529,74.3814387957665,
75.3738586359802,76.3662784761938,77.3586983164074,78.3511181566211,78.5398163397448),
 .UNSPECIFIED.);
#2496=B_SPLINE_CURVE_WITH_KNOTS('',3,(#22052,#22053,#22054,#22055,#22056,
#22057,#22058,#22059,#22060,#22061),.UNSPECIFIED.,.F.,.F.,(4,1,1,1,1,1,
1,4),(72.2566310325652,72.951170699576,73.9435905397896,74.9360103800033,
75.9284302202169,76.9208500604305,77.9132699006442,78.5398163397448),
 .UNSPECIFIED.);
#2497=B_SPLINE_CURVE_WITH_KNOTS('',3,(#22066,#22067,#22068,#22069,#22070,
#22071,#22072,#22073,#22074,#22075),.UNSPECIFIED.,.F.,.F.,(4,1,1,1,1,1,
1,4),(65.9734457253856,66.4420800740575,67.4344999142711,68.4269197544847,
69.4193395946984,70.411759434912,71.4041792751256,72.2566310325652),
 .UNSPECIFIED.);
#2498=B_SPLINE_CURVE_WITH_KNOTS('',3,(#22076,#22077,#22078,#22079,#22080,
#22081,#22082,#22083,#22084,#22085,#22086),.UNSPECIFIED.,.F.,.F.,(4,1,1,
1,1,1,1,1,4),(65.9734457253856,66.0042318180806,66.9966516582942,67.9890714985079,
68.9814913387215,69.9739111789351,70.9663310191488,71.9587508593624,72.2566310325652),
 .UNSPECIFIED.);
#2499=B_SPLINE_CURVE_WITH_KNOTS('',3,(#22091,#22092,#22093,#22094,#22095,
#22096,#22097,#22098,#22099,#22100),.UNSPECIFIED.,.F.,.F.,(4,1,1,1,1,1,
1,4),(59.690260418206,60.4875610327757,61.4799808729893,62.4724007132029,
63.4648205534166,64.4572403936302,65.4496602338438,65.9734457253856),
 .UNSPECIFIED.);
#2500=B_SPLINE_CURVE_WITH_KNOTS('',3,(#22101,#22102,#22103,#22104,#22105,
#22106,#22107,#22108,#22109,#22110),.UNSPECIFIED.,.F.,.F.,(4,1,1,1,1,1,
1,4),(59.690260418206,60.0497127767988,61.0421326170124,62.0345524572261,
63.0269722974397,64.0193921376533,65.011811977867,65.9734457253856),
 .UNSPECIFIED.);
#2501=B_SPLINE_CURVE_WITH_KNOTS('',3,(#22115,#22116,#22117,#22118,#22119,
#22120,#22121,#22122,#22123,#22124,#22125),.UNSPECIFIED.,.F.,.F.,(4,1,1,
1,1,1,1,1,4),(53.4070751110264,53.5406221512803,54.5330419914939,55.5254618317075,
56.5178816719212,57.5103015121348,58.5027213523484,59.4951411925621,59.690260418206),
 .UNSPECIFIED.);
#2502=B_SPLINE_CURVE_WITH_KNOTS('',3,(#22126,#22127,#22128,#22129,#22130,
#22131,#22132,#22133,#22134,#22135),.UNSPECIFIED.,.F.,.F.,(4,1,1,1,1,1,
1,4),(53.4070751110264,54.095193735517,55.0876135757306,56.0800334159443,
57.0724532561579,58.0648730963715,59.0572929365852,59.690260418206),
 .UNSPECIFIED.);
#2503=B_SPLINE_CURVE_WITH_KNOTS('',3,(#22140,#22141,#22142,#22143,#22144,
#22145,#22146,#22147,#22148,#22149),.UNSPECIFIED.,.F.,.F.,(4,1,1,1,1,1,
1,4),(47.1238898038468,47.5861031099985,48.5785229502121,49.5709427904257,
50.5633626306394,51.555782470853,52.5482023110666,53.4070751110264),
 .UNSPECIFIED.);
#2504=B_SPLINE_CURVE_WITH_KNOTS('',3,(#22150,#22151,#22152,#22153,#22154,
#22155,#22156,#22157,#22158,#22159,#22160),.UNSPECIFIED.,.F.,.F.,(4,1,1,
1,1,1,1,1,4),(47.1238898038468,47.1482548540216,48.1406746942352,49.1330945344489,
50.1255143746625,51.1179342148761,52.1103540550898,53.1027738953034,53.4070751110264),
 .UNSPECIFIED.);
#2505=B_SPLINE_CURVE_WITH_KNOTS('',3,(#22165,#22166,#22167,#22168,#22169,
#22170,#22171,#22172,#22173,#22174),.UNSPECIFIED.,.F.,.F.,(4,1,1,1,1,1,
1,4),(40.8407044966672,41.6315840687167,42.6240039089303,43.6164237491439,
44.6088435893576,45.6012634295712,46.5936832697848,47.1238898038468),
 .UNSPECIFIED.);
#2506=B_SPLINE_CURVE_WITH_KNOTS('',3,(#22175,#22176,#22177,#22178,#22179,
#22180,#22181,#22182,#22183,#22184),.UNSPECIFIED.,.F.,.F.,(4,1,1,1,1,1,
1,4),(40.8407044966673,41.1937358127398,42.1861556529534,43.1785754931671,
44.1709953333807,45.1634151735943,46.155835013808,47.1238898038468),
 .UNSPECIFIED.);
#2507=B_SPLINE_CURVE_WITH_KNOTS('',3,(#22189,#22190,#22191,#22192,#22193,
#22194,#22195,#22196,#22197,#22198,#22199),.UNSPECIFIED.,.F.,.F.,(4,1,1,
1,1,1,1,1,4),(34.5575191894876,34.6846451872213,35.6770650274349,36.6694848676485,
37.6619047078622,38.6543245480758,39.6467443882894,40.639164228503,40.8407044966672),
 .UNSPECIFIED.);
#2508=B_SPLINE_CURVE_WITH_KNOTS('',3,(#22200,#22201,#22202,#22203,#22204,
#22205,#22206,#22207,#22208,#22209),.UNSPECIFIED.,.F.,.F.,(4,1,1,1,1,1,
1,4),(34.5575191894877,35.239216771458,36.2316366116717,37.2240564518853,
38.2164762920989,39.2088961323126,40.2013159725262,40.8407044966673),
 .UNSPECIFIED.);
#2509=B_SPLINE_CURVE_WITH_KNOTS('',3,(#22214,#22215,#22216,#22217,#22218,
#22219,#22220,#22221,#22222,#22223),.UNSPECIFIED.,.F.,.F.,(4,1,1,1,1,1,
1,4),(28.274333882308,28.7301261459395,29.7225459861531,30.7149658263667,
31.7073856665804,32.699805506794,33.6922253470076,34.5575191894876),
 .UNSPECIFIED.);
#2510=B_SPLINE_CURVE_WITH_KNOTS('',3,(#22224,#22225,#22226,#22227,#22228,
#22229,#22230,#22231,#22232,#22233,#22234),.UNSPECIFIED.,.F.,.F.,(4,1,1,
1,1,1,1,1,4),(28.2743338823081,28.2922778899626,29.2846977301762,30.2771175703899,
31.2695374106035,32.2619572508171,33.2543770910308,34.2467969312444,34.5575191894877),
 .UNSPECIFIED.);
#2511=B_SPLINE_CURVE_WITH_KNOTS('',3,(#22239,#22240,#22241,#22242,#22243,
#22244,#22245,#22246,#22247,#22248),.UNSPECIFIED.,.F.,.F.,(4,1,1,1,1,1,
1,4),(21.9911485751285,22.7756071046577,23.7680269448713,24.7604467850849,
25.7528666252986,26.7452864655122,27.7377063057258,28.274333882308),
 .UNSPECIFIED.);
#2512=B_SPLINE_CURVE_WITH_KNOTS('',3,(#22249,#22250,#22251,#22252,#22253,
#22254,#22255,#22256,#22257,#22258),.UNSPECIFIED.,.F.,.F.,(4,1,1,1,1,1,
1,4),(21.9911485751285,22.3377588486808,23.3301786888945,24.3225985291081,
25.3150183693217,26.3074382095353,27.299858049749,28.2743338823081),
 .UNSPECIFIED.);
#2513=B_SPLINE_CURVE_WITH_KNOTS('',3,(#22264,#22265,#22266,#22267,#22268),
 .UNSPECIFIED.,.F.,.F.,(4,1,4),(14.3984001269718,15.3908199671854,15.7079632679489),
 .UNSPECIFIED.);
#2514=B_SPLINE_CURVE_WITH_KNOTS('',3,(#22271,#22272,#22273,#22274,#22275),
 .UNSPECIFIED.,.F.,.F.,(4,1,4),(13.8759337553362,14.8362483829486,15.7079632679489),
 .UNSPECIFIED.);
#2515=B_SPLINE_CURVE_WITH_KNOTS('',3,(#22281,#22282,#22283,#22284,#22285,
#22286,#22287,#22288,#22289,#22290,#22291,#22292,#22293,#22294,#22295,#22296,
#22297,#22298,#22299,#22300,#22301,#22302,#22303,#22304,#22305),
 .UNSPECIFIED.,.F.,.F.,(4,3,3,3,3,3,3,3,4),(-3.86106640140271,-3.4533318021373,
-2.95999868754626,-2.46666557295522,-1.97333245836417,-1.47999934377313,
-0.986666229182085,-0.493333114591042,0.),.UNSPECIFIED.);
#2516=B_SPLINE_CURVE_WITH_KNOTS('',3,(#22308,#22309,#22310,#22311,#22312,
#22313,#22314,#22315,#22316,#22317,#22318,#22319,#22320,#22321,#22322,#22323,
#22324,#22325,#22326,#22327,#22328,#22329,#22330,#22331,#22332,#22333,#22334,
#22335,#22336,#22337,#22338,#22339,#22340,#22341,#22342,#22343,#22344),
 .UNSPECIFIED.,.F.,.F.,(4,3,3,3,3,3,3,3,3,3,3,3,4),(2.02782768921384,2.46666557295522,
2.95999868754626,3.45333180213731,3.94666491672835,4.43999803131939,4.93333114591043,
5.42666426050148,5.91999737509252,6.41333048968356,6.90666360427461,7.39999671886565,
7.59153924858053),.UNSPECIFIED.);
#2517=B_SPLINE_CURVE_WITH_KNOTS('',3,(#22349,#22350,#22351,#22352,#22353,
#22354,#22355,#22356,#22357,#22358,#22359,#22360,#22361,#22362,#22363,#22364,
#22365,#22366,#22367,#22368,#22369,#22370,#22371,#22372,#22373,#22374,#22375,
#22376,#22377,#22378,#22379,#22380,#22381,#22382,#22383,#22384,#22385,#22386,
#22387,#22388,#22389,#22390,#22391),.UNSPECIFIED.,.F.,.F.,(4,3,3,3,3,3,
3,3,3,3,3,3,3,3,4),(-10.1442517085823,-9.86666229182086,-9.37332917722982,
-8.87999606263878,-8.38666294804773,-7.89332983345669,-7.39999671886565,
-6.9066636042746,-6.41333048968356,-5.91999737509252,-5.42666426050147,
-4.93333114591043,-4.43999803131939,-3.94666491672835,-3.86106640140271),
 .UNSPECIFIED.);
#2518=B_SPLINE_CURVE_WITH_KNOTS('',3,(#22392,#22393,#22394,#22395,#22396,
#22397,#22398,#22399,#22400,#22401,#22402,#22403,#22404,#22405,#22406,#22407,
#22408,#22409,#22410,#22411,#22412,#22413,#22414,#22415,#22416,#22417,#22418,
#22419,#22420,#22421,#22422,#22423,#22424,#22425,#22426,#22427,#22428,#22429,
#22430,#22431,#22432,#22433,#22434),.UNSPECIFIED.,.F.,.F.,(4,3,3,3,3,3,
3,3,3,3,3,3,3,3,4),(7.59153924858053,7.89332983345669,8.38666294804774,
8.87999606263878,9.37332917722982,9.86666229182087,10.3599954064119,10.853328521003,
11.346661635594,11.839994750185,12.3333278647761,12.8266609793671,13.3199940939582,
13.8133272085492,13.8747245557601),.UNSPECIFIED.);
#2519=B_SPLINE_CURVE_WITH_KNOTS('',3,(#22439,#22440,#22441,#22442,#22443,
#22444,#22445,#22446,#22447,#22448,#22449,#22450,#22451,#22452,#22453,#22454,
#22455,#22456,#22457,#22458,#22459,#22460,#22461,#22462,#22463,#22464,#22465,
#22466,#22467,#22468,#22469,#22470,#22471,#22472,#22473,#22474,#22475,#22476,
#22477,#22478,#22479,#22480,#22481),.UNSPECIFIED.,.F.,.F.,(4,3,3,3,3,3,
3,3,3,3,3,3,3,3,4),(-16.4274370157619,-16.2799927815044,-15.7866596669134,
-15.2933265523223,-14.7999934377313,-14.3066603231402,-13.8133272085492,
-13.3199940939582,-12.8266609793671,-12.3333278647761,-11.839994750185,
-11.346661635594,-10.8533285210029,-10.3599954064119,-10.1442517085823),
 .UNSPECIFIED.);
#2520=B_SPLINE_CURVE_WITH_KNOTS('',3,(#22482,#22483,#22484,#22485,#22486,
#22487,#22488,#22489,#22490,#22491,#22492,#22493,#22494,#22495,#22496,#22497,
#22498,#22499,#22500,#22501,#22502,#22503,#22504,#22505,#22506,#22507,#22508,
#22509,#22510,#22511,#22512,#22513,#22514,#22515,#22516,#22517,#22518,#22519,
#22520,#22521),.UNSPECIFIED.,.F.,.F.,(4,3,3,3,3,3,3,3,3,3,3,3,3,4),(13.8747245557601,
14.3066603231403,14.7999934377313,15.2933265523223,15.7866596669134,16.2799927815044,
16.7733258960955,17.2666590106865,17.7599921252775,18.2533252398686,18.7466583544596,
19.2399914690507,19.7333245836417,20.1579098629397),.UNSPECIFIED.);
#2521=B_SPLINE_CURVE_WITH_KNOTS('',3,(#22526,#22527,#22528,#22529,#22530,
#22531,#22532,#22533,#22534,#22535,#22536,#22537,#22538,#22539,#22540,#22541,
#22542,#22543,#22544,#22545,#22546,#22547,#22548,#22549,#22550,#22551,#22552,
#22553,#22554,#22555,#22556,#22557,#22558,#22559,#22560,#22561,#22562,#22563,
#22564,#22565,#22566,#22567,#22568),.UNSPECIFIED.,.F.,.F.,(4,3,3,3,3,3,
3,3,3,3,3,3,3,3,4),(-22.7106223229415,-22.693323271188,-22.1999901565969,
-21.7066570420059,-21.2133239274149,-20.7199908128238,-20.2266576982328,
-19.7333245836417,-19.2399914690507,-18.7466583544596,-18.2533252398686,
-17.7599921252776,-17.2666590106865,-16.7733258960955,-16.4274370157619),
 .UNSPECIFIED.);
#2522=B_SPLINE_CURVE_WITH_KNOTS('',3,(#22569,#22570,#22571,#22572,#22573,
#22574,#22575,#22576,#22577,#22578,#22579,#22580,#22581,#22582,#22583,#22584,
#22585,#22586,#22587,#22588,#22589,#22590,#22591,#22592,#22593,#22594,#22595,
#22596,#22597,#22598,#22599,#22600,#22601,#22602,#22603,#22604,#22605,#22606,
#22607,#22608,#22609,#22610,#22611),.UNSPECIFIED.,.F.,.F.,(4,3,3,3,3,3,
3,3,3,3,3,3,3,3,4),(20.1579098629397,20.2266576982328,20.7199908128238,
21.2133239274148,21.7066570420059,22.1999901565969,22.693323271188,23.186656385779,
23.6799895003701,24.1733226149611,24.6666557295522,25.1599888441432,25.6533219587342,
26.1466550733253,26.4410951701193),.UNSPECIFIED.);
#2523=B_SPLINE_CURVE_WITH_KNOTS('',3,(#22616,#22617,#22618,#22619,#22620,
#22621,#22622,#22623,#22624,#22625,#22626,#22627,#22628,#22629,#22630,#22631,
#22632,#22633,#22634,#22635,#22636,#22637,#22638,#22639,#22640,#22641,#22642,
#22643,#22644,#22645,#22646,#22647,#22648,#22649,#22650,#22651,#22652,#22653,
#22654,#22655),.UNSPECIFIED.,.F.,.F.,(4,3,3,3,3,3,3,3,3,3,3,3,3,4),(-28.9938076301211,
-28.6133206462805,-28.1199875316895,-27.6266544170984,-27.1333213025074,
-26.6399881879163,-26.1466550733253,-25.6533219587342,-25.1599888441432,
-24.6666557295522,-24.1733226149611,-23.6799895003701,-23.186656385779,
-22.7106223229415),.UNSPECIFIED.);
#2524=B_SPLINE_CURVE_WITH_KNOTS('',3,(#22656,#22657,#22658,#22659,#22660,
#22661,#22662,#22663,#22664,#22665,#22666,#22667,#22668,#22669,#22670,#22671,
#22672,#22673,#22674,#22675,#22676,#22677,#22678,#22679,#22680,#22681,#22682,
#22683,#22684,#22685,#22686,#22687,#22688,#22689,#22690,#22691,#22692,#22693,
#22694,#22695,#22696,#22697,#22698),.UNSPECIFIED.,.F.,.F.,(4,3,3,3,3,3,
3,3,3,3,3,3,3,3,4),(26.4410951701193,26.6399881879163,27.1333213025074,
27.6266544170984,28.1199875316895,28.6133206462805,29.1066537608716,29.5999868754626,
30.0933199900536,30.5866531046447,31.0799862192357,31.5733193338268,32.0666524484178,
32.5599855630089,32.7242804772989),.UNSPECIFIED.);
#2525=B_SPLINE_CURVE_WITH_KNOTS('',3,(#22703,#22704,#22705,#22706,#22707,
#22708,#22709,#22710,#22711,#22712,#22713,#22714,#22715,#22716,#22717,#22718,
#22719,#22720,#22721,#22722,#22723,#22724,#22725,#22726,#22727,#22728,#22729,
#22730,#22731,#22732,#22733,#22734,#22735,#22736,#22737,#22738,#22739,#22740,
#22741,#22742,#22743,#22744,#22745),.UNSPECIFIED.,.F.,.F.,(4,3,3,3,3,3,
3,3,3,3,3,3,3,3,4),(-35.2769929373007,-35.0266511359641,-34.533318021373,
-34.039984906782,-33.5466517921909,-33.0533186775999,-32.5599855630088,
-32.0666524484178,-31.5733193338268,-31.0799862192357,-30.5866531046447,
-30.0933199900536,-29.5999868754626,-29.1066537608715,-28.9938076301211),
 .UNSPECIFIED.);
#2526=B_SPLINE_CURVE_WITH_KNOTS('',3,(#22746,#22747,#22748,#22749,#22750,
#22751,#22752,#22753,#22754,#22755,#22756,#22757,#22758,#22759,#22760,#22761,
#22762,#22763,#22764,#22765,#22766,#22767,#22768,#22769,#22770,#22771,#22772,
#22773,#22774,#22775,#22776,#22777,#22778,#22779,#22780,#22781,#22782,#22783,
#22784,#22785,#22786,#22787,#22788),.UNSPECIFIED.,.F.,.F.,(4,3,3,3,3,3,
3,3,3,3,3,3,3,3,4),(32.7242804772989,33.0533186775999,33.5466517921909,
34.039984906782,34.533318021373,35.0266511359641,35.5199842505551,36.0133173651462,
36.5066504797372,36.9999835943282,37.4933167089193,37.9866498235103,38.4799829381014,
38.9733160526924,39.0074657844785),.UNSPECIFIED.);
#2527=B_SPLINE_CURVE_WITH_KNOTS('',3,(#22793,#22794,#22795,#22796,#22797,
#22798,#22799,#22800,#22801,#22802,#22803,#22804,#22805,#22806,#22807,#22808,
#22809,#22810,#22811,#22812,#22813,#22814,#22815,#22816,#22817,#22818,#22819,
#22820,#22821,#22822,#22823,#22824,#22825,#22826,#22827,#22828,#22829,#22830,
#22831,#22832,#22833,#22834,#22835),.UNSPECIFIED.,.F.,.F.,(4,3,3,3,3,3,
3,3,3,3,3,3,3,3,4),(-41.5601782444803,-41.4399816256476,-40.9466485110566,
-40.4533153964655,-39.9599822818745,-39.4666491672834,-38.9733160526924,
-38.4799829381014,-37.9866498235103,-37.4933167089193,-36.9999835943282,
-36.5066504797372,-36.0133173651462,-35.5199842505551,-35.2769929373007),
 .UNSPECIFIED.);
#2528=B_SPLINE_CURVE_WITH_KNOTS('',3,(#22836,#22837,#22838,#22839,#22840,
#22841,#22842,#22843,#22844,#22845,#22846,#22847,#22848,#22849,#22850,#22851,
#22852,#22853,#22854,#22855,#22856,#22857,#22858,#22859,#22860,#22861,#22862,
#22863,#22864,#22865,#22866,#22867,#22868,#22869,#22870,#22871,#22872,#22873,
#22874,#22875),.UNSPECIFIED.,.F.,.F.,(4,3,3,3,3,3,3,3,3,3,3,3,3,4),(39.0074657844785,
39.4666491672835,39.9599822818745,40.4533153964655,40.9466485110566,41.4399816256476,
41.9333147402387,42.4266478548297,42.9199809694208,43.4133140840118,43.9066471986028,
44.3999803131939,44.8933134277849,45.2906510916581),.UNSPECIFIED.);
#2529=B_SPLINE_CURVE_WITH_KNOTS('',3,(#22881,#22882,#22883,#22884,#22885,
#22886,#22887),.UNSPECIFIED.,.F.,.F.,(4,3,4),(51.5738363988376,51.7999770320595,
52.2933101466506),.UNSPECIFIED.);
#2530=B_SPLINE_CURVE_WITH_KNOTS('',3,(#22890,#22891,#22892,#22893,#22894,
#22895,#22896,#22897,#22898,#22899,#22900,#22901,#22902,#22903,#22904,#22905,
#22906,#22907,#22908),.UNSPECIFIED.,.F.,.F.,(4,3,3,3,3,3,4),(-50.2654824574367,
-49.8266445736954,-49.3333114591043,-48.8399783445133,-48.3466452299222,
-47.8533121153312,-47.8433635516598),.UNSPECIFIED.);
#2531=B_SPLINE_CURVE_WITH_KNOTS('',3,(#22914,#22915,#22916,#22917,#22918,
#22919,#22920,#22921,#22922,#22923,#22924,#22925,#22926),.UNSPECIFIED.,
 .F.,.F.,(4,1,1,1,1,1,1,1,1,1,4),(59.6902604182061,59.7002089818774,60.1935420964684,
60.6868752110595,61.1802083256505,61.6735414402416,62.1668745548326,62.6602076694237,
63.1535407840147,63.6468738986057,64.1402070131968),.UNSPECIFIED.);
#2532=B_SPLINE_CURVE_WITH_KNOTS('',3,(#22929,#22930,#22931,#22932,#22933,
#22934,#22935,#22936,#22937,#22938,#22939,#22940,#22941,#22942),
 .UNSPECIFIED.,.F.,.F.,(4,1,1,1,1,1,1,1,1,1,1,4),(59.6902604182061,59.786255868924,
60.279588983515,60.7729220981061,61.2662552126971,61.7595883272881,62.2529214418792,
62.7462545564702,63.2395876710613,63.7329207856523,64.2262539002434,64.6650917839847),
 .UNSPECIFIED.);
#2533=B_SPLINE_CURVE_WITH_KNOTS('',3,(#22947,#22948,#22949,#22950,#22951,
#22952,#22953,#22954,#22955,#22956,#22957,#22958,#22959,#22960,#22961,#22962),
 .UNSPECIFIED.,.F.,.F.,(4,1,1,1,1,1,1,1,1,1,1,1,1,4),(53.4070751110265,
53.7802116067849,54.2735447213759,54.766877835967,55.260210950558,55.7535440651491,
56.2468771797401,56.7402102943311,57.2335434089222,57.7268765235132,58.2202096381043,
58.7135427526953,59.2068758672864,59.6902604182061),.UNSPECIFIED.);
#2534=B_SPLINE_CURVE_WITH_KNOTS('',3,(#22963,#22964,#22965,#22966,#22967,
#22968,#22969,#22970,#22971,#22972,#22973,#22974,#22975,#22976,#22977,#22978),
 .UNSPECIFIED.,.F.,.F.,(4,1,1,1,1,1,1,1,1,1,1,1,1,4),(53.4070751110265,
53.8662584938314,54.3595916084225,54.8529247230135,55.3462578376046,55.8395909521956,
56.3329240667867,56.8262571813777,57.3195902959688,57.8129234105598,58.3062565251508,
58.7995896397419,59.2929227543329,59.6902604182061),.UNSPECIFIED.);
#2535=B_SPLINE_CURVE_WITH_KNOTS('',3,(#22983,#22984,#22985,#22986,#22987,
#22988,#22989,#22990,#22991,#22992,#22993,#22994,#22995,#22996,#22997,#22998,
#22999),.UNSPECIFIED.,.F.,.F.,(4,1,1,1,1,1,1,1,1,1,1,1,1,1,4),(47.1238898038469,
47.3668811171013,47.8602142316924,48.3535473462834,48.8468804608745,49.3402135754655,
49.8335466900565,50.3268798046476,50.8202129192386,51.3135460338297,51.8068791484207,
52.3002122630117,52.7935453776028,53.2868784921938,53.4070751110265),
 .UNSPECIFIED.);
#2536=B_SPLINE_CURVE_WITH_KNOTS('',3,(#23000,#23001,#23002,#23003,#23004,
#23005,#23006,#23007,#23008,#23009,#23010,#23011,#23012,#23013,#23014,#23015,
#23016),.UNSPECIFIED.,.F.,.F.,(4,1,1,1,1,1,1,1,1,1,1,1,1,1,4),(47.1238898038469,
47.4529280041479,47.9462611187389,48.43959423333,48.932927347921,49.4262604625121,
49.9195935771031,50.4129266916941,50.9062598062852,51.3995929208762,51.8929260354673,
52.3862591500583,52.8795922646494,53.3729253792404,53.4070751110265),
 .UNSPECIFIED.);
#2537=B_SPLINE_CURVE_WITH_KNOTS('',3,(#23021,#23022,#23023,#23024,#23025,
#23026,#23027,#23028,#23029,#23030,#23031,#23032,#23033,#23034,#23035,#23036,
#23037),.UNSPECIFIED.,.F.,.F.,(4,1,1,1,1,1,1,1,1,1,1,1,1,1,4),(40.8407044966673,
40.9535506274178,41.4468837420088,41.9402168565998,42.4335499711909,42.9268830857819,
43.420216200373,43.913549314964,44.4068824295551,44.9002155441461,45.3935486587371,
45.8868817733282,46.3802148879192,46.8735480025103,47.1238898038469),
 .UNSPECIFIED.);
#2538=B_SPLINE_CURVE_WITH_KNOTS('',3,(#23038,#23039,#23040,#23041,#23042,
#23043,#23044,#23045,#23046,#23047,#23048,#23049,#23050,#23051,#23052,#23053,
#23054),.UNSPECIFIED.,.F.,.F.,(4,1,1,1,1,1,1,1,1,1,1,1,1,1,4),(40.8407044966673,
41.0395975144643,41.5329306290554,42.0262637436464,42.5195968582374,43.0129299728285,
43.5062630874195,43.9995962020106,44.4929293166016,44.9862624311927,45.4795955457837,
45.9729286603748,46.4662617749658,46.9595948895568,47.1238898038469),
 .UNSPECIFIED.);
#2539=B_SPLINE_CURVE_WITH_KNOTS('',3,(#23059,#23060,#23061,#23062,#23063,
#23064,#23065,#23066,#23067,#23068,#23069,#23070,#23071,#23072,#23073,#23074),
 .UNSPECIFIED.,.F.,.F.,(4,1,1,1,1,1,1,1,1,1,1,1,1,4),(34.5575191894877,
35.0335532523252,35.5268863669163,36.0202194815073,36.5135525960984,37.0068857106894,
37.5002188252805,37.9935519398715,38.4868850544625,38.9802181690536,39.4735512836446,
39.9668843982357,40.4602175128267,40.8407044966673),.UNSPECIFIED.);
#2540=B_SPLINE_CURVE_WITH_KNOTS('',3,(#23075,#23076,#23077,#23078,#23079,
#23080,#23081,#23082,#23083,#23084,#23085,#23086,#23087,#23088,#23089,#23090,
#23091),.UNSPECIFIED.,.F.,.F.,(4,1,1,1,1,1,1,1,1,1,1,1,1,1,4),(34.5575191894877,
34.6262670247808,35.1196001393718,35.6129332539629,36.1062663685539,36.5995994831449,
37.092932597736,37.586265712327,38.0795988269181,38.5729319415091,39.0662650561001,
39.5595981706912,40.0529312852822,40.5462643998733,40.8407044966673),
 .UNSPECIFIED.);
#2541=B_SPLINE_CURVE_WITH_KNOTS('',3,(#23096,#23097,#23098,#23099,#23100,
#23101,#23102,#23103,#23104,#23105,#23106,#23107,#23108,#23109,#23110,#23111,
#23112),.UNSPECIFIED.,.F.,.F.,(4,1,1,1,1,1,1,1,1,1,1,1,1,1,4),(28.2743338823081,
28.6202227626417,29.1135558772327,29.6068889918238,30.1002221064148,30.5935552210059,
31.0868883355969,31.5802214501879,32.073554564779,32.56688767937,33.0602207939611,
33.5535539085521,34.0468870231432,34.5402201377342,34.5575191894877),
 .UNSPECIFIED.);
#2542=B_SPLINE_CURVE_WITH_KNOTS('',3,(#23113,#23114,#23115,#23116,#23117,
#23118,#23119,#23120,#23121,#23122,#23123,#23124,#23125,#23126,#23127,#23128),
 .UNSPECIFIED.,.F.,.F.,(4,1,1,1,1,1,1,1,1,1,1,1,1,4),(28.2743338823081,
28.7062696496882,29.1996027642793,29.6929358788703,30.1862689934614,30.6796021080524,
31.1729352226435,31.6662683372345,32.1596014518255,32.6529345664166,33.1462676810076,
33.6396007955987,34.1329339101897,34.5575191894877),.UNSPECIFIED.);
#2543=B_SPLINE_CURVE_WITH_KNOTS('',3,(#23133,#23134,#23135,#23136,#23137,
#23138,#23139,#23140,#23141,#23142,#23143,#23144,#23145,#23146,#23147,#23148,
#23149),.UNSPECIFIED.,.F.,.F.,(4,1,1,1,1,1,1,1,1,1,1,1,1,1,4),(21.9911485751285,
22.2068922729581,22.7002253875492,23.1935585021402,23.6868916167312,24.1802247313223,
24.6735578459133,25.1668909605044,25.6602240750954,26.1535571896865,26.6468903042775,
27.1402234188686,27.6335565334596,28.1268896480506,28.2743338823081),
 .UNSPECIFIED.);
#2544=B_SPLINE_CURVE_WITH_KNOTS('',3,(#23150,#23151,#23152,#23153,#23154,
#23155,#23156,#23157,#23158,#23159,#23160,#23161,#23162,#23163,#23164,#23165,
#23166),.UNSPECIFIED.,.F.,.F.,(4,1,1,1,1,1,1,1,1,1,1,1,1,1,4),(21.9911485751285,
22.2929391600047,22.7862722745957,23.2796053891868,23.7729385037778,24.2662716183689,
24.7596047329599,25.2529378475509,25.746270962142,26.239604076733,26.7329371913241,
27.2262703059151,27.7196034205062,28.2129365350972,28.2743338823081),
 .UNSPECIFIED.);
#2545=B_SPLINE_CURVE_WITH_KNOTS('',3,(#23172,#23173,#23174,#23175,#23176,
#23177),.UNSPECIFIED.,.F.,.F.,(4,1,1,4),(14.399609326548,14.892942441139,
15.3862755557301,15.7079632679489),.UNSPECIFIED.);
#2546=B_SPLINE_CURVE_WITH_KNOTS('',3,(#23180,#23181,#23182,#23183,#23184,
#23185,#23186),.UNSPECIFIED.,.F.,.F.,(4,1,1,1,4),(13.8747245557601,14.3135624395014,
14.8068955540925,15.3002286686835,15.7079632679489),.UNSPECIFIED.);
#2547=B_SPLINE_CURVE_WITH_KNOTS('',3,(#23188,#23189,#23190,#23191,#23192,
#23193,#23194,#23195,#23196,#23197,#23198,#23199,#23200,#23201,#23202,#23203,
#23204),.UNSPECIFIED.,.F.,.F.,(4,1,1,1,1,1,1,1,1,1,1,1,1,1,4),(15.7079632679489,
15.7935617832746,16.2868948978656,16.7802280124566,17.2735611270477,17.7668942416387,
18.2602273562298,18.7535604708208,19.2468935854119,19.7402267000029,20.2335598145939,
20.726892929185,21.220226043776,21.7135591583671,21.9911485751285),
 .UNSPECIFIED.);
#2548=B_SPLINE_CURVE_WITH_KNOTS('',3,(#23205,#23206,#23207,#23208,#23209,
#23210,#23211,#23212,#23213,#23214,#23215,#23216,#23217,#23218,#23219,#23220,
#23221),.UNSPECIFIED.,.F.,.F.,(4,1,1,1,1,1,1,1,1,1,1,1,1,1,4),(15.7079632679489,
15.8796086703211,16.3729417849122,16.8662748995032,17.3596080140942,17.8529411286853,
18.3462742432763,18.8396073578674,19.3329404724584,19.8262735870495,20.3196067016405,
20.8129398162316,21.3062729308226,21.7996060454136,21.9911485751285),
 .UNSPECIFIED.);
#2549=B_SPLINE_CURVE_WITH_KNOTS('',3,(#23658,#23659,#23660,#23661,#23662,
#23663,#23664,#23665,#23666,#23667,#23668,#23669,#23670,#23671,#23672,#23673,
#23674,#23675,#23676,#23677,#23678,#23679,#23680,#23681,#23682,#23683,#23684,
#23685,#23686,#23687,#23688,#23689,#23690,#23691,#23692,#23693,#23694,#23695,
#23696,#23697,#23698,#23699,#23700,#23701,#23702,#23703,#23704,#23705,#23706,
#23707,#23708,#23709,#23710,#23711,#23712,#23713,#23714,#23715,#23716,#23717,
#23718,#23719,#23720,#23721,#23722,#23723,#23724,#23725,#23726,#23727,#23728,
#23729,#23730,#23731,#23732,#23733,#23734,#23735,#23736,#23737,#23738,#23739,
#23740,#23741,#23742,#23743,#23744,#23745,#23746,#23747,#23748,#23749,#23750,
#23751,#23752,#23753,#23754,#23755,#23756,#23757,#23758,#23759,#23760,#23761,
#23762,#23763,#23764,#23765,#23766,#23767,#23768,#23769,#23770,#23771,#23772,
#23773,#23774,#23775),.UNSPECIFIED.,.F.,.F.,(4,3,3,3,3,3,3,3,3,3,3,3,3,
3,3,3,3,3,3,3,3,3,3,3,3,3,3,3,3,3,3,3,3,3,3,3,3,3,3,4),(0.,0.0627492990436898,
0.126104878557015,0.189559165750867,0.252240710610912,0.288293603463481,
0.305992302061488,0.313657647656099,0.376040517871268,0.396452282021189,
0.458859852998567,0.521377063013053,0.583471845815152,0.608441703375899,
0.617034910983491,0.624625669288178,0.686130542524575,0.747366752808485,
0.783230706301131,0.844791963679094,0.884204320253698,0.904295818732976,
0.915687585522282,0.925544690548276,0.986118296783461,1.04668162399669,
1.10647431181231,1.16009081627592,1.20586175519752,1.21479111361079,1.22268680003196,
1.28246147175047,1.34341068572502,1.36939753329053,1.38708197012437,1.39811570618177,
1.45723390803205,1.51569706964298,1.52625832764867,1.5660690749997),
 .UNSPECIFIED.);
#2550=B_SPLINE_CURVE_WITH_KNOTS('',3,(#23776,#23777,#23778,#23779,#23780,
#23781,#23782,#23783,#23784,#23785,#23786,#23787,#23788,#23789,#23790,#23791,
#23792,#23793,#23794,#23795,#23796,#23797,#23798,#23799,#23800,#23801,#23802,
#23803,#23804,#23805,#23806,#23807,#23808,#23809,#23810,#23811,#23812,#23813,
#23814,#23815,#23816,#23817,#23818,#23819,#23820,#23821,#23822,#23823,#23824,
#23825,#23826,#23827,#23828,#23829,#23830,#23831,#23832,#23833,#23834,#23835,
#23836,#23837,#23838,#23839,#23840,#23841,#23842,#23843,#23844,#23845,#23846,
#23847,#23848,#23849,#23850,#23851,#23852,#23853,#23854,#23855,#23856,#23857,
#23858,#23859,#23860,#23861,#23862,#23863,#23864,#23865,#23866,#23867,#23868,
#23869,#23870,#23871,#23872,#23873,#23874,#23875,#23876,#23877,#23878,#23879,
#23880,#23881,#23882,#23883,#23884,#23885,#23886,#23887,#23888,#23889,#23890),
 .UNSPECIFIED.,.F.,.F.,(4,3,3,3,3,3,3,3,3,3,3,3,3,3,3,3,3,3,3,3,3,3,3,3,
3,3,3,3,3,3,3,3,3,3,3,3,3,3,4),(0.,0.0577406588992485,0.116385458548516,
0.178509073187712,0.237685128911259,0.26948382595977,0.284721470013156,
0.290885054843453,0.350989811053008,0.364879917105302,0.424389656797942,
0.484492894172679,0.544731621925967,0.569116073872798,0.578654385819093,
0.585597036801517,0.646393915917858,0.707630011320198,0.73980723750061,
0.800806777752653,0.841276065989419,0.862788429498789,0.876711500915515,
0.884407389586128,0.946057888963432,1.00815397980749,1.07016859908497,1.12456108364678,
1.17378987619966,1.18207737487297,1.1898217223955,1.2520187672784,1.3147895064124,
1.36568998582675,1.37764504908115,1.44103981650812,1.50440163169237,1.5183914240698,
1.56247950813563),.UNSPECIFIED.);
#2551=B_SPLINE_CURVE_WITH_KNOTS('',3,(#23891,#23892,#23893,#23894,#23895,
#23896,#23897,#23898,#23899,#23900,#23901,#23902,#23903,#23904,#23905,#23906,
#23907,#23908,#23909,#23910,#23911,#23912,#23913,#23914,#23915,#23916,#23917,
#23918,#23919,#23920,#23921,#23922,#23923,#23924,#23925,#23926,#23927,#23928,
#23929,#23930),.UNSPECIFIED.,.F.,.F.,(4,3,3,3,3,3,3,3,3,3,3,3,3,4),(-47.8433635516598,
-47.3599790007401,-46.8666458861491,-46.3733127715581,-45.879979656967,
-45.386646542376,-44.8933134277849,-44.3999803131939,-43.9066471986028,
-43.4133140840118,-42.9199809694207,-42.4266478548297,-41.9333147402387,
-41.5601782444803),.UNSPECIFIED.);
#2552=B_SPLINE_CURVE_WITH_KNOTS('',3,(#24367,#24368,#24369,#24370,#24371,
#24372,#24373,#24374,#24375,#24376,#24377,#24378,#24379,#24380,#24381,#24382,
#24383,#24384,#24385,#24386,#24387,#24388,#24389,#24390,#24391,#24392,#24393,
#24394,#24395,#24396,#24397,#24398,#24399,#24400,#24401,#24402,#24403,#24404,
#24405,#24406,#24407,#24408,#24409,#24410,#24411,#24412,#24413,#24414,#24415,
#24416,#24417,#24418,#24419,#24420,#24421,#24422,#24423,#24424,#24425,#24426,
#24427,#24428,#24429,#24430,#24431,#24432,#24433,#24434,#24435,#24436,#24437,
#24438,#24439,#24440,#24441,#24442,#24443,#24444,#24445,#24446,#24447,#24448,
#24449,#24450,#24451,#24452,#24453,#24454,#24455,#24456,#24457,#24458,#24459,
#24460,#24461,#24462,#24463,#24464,#24465,#24466,#24467,#24468,#24469,#24470,
#24471,#24472,#24473,#24474,#24475,#24476,#24477,#24478,#24479,#24480,#24481),
 .UNSPECIFIED.,.F.,.F.,(4,3,3,3,3,3,3,3,3,3,3,3,3,3,3,3,3,3,3,3,3,3,3,3,
3,3,3,3,3,3,3,3,3,3,3,3,3,3,4),(0.,0.0577407111586883,0.116385549588121,
0.178509141467415,0.237685182802617,0.269483866378287,0.284721532925159,
0.290885122681355,0.350989895531535,0.364879917105296,0.424389621803389,
0.484492840377873,0.544731565736105,0.56911602470667,0.578654437928008,
0.58559704689236,0.646393901436191,0.707629993882402,0.739807237500627,
0.800806786500127,0.841276073643457,0.862788446713888,0.876711473705084,
0.884407384588612,0.946057896589746,1.00815399351749,1.07016861248816,1.12456108364677,
1.17378987619965,1.18207737505914,1.18982172246769,1.25201876607222,1.31478950544163,
1.36568998509867,1.3776450487033,1.44103981654898,1.50440163107218,1.51839142406977,
1.56247950813554),.UNSPECIFIED.);
#2553=B_SPLINE_CURVE_WITH_KNOTS('',3,(#24482,#24483,#24484,#24485,#24486,
#24487,#24488,#24489,#24490,#24491,#24492,#24493,#24494,#24495,#24496,#24497,
#24498,#24499,#24500,#24501,#24502,#24503,#24504,#24505,#24506,#24507,#24508,
#24509,#24510,#24511,#24512,#24513,#24514,#24515,#24516,#24517,#24518,#24519,
#24520,#24521,#24522,#24523,#24524),.UNSPECIFIED.,.F.,.F.,(4,3,3,3,3,3,
3,3,3,3,3,3,3,3,4),(45.2906510916581,45.386646542376,45.879979656967,46.3733127715581,
46.8666458861491,47.3599790007402,47.8533121153312,48.3466452299222,48.8399783445133,
49.3333114591043,49.8266445736954,50.3199776882864,50.8133108028775,51.3066439174685,
51.5738363988376),.UNSPECIFIED.);
#2554=B_SPLINE_CURVE_WITH_KNOTS('',3,(#24525,#24526,#24527,#24528,#24529,
#24530,#24531,#24532,#24533,#24534,#24535,#24536,#24537,#24538,#24539,#24540,
#24541,#24542,#24543,#24544,#24545,#24546,#24547,#24548,#24549,#24550,#24551,
#24552,#24553,#24554,#24555,#24556,#24557,#24558,#24559,#24560,#24561,#24562,
#24563,#24564,#24565,#24566,#24567,#24568,#24569,#24570,#24571,#24572,#24573,
#24574,#24575,#24576,#24577,#24578,#24579,#24580,#24581,#24582,#24583,#24584,
#24585,#24586,#24587,#24588,#24589,#24590,#24591,#24592,#24593,#24594,#24595,
#24596,#24597,#24598,#24599,#24600,#24601,#24602,#24603,#24604,#24605,#24606,
#24607,#24608,#24609,#24610,#24611,#24612,#24613,#24614,#24615,#24616,#24617,
#24618,#24619,#24620,#24621,#24622,#24623,#24624,#24625,#24626,#24627,#24628,
#24629,#24630,#24631,#24632,#24633,#24634,#24635,#24636,#24637,#24638,#24639,
#24640,#24641,#24642),.UNSPECIFIED.,.F.,.F.,(4,3,3,3,3,3,3,3,3,3,3,3,3,
3,3,3,3,3,3,3,3,3,3,3,3,3,3,3,3,3,3,3,3,3,3,3,3,3,3,4),(0.,0.0627493370856802,
0.126104932649105,0.189559213327594,0.252240727815851,0.288293616367183,
0.305992302583669,0.313657647775325,0.376040508715825,0.396452282021179,
0.458859839175422,0.521377049363119,0.583471840572106,0.608441698788235,
0.617034861909103,0.624625665831328,0.686130535161024,0.747366753389966,
0.783230706301136,0.844791964570227,0.884204321033441,0.904295823092356,
0.915687649661771,0.925544683877737,0.98611829233901,1.04668162002177,1.1064743111715,
1.16009081627594,1.20586175519753,1.21479111379007,1.22268680009421,1.28246147324105,
1.34341068684296,1.36939753500024,1.3870819748845,1.39811570742417,1.45723390831247,
1.51569706474686,1.52625832764868,1.56606907499972),.UNSPECIFIED.);
#2555=B_SPLINE_CURVE_WITH_KNOTS('',3,(#24660,#24661,#24662,#24663,#24664,
#24665,#24666,#24667,#24668,#24669,#24670,#24671,#24672,#24673,#24674,#24675,
#24676,#24677,#24678,#24679,#24680,#24681,#24682,#24683,#24684,#24685,#24686,
#24687,#24688,#24689,#24690,#24691,#24692,#24693,#24694,#24695,#24696,#24697,
#24698,#24699,#24700,#24701,#24702,#24703,#24704,#24705,#24706,#24707,#24708,
#24709,#24710,#24711,#24712,#24713,#24714,#24715,#24716,#24717,#24718,#24719,
#24720,#24721,#24722,#24723,#24724,#24725,#24726,#24727,#24728,#24729,#24730,
#24731,#24732,#24733,#24734,#24735,#24736,#24737,#24738,#24739,#24740,#24741,
#24742,#24743,#24744,#24745,#24746,#24747,#24748,#24749,#24750),
 .UNSPECIFIED.,.F.,.F.,(4,3,3,3,3,3,3,3,3,3,3,3,3,3,3,3,3,3,3,3,3,3,3,3,
3,3,3,3,3,3,4),(0.,0.0297288188736182,0.0601143137532858,0.0893457032423633,
0.114923169045306,0.120627215633482,0.150386402906777,0.17998053365335,
0.208476757656489,0.220427983970411,0.228734462393759,0.234133594656578,
0.264049512161242,0.291954347405626,0.293965429665906,0.322911719928455,
0.339205408301995,0.343413416245237,0.371505798227718,0.399644786528458,
0.427380412744627,0.437702076823844,0.444667737156878,0.449308449996483,
0.477249012718954,0.498204434760807,0.506474258991161,0.511856137621095,
0.53779059950688,0.561070700886365,0.569248610399433),.UNSPECIFIED.);
#2556=B_SPLINE_CURVE_WITH_KNOTS('',3,(#24751,#24752,#24753,#24754,#24755,
#24756,#24757,#24758,#24759,#24760,#24761,#24762,#24763,#24764,#24765,#24766,
#24767,#24768,#24769,#24770,#24771,#24772,#24773,#24774,#24775,#24776,#24777,
#24778,#24779,#24780,#24781,#24782,#24783,#24784,#24785,#24786,#24787,#24788,
#24789,#24790,#24791,#24792,#24793,#24794,#24795,#24796,#24797,#24798,#24799,
#24800,#24801,#24802,#24803,#24804,#24805,#24806,#24807,#24808,#24809,#24810,
#24811,#24812,#24813,#24814,#24815,#24816,#24817,#24818,#24819,#24820,#24821,
#24822,#24823,#24824,#24825,#24826,#24827,#24828,#24829,#24830,#24831,#24832,
#24833,#24834,#24835,#24836,#24837,#24838,#24839,#24840,#24841,#24842,#24843,
#24844),.UNSPECIFIED.,.F.,.F.,(4,3,3,3,3,3,3,3,3,3,3,3,3,3,3,3,3,3,3,3,
3,3,3,3,3,3,3,3,3,3,3,4),(0.,0.0253686794174057,0.0514083856253428,0.0781556456631177,
0.0899216241726569,0.0966318743809286,0.10267802399304,0.12998244418627,
0.157736117425355,0.184648704550902,0.195933028986547,0.203013212233092,
0.207157428316433,0.236271947121987,0.265386465927542,0.293276540785509,
0.302549255500035,0.31126847526333,0.31569998302984,0.343808925905663,0.372948812494613,
0.402401913058982,0.413322292212205,0.422821815526522,0.427499464953869,
0.457558884663827,0.48241578665523,0.491036990018943,0.49835751386338,0.528866710916645,
0.556986492629438,0.566847306048074),.UNSPECIFIED.);
#2557=B_SPLINE_CURVE_WITH_KNOTS('',3,(#24845,#24846,#24847,#24848,#24849,
#24850,#24851,#24852,#24853,#24854,#24855,#24856,#24857,#24858,#24859,#24860,
#24861,#24862,#24863,#24864,#24865,#24866,#24867,#24868,#24869,#24870,#24871,
#24872,#24873,#24874,#24875,#24876,#24877,#24878,#24879,#24880,#24881,#24882,
#24883,#24884,#24885,#24886,#24887,#24888,#24889,#24890,#24891,#24892,#24893,
#24894,#24895,#24896,#24897,#24898,#24899,#24900,#24901,#24902,#24903,#24904,
#24905,#24906,#24907,#24908,#24909,#24910,#24911,#24912,#24913,#24914,#24915,
#24916,#24917,#24918,#24919,#24920,#24921,#24922,#24923,#24924,#24925,#24926,
#24927,#24928,#24929,#24930,#24931,#24932,#24933,#24934,#24935),
 .UNSPECIFIED.,.F.,.F.,(4,3,3,3,3,3,3,3,3,3,3,3,3,3,3,3,3,3,3,3,3,3,3,3,
3,3,3,3,3,3,4),(0.,0.0297288300137718,0.0601143303526995,0.0893457177668503,
0.114923181754232,0.120627216473642,0.150386403780864,0.179980531396028,
0.208476755963498,0.220427980048027,0.228734451696019,0.2341335924423,0.264049511054103,
0.291954343374694,0.293965429665906,0.322911720395065,0.339205406534996,
0.343413414673066,0.371505796934876,0.399644785176017,0.42738040871261,
0.437702067530731,0.444667652090904,0.449308353053096,0.477248940011413,
0.498204380230151,0.50647415245726,0.51185608788507,0.537790544146639,0.561070700886365,
0.569248610399433),.UNSPECIFIED.);
#2558=B_SPLINE_CURVE_WITH_KNOTS('',3,(#24936,#24937,#24938,#24939,#24940,
#24941,#24942,#24943,#24944,#24945,#24946,#24947,#24948,#24949,#24950,#24951,
#24952,#24953,#24954,#24955,#24956,#24957,#24958,#24959,#24960,#24961,#24962,
#24963,#24964,#24965,#24966,#24967,#24968,#24969,#24970,#24971,#24972,#24973,
#24974,#24975,#24976,#24977,#24978,#24979,#24980,#24981,#24982,#24983,#24984,
#24985,#24986,#24987,#24988,#24989,#24990,#24991,#24992,#24993,#24994,#24995,
#24996,#24997,#24998,#24999,#25000,#25001,#25002,#25003,#25004,#25005,#25006,
#25007,#25008,#25009,#25010,#25011,#25012,#25013,#25014,#25015,#25016,#25017,
#25018,#25019,#25020,#25021,#25022,#25023,#25024,#25025,#25026,#25027,#25028,
#25029),.UNSPECIFIED.,.F.,.F.,(4,3,3,3,3,3,3,3,3,3,3,3,3,3,3,3,3,3,3,3,
3,3,3,3,3,3,3,3,3,3,3,4),(0.,0.025368693811206,0.05140841299331,0.0781556696100889,
0.0899216297021826,0.0966318750772424,0.102678024005019,0.129982454186119,
0.157736132240341,0.184648715662141,0.19593303134926,0.203013213057673,
0.207157430078829,0.236271948003186,0.265386465927542,0.293276533635152,
0.302549240751372,0.311268412157304,0.315699971306864,0.343808903791577,
0.372948785654744,0.40240188507586,0.41332223980539,0.422821617175178,0.427499196231939,
0.457558610846334,0.48241558129211,0.491036574482664,0.498357488494488,
0.528866685800111,0.556986492629438,0.566847306048074),.UNSPECIFIED.);
#2559=B_SPLINE_CURVE_WITH_KNOTS('',3,(#25030,#25031,#25032,#25033,#25034,
#25035,#25036,#25037,#25038,#25039,#25040,#25041,#25042,#25043,#25044,#25045,
#25046,#25047,#25048,#25049,#25050,#25051,#25052,#25053,#25054,#25055,#25056,
#25057,#25058,#25059,#25060,#25061,#25062,#25063,#25064,#25065,#25066,#25067,
#25068,#25069,#25070,#25071,#25072,#25073,#25074,#25075,#25076,#25077,#25078,
#25079,#25080,#25081,#25082,#25083,#25084,#25085,#25086,#25087,#25088,#25089,
#25090,#25091,#25092,#25093,#25094,#25095,#25096,#25097,#25098,#25099,#25100,
#25101,#25102,#25103,#25104,#25105,#25106,#25107,#25108,#25109,#25110,#25111,
#25112,#25113,#25114,#25115,#25116,#25117,#25118,#25119,#25120),
 .UNSPECIFIED.,.F.,.F.,(4,3,3,3,3,3,3,3,3,3,3,3,3,3,3,3,3,3,3,3,3,3,3,3,
3,3,3,3,3,3,4),(0.,0.0297288424070436,0.0601143488180543,0.0893457339240374,
0.114923195891773,0.120627217421351,0.150386404765411,0.179980528895957,
0.208476754088448,0.220427975697114,0.228734439831626,0.234133589983501,
0.26404950982471,0.291954338892652,0.293965429665919,0.322911720916077,
0.339205404572844,0.343413412951878,0.371505795524539,0.399644783698224,
0.427380404250721,0.437702057239815,0.4446675578577,0.449308245657091,0.477248859464417,
0.498204319819911,0.506474034422274,0.511856032820092,0.537790482818068,
0.561070700886393,0.569248610399461),.UNSPECIFIED.);
#2560=B_SPLINE_CURVE_WITH_KNOTS('',3,(#25121,#25122,#25123,#25124,#25125,
#25126,#25127,#25128,#25129,#25130,#25131,#25132,#25133,#25134,#25135,#25136,
#25137,#25138,#25139,#25140,#25141,#25142,#25143,#25144,#25145,#25146,#25147,
#25148,#25149,#25150,#25151,#25152,#25153,#25154,#25155,#25156,#25157,#25158,
#25159,#25160,#25161,#25162,#25163,#25164,#25165,#25166,#25167,#25168,#25169,
#25170,#25171,#25172,#25173,#25174,#25175,#25176,#25177,#25178,#25179,#25180,
#25181,#25182,#25183,#25184,#25185,#25186,#25187,#25188,#25189,#25190,#25191,
#25192,#25193,#25194,#25195,#25196,#25197,#25198,#25199,#25200,#25201,#25202,
#25203,#25204,#25205,#25206,#25207,#25208,#25209,#25210,#25211,#25212,#25213,
#25214),.UNSPECIFIED.,.F.,.F.,(4,3,3,3,3,3,3,3,3,3,3,3,3,3,3,3,3,3,3,3,
3,3,3,3,3,3,3,3,3,3,3,4),(0.,0.0253686551369141,0.0514083394586729,0.0781556052672844,
0.0899216148451408,0.0966318732064026,0.102678023982166,0.1299824273254,
0.157736092440688,0.184648685812407,0.19593302500215,0.203013210837855,
0.20715742531342,0.236271945620492,0.265386465927564,0.293276552845118,
0.302549280374791,0.311268581698407,0.315700002803736,0.343808963203445,
0.372948857762899,0.402401960255444,0.413322380602343,0.42282215008815,
0.427499918423473,0.45755934672975,0.482416133204678,0.491037691280722,
0.498357556788384,0.528866753414147,0.556986492629462,0.566847306048097),
 .UNSPECIFIED.);
#2561=B_SPLINE_CURVE_WITH_KNOTS('',3,(#25215,#25216,#25217,#25218,#25219,
#25220,#25221,#25222,#25223,#25224,#25225,#25226,#25227,#25228,#25229,#25230,
#25231,#25232,#25233,#25234,#25235,#25236,#25237,#25238,#25239,#25240,#25241,
#25242,#25243,#25244,#25245,#25246,#25247,#25248,#25249,#25250,#25251,#25252,
#25253,#25254,#25255,#25256,#25257,#25258,#25259,#25260,#25261,#25262,#25263,
#25264,#25265,#25266,#25267,#25268,#25269,#25270,#25271,#25272,#25273,#25274,
#25275,#25276,#25277,#25278,#25279,#25280,#25281,#25282,#25283,#25284,#25285,
#25286,#25287,#25288,#25289,#25290,#25291,#25292,#25293,#25294,#25295,#25296,
#25297,#25298,#25299,#25300,#25301,#25302,#25303,#25304,#25305),
 .UNSPECIFIED.,.F.,.F.,(4,3,3,3,3,3,3,3,3,3,3,3,3,3,3,3,3,3,3,3,3,3,3,3,
3,3,3,3,3,3,4),(0.,0.0297288560421965,0.060114369134978,0.0893457517013431,
0.114923211446913,0.120627218448761,0.150386405832768,0.179980526129192,
0.208476752013369,0.220427970890768,0.228734426721466,0.234133587258058,
0.264049508461979,0.291954333951181,0.293965429665899,0.322911721485533,
0.339205402404708,0.343413411034994,0.371505793949006,0.399644782047769,
0.427380399316125,0.437702045866938,0.444667453732877,0.449308126997909,
0.47724877047002,0.498204253074103,0.506473904026581,0.511855971995141,
0.537790415102179,0.561070700886353,0.56924861039942),.UNSPECIFIED.);
#2562=B_SPLINE_CURVE_WITH_KNOTS('',3,(#25306,#25307,#25308,#25309,#25310,
#25311,#25312,#25313,#25314,#25315,#25316,#25317,#25318,#25319,#25320,#25321,
#25322,#25323,#25324,#25325,#25326,#25327,#25328,#25329,#25330,#25331,#25332,
#25333,#25334,#25335,#25336,#25337,#25338,#25339,#25340,#25341,#25342,#25343,
#25344,#25345,#25346,#25347,#25348,#25349,#25350,#25351,#25352,#25353,#25354,
#25355,#25356,#25357,#25358,#25359,#25360,#25361,#25362,#25363,#25364,#25365,
#25366,#25367,#25368,#25369,#25370,#25371,#25372,#25373,#25374,#25375,#25376,
#25377,#25378,#25379,#25380,#25381,#25382,#25383,#25384,#25385,#25386,#25387,
#25388,#25389,#25390,#25391,#25392,#25393,#25394,#25395,#25396,#25397,#25398,
#25399),.UNSPECIFIED.,.F.,.F.,(4,3,3,3,3,3,3,3,3,3,3,3,3,3,3,3,3,3,3,3,
3,3,3,3,3,3,3,3,3,3,3,4),(0.,0.0253686665250508,0.0514083611125175,0.0781556242143958,
0.0899216192202383,0.0966318737573469,0.102678023990962,0.129982435238011,
0.157736104164076,0.184648694604943,0.195933026871913,0.203013211491678,
0.207157426736985,0.236271946332265,0.265386465927544,0.29327654718868,
0.302549268707551,0.311268531776406,0.315699993528777,0.34380894570794,
0.372948836529036,0.402401938117202,0.413322339141515,0.422821993154248,
0.427499705665215,0.457559129940086,0.482415970612417,0.4910373622589,0.498357536637505,
0.528866733464123,0.556986492629412,0.566847306048045),.UNSPECIFIED.);
#2563=B_SPLINE_CURVE_WITH_KNOTS('',3,(#25401,#25402,#25403,#25404,#25405,
#25406,#25407,#25408,#25409,#25410,#25411,#25412,#25413,#25414,#25415,#25416,
#25417,#25418,#25419,#25420,#25421,#25422,#25423,#25424,#25425,#25426,#25427,
#25428,#25429,#25430,#25431,#25432,#25433,#25434,#25435,#25436,#25437,#25438,
#25439,#25440,#25441,#25442,#25443,#25444,#25445,#25446,#25447,#25448,#25449,
#25450,#25451,#25452,#25453,#25454,#25455,#25456,#25457,#25458,#25459,#25460,
#25461,#25462,#25463,#25464,#25465,#25466,#25467,#25468,#25469,#25470,#25471,
#25472,#25473,#25474,#25475,#25476,#25477,#25478,#25479,#25480,#25481,#25482,
#25483,#25484,#25485,#25486,#25487,#25488,#25489,#25490,#25491,#25492,#25493,
#25494),.UNSPECIFIED.,.F.,.F.,(4,3,3,3,3,3,3,3,3,3,3,3,3,3,3,3,3,3,3,3,
3,3,3,3,3,3,3,3,3,3,3,4),(-0.569248610399439,-0.543569219999376,-0.51726245007343,
-0.510383830357802,-0.504799176206508,-0.477734550505478,-0.455898128177116,
-0.447143555146704,-0.442467632926928,-0.414733780296404,-0.386572344665108,
-0.358632098172949,-0.344734866599356,-0.340184942209154,-0.311254405969609,
-0.30304317187858,-0.275230199031541,-0.246787090793276,-0.236990270246434,
-0.232158279697281,-0.227903807505874,-0.198913875468756,-0.169351066942439,
-0.13955255925445,-0.12334611597552,-0.118091324130729,-0.113402165305129,
-0.0828552636377898,-0.0522813313134371,-0.022324559840541,-0.0099010130230106,
0.),.UNSPECIFIED.);
#2564=B_SPLINE_CURVE_WITH_KNOTS('',3,(#25495,#25496,#25497,#25498,#25499,
#25500,#25501,#25502,#25503,#25504,#25505,#25506,#25507,#25508,#25509,#25510,
#25511,#25512,#25513,#25514,#25515,#25516,#25517,#25518,#25519,#25520,#25521,
#25522,#25523,#25524,#25525,#25526,#25527,#25528,#25529,#25530,#25531,#25532,
#25533,#25534,#25535,#25536,#25537,#25538,#25539,#25540,#25541,#25542,#25543,
#25544,#25545,#25546,#25547,#25548,#25549,#25550,#25551,#25552,#25553,#25554,
#25555,#25556,#25557,#25558,#25559,#25560,#25561,#25562,#25563,#25564,#25565,
#25566,#25567,#25568,#25569,#25570,#25571,#25572,#25573,#25574,#25575,#25576,
#25577,#25578,#25579,#25580,#25581,#25582,#25583,#25584,#25585,#25586,#25587,
#25588),.UNSPECIFIED.,.F.,.F.,(4,3,3,3,3,3,3,3,3,3,3,3,3,3,3,3,3,3,3,3,
3,3,3,3,3,3,3,3,3,3,3,4),(-0.566847306048102,-0.536662350861785,-0.506055522441016,
-0.497410970877117,-0.490478592762268,-0.460331914265818,-0.437093650808009,
-0.424723077676165,-0.420481376095385,-0.391056955765019,-0.361899168474601,
-0.333575784057379,-0.318788289693871,-0.313125278571146,-0.308695666218845,
-0.280706728188629,-0.274425806603346,-0.24594922105141,-0.216224375904036,
-0.204597160989918,-0.200878778856265,-0.173045052463213,-0.145277293489921,
-0.117981907776077,-0.104252976788119,-0.100010196974054,-0.095829444774943,
-0.0691576524997616,-0.0429343526171,-0.0175124074222168,-0.00815045987241754,
0.),.UNSPECIFIED.);
#2565=B_SPLINE_CURVE_WITH_KNOTS('',3,(#25590,#25591,#25592,#25593,#25594,
#25595,#25596,#25597,#25598,#25599,#25600),.UNSPECIFIED.,.F.,.F.,(4,1,1,
1,1,1,1,1,4),(15.7079632679489,15.8286682231623,16.8210880633759,17.8135079035895,
18.8059277438032,19.7983475840168,20.7907674242304,21.7831872644441,21.9911485751285),
 .UNSPECIFIED.);
#2566=B_SPLINE_CURVE_WITH_KNOTS('',3,(#25601,#25602,#25603,#25604,#25605,
#25606,#25607,#25608,#25609,#25610),.UNSPECIFIED.,.F.,.F.,(4,1,1,1,1,1,
1,4),(15.7079632679489,16.383239807399,17.3756596476127,18.3680794878263,
19.3604993280399,20.3529191682536,21.3453390084672,21.9911485751285),
 .UNSPECIFIED.);
#2567=B_SPLINE_CURVE_WITH_KNOTS('',3,(#26011,#26012,#26013,#26014,#26015,
#26016,#26017,#26018,#26019,#26020,#26021,#26022,#26023,#26024,#26025,#26026,
#26027,#26028,#26029,#26030,#26031,#26032,#26033,#26034,#26035),
 .UNSPECIFIED.,.F.,.F.,(4,3,3,3,3,3,3,3,4),(-10.1321597128207,-9.92419840213631,
-8.93177856192268,-7.93935872170905,-6.94693888149542,-5.95451904128179,
-4.96209920106816,-3.96967936085453,-3.84897440564114),.UNSPECIFIED.);
#2568=B_SPLINE_CURVE_WITH_KNOTS('',3,(#26436,#26437,#26438,#26439,#26440,
#26441,#26442,#26443,#26444,#26445,#26446,#26447,#26448,#26449,#26450,#26451,
#26452,#26453,#26454,#26455,#26456,#26457),.UNSPECIFIED.,.F.,.F.,(4,3,3,
3,3,3,3,4),(7.59274844815661,7.93935872170905,8.93177856192268,9.92419840213631,
10.9166182423499,11.9090380825636,12.9014579227772,13.8759337553362),
 .UNSPECIFIED.);
#2569=B_SPLINE_CURVE_WITH_KNOTS('',3,(#26460,#26461,#26462,#26463,#26464,
#26465,#26466,#26467,#26468,#26469,#26470,#26471,#26472,#26473,#26474,#26475,
#26476,#26477,#26478,#26479,#26480,#26481,#26482,#26483,#26484,#26485,#26486,
#26487,#26488,#26489,#26490,#26491,#26492,#26493,#26494,#26495,#26496,#26497,
#26498,#26499,#26500,#26501,#26502,#26503,#26504,#26505,#26506,#26507,#26508,
#26509,#26510,#26511,#26512,#26513,#26514,#26515,#26516,#26517,#26518,#26519,
#26520,#26521,#26522,#26523,#26524,#26525,#26526,#26527,#26528,#26529,#26530,
#26531,#26532,#26533,#26534,#26535,#26536,#26537,#26538,#26539,#26540,#26541,
#26542,#26543,#26544,#26545,#26546,#26547,#26548,#26549,#26550,#26551,#26552,
#26553),.UNSPECIFIED.,.F.,.F.,(4,3,3,3,3,3,3,3,3,3,3,3,3,3,3,3,3,3,3,3,
3,3,3,3,3,3,3,3,3,3,3,4),(-0.569248610399384,-0.543569235590288,-0.517262478651252,
-0.510383901889905,-0.5047991812893,-0.477734566431476,-0.45589814211236,
-0.447143686501957,-0.442467743120936,-0.414733902739171,-0.386572466363187,
-0.358632212682089,-0.344734952481205,-0.340185022063421,-0.311254485448412,
-0.303043171878551,-0.275230188458927,-0.24678707363057,-0.236990217909345,
-0.232158195033693,-0.227903714787798,-0.198913772270501,-0.169350958285975,
-0.139552450005073,-0.123346020382315,-0.118091100987548,-0.11340214359472,
-0.0828552403272742,-0.052281308311463,-0.0223245354250729,-0.00990101302301064,
0.),.UNSPECIFIED.);
#2570=B_SPLINE_CURVE_WITH_KNOTS('',3,(#26554,#26555,#26556,#26557,#26558,
#26559,#26560,#26561,#26562,#26563,#26564,#26565,#26566,#26567,#26568,#26569,
#26570,#26571,#26572,#26573,#26574,#26575,#26576,#26577,#26578,#26579,#26580,
#26581,#26582,#26583,#26584,#26585,#26586,#26587,#26588,#26589,#26590,#26591,
#26592,#26593,#26594,#26595,#26596,#26597,#26598,#26599,#26600,#26601,#26602,
#26603,#26604,#26605,#26606,#26607,#26608,#26609,#26610,#26611,#26612,#26613,
#26614,#26615,#26616,#26617,#26618,#26619,#26620,#26621,#26622,#26623,#26624,
#26625,#26626,#26627,#26628,#26629,#26630,#26631,#26632,#26633,#26634,#26635,
#26636,#26637,#26638,#26639,#26640,#26641,#26642,#26643,#26644,#26645,#26646,
#26647),.UNSPECIFIED.,.F.,.F.,(4,3,3,3,3,3,3,3,3,3,3,3,3,3,3,3,3,3,3,3,
3,3,3,3,3,3,3,3,3,3,3,4),(-0.566847306048057,-0.536662357910539,-0.506055531265482,
-0.49741098170805,-0.490478594836811,-0.460331915979511,-0.437093652307487,
-0.424723081249797,-0.420481379994704,-0.391056958700494,-0.361899170676201,
-0.333575783700219,-0.318788289425995,-0.31312527916877,-0.308695666742216,
-0.28070672569703,-0.274425806603323,-0.245949220781907,-0.21622437566822,
-0.204597161217252,-0.200878778552373,-0.173045052561144,-0.145277293074677,
-0.117981904358029,-0.104252973797327,-0.100010187224494,-0.0958294424246432,
-0.0691576481481108,-0.0429343440651014,-0.0175123918711586,-0.00815045987241372,
0.),.UNSPECIFIED.);
#2571=B_SPLINE_CURVE_WITH_KNOTS('',3,(#26649,#26650,#26651,#26652,#26653,
#26654,#26655,#26656,#26657,#26658,#26659),.UNSPECIFIED.,.F.,.F.,(4,1,1,
1,1,1,1,1,4),(15.7079632679489,15.8286682231623,16.8210880633759,17.8135079035895,
18.8059277438032,19.7983475840168,20.7907674242304,21.7831872644441,21.9911485751285),
 .UNSPECIFIED.);
#2572=B_SPLINE_CURVE_WITH_KNOTS('',3,(#26660,#26661,#26662,#26663,#26664,
#26665,#26666,#26667,#26668,#26669),.UNSPECIFIED.,.F.,.F.,(4,1,1,1,1,1,
1,4),(15.7079632679489,16.383239807399,17.3756596476127,18.3680794878263,
19.3604993280399,20.3529191682536,21.3453390084672,21.9911485751285),
 .UNSPECIFIED.);
#2573=B_SPLINE_CURVE_WITH_KNOTS('',3,(#27070,#27071,#27072,#27073,#27074,
#27075,#27076,#27077,#27078,#27079,#27080,#27081,#27082,#27083,#27084,#27085,
#27086,#27087,#27088,#27089,#27090,#27091,#27092,#27093,#27094),
 .UNSPECIFIED.,.F.,.F.,(4,3,3,3,3,3,3,3,4),(-10.1321597128207,-9.92419840213631,
-8.93177856192268,-7.93935872170905,-6.94693888149542,-5.95451904128179,
-4.96209920106816,-3.96967936085453,-3.84897440564114),.UNSPECIFIED.);
#2574=B_SPLINE_CURVE_WITH_KNOTS('',3,(#27495,#27496,#27497,#27498,#27499,
#27500,#27501,#27502,#27503,#27504,#27505,#27506,#27507,#27508,#27509,#27510,
#27511,#27512,#27513,#27514,#27515,#27516),.UNSPECIFIED.,.F.,.F.,(4,3,3,
3,3,3,3,4),(7.59274844815661,7.93935872170905,8.93177856192269,9.92419840213631,
10.9166182423499,11.9090380825636,12.9014579227772,13.8759337553362),
 .UNSPECIFIED.);
#2575=B_SPLINE_CURVE_WITH_KNOTS('',3,(#27521,#27522,#27523,#27524,#27525,
#27526,#27527,#27528,#27529,#27530,#27531,#27532,#27533,#27534,#27535,#27536,
#27537,#27538,#27539,#27540,#27541,#27542,#27543,#27544,#27545,#27546,#27547,
#27548,#27549,#27550,#27551),.UNSPECIFIED.,.F.,.F.,(4,3,3,3,3,3,3,3,3,3,
4),(-0.186478347341216,-0.158619634599147,-0.131056531933734,-0.104105248740391,
-0.100056848097327,-0.0957909510082901,-0.0691196899172101,-0.0428971352288845,
-0.0174757607808009,-0.00815045987241733,0.),.UNSPECIFIED.);
#2576=B_SPLINE_CURVE_WITH_KNOTS('',3,(#27555,#27556,#27557,#27558,#27559,
#27560,#27561,#27562,#27563,#27564,#27565,#27566,#27567,#27568,#27569,#27570,
#27571,#27572,#27573,#27574,#27575,#27576,#27577,#27578,#27579,#27580,#27581,
#27582,#27583,#27584,#27585,#27586,#27587,#27588,#27589,#27590,#27591,#27592,
#27593,#27594,#27595,#27596,#27597,#27598,#27599,#27600,#27601,#27602,#27603,
#27604,#27605,#27606,#27607,#27608,#27609,#27610,#27611,#27612,#27613,#27614,
#27615,#27616,#27617,#27618),.UNSPECIFIED.,.F.,.F.,(4,3,3,3,3,3,3,3,3,3,
3,3,3,3,3,3,3,3,3,3,3,4),(-0.382265902471371,-0.354388912953647,-0.344229210342304,
-0.337959875745192,-0.309029041715164,-0.303043171878561,-0.275230178847725,
-0.246787058020227,-0.236990170309578,-0.232158118032837,-0.227903630488106,
-0.198913678448654,-0.169350859502243,-0.139552350678771,-0.123345933471801,
-0.118090898210581,-0.113402123852804,-0.0828552191246252,-0.0522812873900625,
-0.0223245132224302,-0.00990101302301068,0.),.UNSPECIFIED.);
#2577=B_SPLINE_CURVE_WITH_KNOTS('',3,(#27619,#27620,#27621,#27622,#27623,
#27624,#27625,#27626,#27627,#27628,#27629,#27630,#27631,#27632,#27633,#27634,
#27635,#27636,#27637,#27638,#27639,#27640,#27641,#27642,#27643,#27644,#27645,
#27646,#27647,#27648,#27649,#27650,#27651,#27652,#27653,#27654,#27655,#27656,
#27657,#27658,#27659,#27660,#27661,#27662,#27663,#27664,#27665,#27666,#27667,
#27668,#27669,#27670,#27671,#27672,#27673,#27674,#27675,#27676,#27677,#27678,
#27679,#27680,#27681,#27682),.UNSPECIFIED.,.F.,.F.,(4,3,3,3,3,3,3,3,3,3,
3,3,3,3,3,3,3,3,3,3,3,4),(-0.566847306048054,-0.536662333984777,-0.506055501317574,
-0.49741094495226,-0.490478587792416,-0.46033191015455,-0.437093647210649,
-0.424723069108858,-0.42048136705109,-0.391056949034952,-0.361899163427049,
-0.333575785136632,-0.318788290503309,-0.313125277598956,-0.308695665438203,
-0.280706734635303,-0.274425806603339,-0.24586775158787,-0.216173049464543,
-0.206760965590708,-0.202702619221145,-0.186478347341216),.UNSPECIFIED.);
#2578=B_SPLINE_CURVE_WITH_KNOTS('',3,(#27687,#27688,#27689,#27690,#27691,
#27692,#27693,#27694,#27695,#27696,#27697,#27698,#27699,#27700,#27701,#27702,
#27703,#27704,#27705,#27706,#27707,#27708,#27709,#27710,#27711,#27712,#27713,
#27714,#27715,#27716,#27717,#27718,#27719,#27720),.UNSPECIFIED.,.F.,.F.,
(4,3,3,3,3,3,3,3,3,3,3,4),(-0.569248610399408,-0.543383188674187,-0.523243527898835,
-0.5111120528569,-0.504565698233315,-0.477731171126537,-0.453864853962746,
-0.447746320338163,-0.443048137353461,-0.415379481235353,-0.38724361464334,
-0.382265902471371),.UNSPECIFIED.);
#2579=B_SPLINE_CURVE_WITH_KNOTS('',3,(#27722,#27723,#27724,#27725,#27726,
#27727,#27728,#27729,#27730,#27731,#27732),.UNSPECIFIED.,.F.,.F.,(4,1,1,
1,1,1,1,1,4),(15.7079632679489,15.8286682231623,16.8210880633759,17.8135079035895,
18.8059277438032,19.7983475840168,20.7907674242304,21.7831872644441,21.9911485751285),
 .UNSPECIFIED.);
#2580=B_SPLINE_CURVE_WITH_KNOTS('',3,(#27733,#27734,#27735,#27736,#27737,
#27738,#27739,#27740,#27741,#27742),.UNSPECIFIED.,.F.,.F.,(4,1,1,1,1,1,
1,4),(15.7079632679489,16.383239807399,17.3756596476127,18.3680794878263,
19.3604993280399,20.3529191682536,21.3453390084672,21.9911485751285),
 .UNSPECIFIED.);
#2581=B_SPLINE_CURVE_WITH_KNOTS('',3,(#28143,#28144,#28145,#28146,#28147,
#28148,#28149,#28150,#28151,#28152,#28153,#28154,#28155,#28156,#28157,#28158,
#28159,#28160,#28161,#28162,#28163,#28164,#28165,#28166,#28167),
 .UNSPECIFIED.,.F.,.F.,(4,3,3,3,3,3,3,3,4),(-10.1321597128207,-9.92419840213631,
-8.93177856192268,-7.93935872170905,-6.94693888149542,-5.95451904128179,
-4.96209920106816,-3.96967936085453,-3.84897440564114),.UNSPECIFIED.);
#2582=B_SPLINE_CURVE_WITH_KNOTS('',3,(#28568,#28569,#28570,#28571,#28572,
#28573,#28574,#28575,#28576,#28577,#28578,#28579,#28580,#28581,#28582,#28583,
#28584,#28585,#28586,#28587,#28588,#28589),.UNSPECIFIED.,.F.,.F.,(4,3,3,
3,3,3,3,4),(7.59274844815661,7.93935872170905,8.93177856192269,9.92419840213631,
10.9166182423499,11.9090380825636,12.9014579227772,13.8759337553362),
 .UNSPECIFIED.);
#2583=B_SPLINE_CURVE_WITH_KNOTS('',3,(#28592,#28593,#28594,#28595,#28596,
#28597,#28598,#28599,#28600,#28601),.UNSPECIFIED.,.F.,.F.,(4,2,2,2,4),(1.93603633322311,
2.0327017356838,2.12936713814449,2.22630536900611,2.32324359986774),
 .UNSPECIFIED.);
#2584=B_SPLINE_CURVE_WITH_KNOTS('',3,(#28602,#28603,#28604,#28605,#28606,
#28607,#28608,#28609,#28610,#28611),.UNSPECIFIED.,.F.,.F.,(4,2,2,2,4),(0.774414533289245,
0.871352764150867,0.968290995012489,1.06495639747318,1.16162179993387),
 .UNSPECIFIED.);
#2585=B_SPLINE_CURVE_WITH_KNOTS('',3,(#28615,#28616,#28617,#28618,#28619,
#28620,#28621,#28622,#28623,#28624,#28625,#28626,#28627,#28628,#28629,#28630,
#28631,#28632,#28633,#28634,#28635,#28636,#28637,#28638,#28639,#28640,#28641,
#28642,#28643,#28644,#28645),.UNSPECIFIED.,.F.,.F.,(4,3,3,3,3,3,3,3,3,3,
4),(-0.186478347341219,-0.158619634855163,-0.131056530031512,-0.104105241249995,
-0.100056821695491,-0.0957909465603036,-0.0691196829588407,-0.0428971229819699,
-0.0174757397045835,-0.00815045987241733,0.),.UNSPECIFIED.);
#2586=B_SPLINE_CURVE_WITH_KNOTS('',3,(#28649,#28650,#28651,#28652,#28653,
#28654,#28655,#28656,#28657,#28658,#28659,#28660,#28661,#28662,#28663,#28664,
#28665,#28666,#28667,#28668,#28669,#28670,#28671,#28672,#28673,#28674,#28675,
#28676,#28677,#28678,#28679,#28680,#28681,#28682,#28683,#28684,#28685,#28686,
#28687,#28688,#28689,#28690,#28691,#28692,#28693,#28694,#28695,#28696,#28697,
#28698,#28699,#28700,#28701,#28702,#28703,#28704,#28705,#28706,#28707,#28708,
#28709,#28710,#28711,#28712),.UNSPECIFIED.,.F.,.F.,(4,3,3,3,3,3,3,3,3,3,
3,3,3,3,3,3,3,3,3,3,3,4),(-0.382265902471371,-0.354388907971518,-0.344229193097268,
-0.337959880834284,-0.309029046216205,-0.303043171878561,-0.275230170211377,
-0.246787044002095,-0.236990127562464,-0.232158048919115,-0.227903554968478,
-0.198913594373769,-0.169350770972404,-0.139552261670151,-0.123345855589258,
-0.11809071636682,-0.11340210613496,-0.0828552000931288,-0.0522812686134481,
-0.0223244932935985,-0.00990101302301068,0.),.UNSPECIFIED.);
#2587=B_SPLINE_CURVE_WITH_KNOTS('',3,(#28713,#28714,#28715,#28716,#28717,
#28718,#28719,#28720,#28721,#28722,#28723,#28724,#28725,#28726,#28727,#28728,
#28729,#28730,#28731,#28732,#28733,#28734,#28735,#28736,#28737,#28738,#28739,
#28740,#28741,#28742,#28743,#28744,#28745,#28746,#28747,#28748,#28749,#28750,
#28751,#28752,#28753,#28754,#28755,#28756,#28757,#28758,#28759,#28760,#28761,
#28762,#28763,#28764,#28765,#28766,#28767,#28768,#28769,#28770,#28771,#28772,
#28773,#28774,#28775,#28776),.UNSPECIFIED.,.F.,.F.,(4,3,3,3,3,3,3,3,3,3,
3,3,3,3,3,3,3,3,3,3,3,4),(-0.566847306048054,-0.53666234288915,-0.506055512459245,
-0.497410958629855,-0.490478590394541,-0.460331912302746,-0.43709364909032,
-0.424723073596147,-0.420481371815357,-0.391056952578469,-0.361899166084687,
-0.333575784563524,-0.318788290073478,-0.313125278104711,-0.308695665838356,
-0.280706731221203,-0.274425806603339,-0.24586775166354,-0.21617304950238,
-0.206760964784706,-0.20270261672099,-0.186478347341219),.UNSPECIFIED.);
#2588=B_SPLINE_CURVE_WITH_KNOTS('',3,(#28781,#28782,#28783,#28784,#28785,
#28786,#28787,#28788,#28789,#28790,#28791,#28792,#28793,#28794,#28795,#28796,
#28797,#28798,#28799,#28800,#28801,#28802,#28803,#28804,#28805,#28806,#28807,
#28808,#28809,#28810,#28811,#28812,#28813,#28814),.UNSPECIFIED.,.F.,.F.,
(4,3,3,3,3,3,3,3,3,3,3,4),(-0.569248610399408,-0.543383200898257,-0.523243538594896,
-0.511112056843439,-0.504565699175182,-0.477731182424187,-0.453864862435983,
-0.447746321418146,-0.443048138290636,-0.415379490937535,-0.387243626784474,
-0.382265902471371),.UNSPECIFIED.);
#2589=B_SPLINE_CURVE_WITH_KNOTS('',3,(#28816,#28817,#28818,#28819,#28820,
#28821,#28822,#28823,#28824,#28825,#28826),.UNSPECIFIED.,.F.,.F.,(4,1,1,
1,1,1,1,1,4),(15.7079632679489,15.8286682231623,16.8210880633759,17.8135079035895,
18.8059277438032,19.7983475840168,20.7907674242304,21.7831872644441,21.9911485751285),
 .UNSPECIFIED.);
#2590=B_SPLINE_CURVE_WITH_KNOTS('',3,(#28827,#28828,#28829,#28830,#28831,
#28832,#28833,#28834,#28835,#28836),.UNSPECIFIED.,.F.,.F.,(4,1,1,1,1,1,
1,4),(15.7079632679489,16.383239807399,17.3756596476127,18.3680794878263,
19.3604993280399,20.3529191682536,21.3453390084672,21.9911485751285),
 .UNSPECIFIED.);
#2591=B_SPLINE_CURVE_WITH_KNOTS('',3,(#29237,#29238,#29239,#29240,#29241,
#29242,#29243,#29244,#29245,#29246,#29247,#29248,#29249,#29250,#29251,#29252,
#29253,#29254,#29255,#29256,#29257,#29258,#29259,#29260,#29261),
 .UNSPECIFIED.,.F.,.F.,(4,3,3,3,3,3,3,3,4),(-10.1321597128207,-9.92419840213631,
-8.93177856192268,-7.93935872170905,-6.94693888149542,-5.95451904128179,
-4.96209920106816,-3.96967936085453,-3.84897440564114),.UNSPECIFIED.);
#2592=B_SPLINE_CURVE_WITH_KNOTS('',3,(#29662,#29663,#29664,#29665,#29666,
#29667,#29668,#29669,#29670,#29671,#29672,#29673,#29674,#29675,#29676,#29677,
#29678,#29679,#29680,#29681,#29682,#29683),.UNSPECIFIED.,.F.,.F.,(4,3,3,
3,3,3,3,4),(7.59274844815661,7.93935872170905,8.93177856192269,9.92419840213631,
10.9166182423499,11.9090380825636,12.9014579227772,13.8759337553362),
 .UNSPECIFIED.);
#2593=B_SPLINE_CURVE_WITH_KNOTS('',3,(#29686,#29687,#29688,#29689,#29690,
#29691,#29692,#29693,#29694,#29695),.UNSPECIFIED.,.F.,.F.,(4,2,2,2,4),(1.93603633322311,
2.0327017356838,2.12936713814449,2.22630536900611,2.32324359986774),
 .UNSPECIFIED.);
#2594=B_SPLINE_CURVE_WITH_KNOTS('',3,(#29696,#29697,#29698,#29699,#29700,
#29701,#29702,#29703,#29704,#29705),.UNSPECIFIED.,.F.,.F.,(4,2,2,2,4),(0.774414533289245,
0.871352764150867,0.968290995012489,1.06495639747318,1.16162179993387),
 .UNSPECIFIED.);
#2595=B_SPLINE_CURVE_WITH_KNOTS('',3,(#29711,#29712,#29713,#29714,#29715,
#29716,#29717,#29718,#29719,#29720,#29721,#29722,#29723,#29724,#29725,#29726,
#29727,#29728,#29729,#29730,#29731,#29732,#29733,#29734,#29735,#29736,#29737,
#29738,#29739,#29740,#29741,#29742,#29743,#29744,#29745,#29746,#29747,#29748,
#29749,#29750,#29751,#29752,#29753,#29754,#29755,#29756,#29757,#29758,#29759,
#29760,#29761,#29762,#29763,#29764,#29765,#29766,#29767,#29768,#29769,#29770,
#29771,#29772,#29773,#29774,#29775,#29776,#29777,#29778,#29779,#29780,#29781,
#29782,#29783,#29784,#29785,#29786,#29787,#29788,#29789,#29790,#29791,#29792,
#29793,#29794,#29795,#29796,#29797,#29798),.UNSPECIFIED.,.F.,.F.,(4,3,3,
3,3,3,3,3,3,3,3,3,3,3,3,3,3,3,3,3,3,3,3,3,3,3,3,3,3,4),(-0.378621596831415,
-0.359797488651071,-0.347859564017193,-0.339721384340795,-0.335383707835788,
-0.315512004032695,-0.301177697597527,-0.297260794867737,-0.293227238012395,
-0.27282498756368,-0.252127330348507,-0.239304885899219,-0.228805595020818,
-0.224505148589752,-0.203200592223416,-0.200837552551353,-0.18035024909426,
-0.158310752857967,-0.154330298823938,-0.150809435172749,-0.129426160732041,
-0.10759198857076,-0.085625366894301,-0.0802031148086871,-0.0759441736813679,
-0.0533965995856124,-0.030824430585221,-0.00876579303116958,-0.0040342792039134,
0.),.UNSPECIFIED.);
#2596=B_SPLINE_CURVE_WITH_KNOTS('',3,(#29799,#29800,#29801,#29802,#29803,
#29804,#29805,#29806,#29807,#29808,#29809,#29810,#29811,#29812,#29813,#29814,
#29815,#29816,#29817,#29818,#29819,#29820,#29821,#29822,#29823,#29824,#29825,
#29826,#29827,#29828,#29829,#29830,#29831,#29832,#29833,#29834,#29835,#29836,
#29837,#29838,#29839,#29840,#29841,#29842,#29843,#29844,#29845,#29846,#29847,
#29848,#29849,#29850,#29851,#29852,#29853,#29854,#29855,#29856,#29857,#29858,
#29859,#29860,#29861,#29862,#29863,#29864,#29865,#29866,#29867,#29868,#29869,
#29870,#29871,#29872,#29873,#29874,#29875,#29876,#29877,#29878,#29879,#29880,
#29881,#29882,#29883),.UNSPECIFIED.,.F.,.F.,(4,3,3,3,3,3,3,3,3,3,3,3,3,
3,3,3,3,3,3,3,3,3,3,3,3,3,3,3,4),(-0.376940817211644,-0.354634297224817,
-0.332912868281746,-0.328064575910149,-0.305815976299773,-0.290196837472332,
-0.284261042344383,-0.278600436982198,-0.256917266795448,-0.235699705654349,
-0.214947482958391,-0.208197203240807,-0.204402057618207,-0.183825925259162,
-0.180862865680244,-0.159880209119453,-0.140305785753204,-0.136021308905087,
-0.132587897579495,-0.112128579246988,-0.0917639886504933,-0.0718357414527914,
-0.0676216417654861,-0.0636601334983857,-0.0441022477646612,-0.0249163166467412,
-0.00635335474236993,-0.00328482218946179,0.),.UNSPECIFIED.);
#2597=B_SPLINE_CURVE_WITH_KNOTS('',3,(#29885,#29886,#29887,#29888,#29889,
#29890,#29891,#29892,#29893,#29894,#29895),.UNSPECIFIED.,.F.,.F.,(4,1,1,
1,1,1,1,1,4),(15.7079632679489,15.851694142003,16.8492226764396,17.8467512108762,
18.8442797453128,19.8418082797494,20.839336814186,21.8368653486226,21.9911485751285),
 .UNSPECIFIED.);
#2598=B_SPLINE_CURVE_WITH_KNOTS('',3,(#29896,#29897,#29898,#29899,#29900,
#29901,#29902,#29903,#29904,#29905),.UNSPECIFIED.,.F.,.F.,(4,1,1,1,1,1,
1,4),(15.7079632679489,16.39319808165,17.3907266160866,18.3882551505232,
19.3857836849598,20.3833122193964,21.380840753833,21.9911485751284),
 .UNSPECIFIED.);
#2599=B_SPLINE_CURVE_WITH_KNOTS('',3,(#30322,#30323,#30324,#30325,#30326,
#30327,#30328,#30329,#30330,#30331,#30332,#30333,#30334,#30335,#30336,#30337,
#30338,#30339,#30340,#30341,#30342,#30343,#30344,#30345,#30346,#30347,#30348,
#30349,#30350,#30351,#30352,#30353,#30354,#30355,#30356,#30357,#30358,#30359,
#30360,#30361,#30362,#30363,#30364,#30365,#30366,#30367,#30368,#30369,#30370,
#30371,#30372,#30373,#30374,#30375,#30376,#30377,#30378,#30379,#30380,#30381,
#30382,#30383,#30384,#30385,#30386,#30387,#30388,#30389,#30390,#30391,#30392,
#30393,#30394,#30395,#30396,#30397,#30398,#30399,#30400,#30401,#30402,#30403),
 .UNSPECIFIED.,.F.,.F.,(4,3,3,3,3,3,3,3,3,3,3,3,3,3,3,3,3,3,3,3,3,3,3,3,
3,3,3,4),(0.,0.0185974702011865,0.0384224406125438,0.0557692897224814,0.0644714144177272,
0.0684505998290036,0.0885047671947535,0.108914689664935,0.125985325621712,
0.133848200607443,0.137284581833955,0.158359464766614,0.177197233492045,
0.197725006274794,0.20564964402825,0.20912533594064,0.230131014427894,0.251623268601124,
0.268075190636431,0.278317576716938,0.284044648983082,0.306313636977894,
0.322966020148207,0.328172647466716,0.333184029352957,0.355705443842072,
0.372923169659143,0.376940817211587),.UNSPECIFIED.);
#2600=B_SPLINE_CURVE_WITH_KNOTS('',3,(#30404,#30405,#30406,#30407,#30408,
#30409,#30410,#30411,#30412,#30413,#30414,#30415,#30416,#30417,#30418,#30419,
#30420,#30421,#30422,#30423,#30424,#30425,#30426,#30427,#30428),
 .UNSPECIFIED.,.F.,.F.,(4,3,3,3,3,3,3,3,4),(-10.1295685708719,-9.975285344366,
-8.9777568099294,-7.9802282754928,-6.9826997410562,-5.9851712066196,-4.987642672183,
-3.9901141377464,-3.84638326369234),.UNSPECIFIED.);
#2601=B_SPLINE_CURVE_WITH_KNOTS('',3,(#30845,#30846,#30847,#30848,#30849,
#30850,#30851,#30852,#30853,#30854,#30855,#30856,#30857,#30858,#30859,#30860,
#30861,#30862,#30863,#30864,#30865,#30866),.UNSPECIFIED.,.F.,.F.,(4,3,3,
3,3,3,3,4),(7.59300756235157,7.9802282754928,8.9777568099294,9.975285344366,
10.9728138788026,11.9703424132392,12.9678709476758,13.8761928695312),
 .UNSPECIFIED.);
#2602=B_SPLINE_CURVE_WITH_KNOTS('',3,(#30867,#30868,#30869,#30870,#30871,
#30872,#30873,#30874,#30875,#30876,#30877,#30878,#30879,#30880,#30881,#30882,
#30883,#30884,#30885,#30886,#30887,#30888,#30889,#30890,#30891,#30892,#30893,
#30894,#30895,#30896,#30897,#30898,#30899,#30900,#30901,#30902,#30903,#30904,
#30905,#30906,#30907,#30908,#30909,#30910,#30911,#30912,#30913,#30914,#30915,
#30916,#30917,#30918,#30919,#30920,#30921,#30922,#30923,#30924,#30925,#30926,
#30927,#30928,#30929,#30930,#30931,#30932,#30933,#30934,#30935,#30936,#30937,
#30938,#30939,#30940,#30941,#30942,#30943,#30944,#30945,#30946,#30947,#30948,
#30949,#30950,#30951),.UNSPECIFIED.,.F.,.F.,(4,3,3,3,3,3,3,3,3,3,3,3,3,
3,3,3,3,3,3,3,3,3,3,3,3,3,3,3,4),(0.,0.0219661302700472,0.0445436036366041,
0.06362009313796,0.0720969467217393,0.0767544176956762,0.0810485403387707,
0.102995140835155,0.124771437273058,0.142867457866657,0.150422750087673,
0.153917807515336,0.157566643421491,0.178337400691585,0.197155519647451,
0.219426672701591,0.224328239844768,0.22940123318273,0.25006631851888,0.27072713343305,
0.285676237002597,0.296892227344257,0.30062314254954,0.320395494413919,
0.334302188530373,0.338768597396786,0.357793672729449,0.375324744080571,
0.378621596831418),.UNSPECIFIED.);
#2603=B_SPLINE_CURVE_WITH_KNOTS('',3,(#30954,#30955,#30956,#30957,#30958,
#30959,#30960,#30961,#30962,#30963,#30964,#30965,#30966,#30967,#30968,#30969,
#30970,#30971,#30972,#30973,#30974,#30975,#30976,#30977,#30978,#30979,#30980,
#30981,#30982,#30983,#30984,#30985,#30986,#30987,#30988,#30989,#30990,#30991,
#30992,#30993,#30994,#30995,#30996,#30997,#30998,#30999,#31000,#31001,#31002,
#31003,#31004,#31005,#31006,#31007,#31008,#31009,#31010,#31011,#31012,#31013,
#31014,#31015,#31016,#31017,#31018,#31019,#31020,#31021,#31022,#31023,#31024,
#31025,#31026,#31027,#31028,#31029,#31030,#31031,#31032,#31033,#31034,#31035,
#31036,#31037,#31038,#31039,#31040,#31041),.UNSPECIFIED.,.F.,.F.,(4,3,3,
3,3,3,3,3,3,3,3,3,3,3,3,3,3,3,3,3,3,3,3,3,3,3,3,3,3,4),(-0.378621596831449,
-0.359797495255613,-0.347859580799326,-0.339721534947358,-0.335383781754089,
-0.31551208410872,-0.301177767664049,-0.297260953938726,-0.293227258605859,
-0.272825012825785,-0.252127354965836,-0.239304904362215,-0.228805622237141,
-0.224505157276384,-0.203200600638345,-0.200837552551351,-0.180350244595754,
-0.158310748921773,-0.154330272617166,-0.150809430446371,-0.129426152351927,
-0.107591978572832,-0.0856253568644043,-0.0802030973073672,-0.0759441676007146,
-0.0533965927429803,-0.0308244238812939,-0.00876578556903723,-0.00403427920390745,
0.),.UNSPECIFIED.);
#2604=B_SPLINE_CURVE_WITH_KNOTS('',3,(#31042,#31043,#31044,#31045,#31046,
#31047,#31048,#31049,#31050,#31051,#31052,#31053,#31054,#31055,#31056,#31057,
#31058,#31059,#31060,#31061,#31062,#31063,#31064,#31065,#31066,#31067,#31068,
#31069,#31070,#31071,#31072,#31073,#31074,#31075,#31076,#31077,#31078,#31079,
#31080,#31081,#31082,#31083,#31084,#31085,#31086,#31087,#31088,#31089,#31090,
#31091,#31092,#31093,#31094,#31095,#31096,#31097,#31098,#31099,#31100,#31101,
#31102,#31103,#31104,#31105,#31106,#31107,#31108,#31109,#31110,#31111,#31112,
#31113,#31114,#31115,#31116,#31117,#31118,#31119,#31120,#31121,#31122,#31123,
#31124,#31125,#31126),.UNSPECIFIED.,.F.,.F.,(4,3,3,3,3,3,3,3,3,3,3,3,3,
3,3,3,3,3,3,3,3,3,3,3,3,3,3,3,4),(-0.376940817211602,-0.354634286106805,
-0.332912858553484,-0.328064564631197,-0.305815965171254,-0.290196827734877,
-0.284261020742464,-0.278600438394339,-0.25691727004817,-0.235699713647721,
-0.214947494052335,-0.208197196081605,-0.204402058518297,-0.183825930761354,
-0.180862865680241,-0.159880209155866,-0.140305785785065,-0.136021316510379,
-0.132587903785407,-0.112128584732708,-0.0917639954653299,-0.0718357542938654,
-0.067621677650879,-0.0636601454777048,-0.0441022630341506,-0.0249163391034165,
-0.00635338900437089,-0.00328482218946166,0.),.UNSPECIFIED.);
#2605=B_SPLINE_CURVE_WITH_KNOTS('',3,(#31128,#31129,#31130,#31131,#31132,
#31133,#31134,#31135,#31136,#31137,#31138),.UNSPECIFIED.,.F.,.F.,(4,1,1,
1,1,1,1,1,4),(15.7079632679489,15.851694142003,16.8492226764396,17.8467512108762,
18.8442797453128,19.8418082797494,20.839336814186,21.8368653486226,21.9911485751285),
 .UNSPECIFIED.);
#2606=B_SPLINE_CURVE_WITH_KNOTS('',3,(#31139,#31140,#31141,#31142,#31143,
#31144,#31145,#31146,#31147,#31148),.UNSPECIFIED.,.F.,.F.,(4,1,1,1,1,1,
1,4),(15.7079632679489,16.3931980816501,17.3907266160867,18.3882551505233,
19.3857836849599,20.3833122193965,21.3808407538331,21.9911485751285),
 .UNSPECIFIED.);
#2607=B_SPLINE_CURVE_WITH_KNOTS('',3,(#31565,#31566,#31567,#31568,#31569,
#31570,#31571,#31572,#31573,#31574,#31575,#31576,#31577,#31578,#31579,#31580,
#31581,#31582,#31583,#31584,#31585,#31586,#31587,#31588,#31589,#31590,#31591,
#31592,#31593,#31594,#31595,#31596,#31597,#31598,#31599,#31600,#31601,#31602,
#31603,#31604,#31605,#31606,#31607,#31608,#31609,#31610,#31611,#31612,#31613,
#31614,#31615,#31616,#31617,#31618,#31619,#31620,#31621,#31622,#31623,#31624,
#31625,#31626,#31627,#31628,#31629,#31630,#31631,#31632,#31633,#31634,#31635,
#31636,#31637,#31638,#31639,#31640,#31641,#31642,#31643,#31644,#31645,#31646),
 .UNSPECIFIED.,.F.,.F.,(4,3,3,3,3,3,3,3,3,3,3,3,3,3,3,3,3,3,3,3,3,3,3,3,
3,3,3,4),(0.,0.0185974884483997,0.038422456578859,0.0557693036930108,0.0644714385966712,
0.0684506061088201,0.0885047864975771,0.108914714586146,0.125985344312628,
0.133848230034327,0.137284597158202,0.15835947839364,0.177197233492074,
0.197724997131683,0.205649639196346,0.209125332530892,0.230131000272577,
0.25162324878857,0.268075195219975,0.278317587273375,0.284044646363506,
0.30631363368784,0.32296601768069,0.328172641994334,0.33318402658793,0.355705441161373,
0.37292316965924,0.376940817211689),.UNSPECIFIED.);
#2608=B_SPLINE_CURVE_WITH_KNOTS('',3,(#31647,#31648,#31649,#31650,#31651,
#31652,#31653,#31654,#31655,#31656,#31657,#31658,#31659,#31660,#31661,#31662,
#31663,#31664,#31665,#31666,#31667,#31668,#31669,#31670,#31671),
 .UNSPECIFIED.,.F.,.F.,(4,3,3,3,3,3,3,3,4),(-10.1295685708719,-9.975285344366,
-8.9777568099294,-7.9802282754928,-6.9826997410562,-5.98517120661959,-4.98764267218299,
-3.9901141377464,-3.8463832636923),.UNSPECIFIED.);
#2609=B_SPLINE_CURVE_WITH_KNOTS('',3,(#32088,#32089,#32090,#32091,#32092,
#32093,#32094,#32095,#32096,#32097,#32098,#32099,#32100,#32101,#32102,#32103,
#32104,#32105,#32106,#32107,#32108,#32109),.UNSPECIFIED.,.F.,.F.,(4,3,3,
3,3,3,3,4),(7.59300756235153,7.98022827549279,8.97775680992939,9.97528534436599,
10.9728138788026,11.9703424132392,12.9678709476758,13.8761928695311),
 .UNSPECIFIED.);
#2610=B_SPLINE_CURVE_WITH_KNOTS('',3,(#32110,#32111,#32112,#32113,#32114,
#32115,#32116,#32117,#32118,#32119,#32120,#32121,#32122,#32123,#32124,#32125,
#32126,#32127,#32128,#32129,#32130,#32131,#32132,#32133,#32134,#32135,#32136,
#32137,#32138,#32139,#32140,#32141,#32142,#32143,#32144,#32145,#32146,#32147,
#32148,#32149,#32150,#32151,#32152,#32153,#32154,#32155,#32156,#32157,#32158,
#32159,#32160,#32161,#32162,#32163,#32164,#32165,#32166,#32167,#32168,#32169,
#32170,#32171,#32172,#32173,#32174,#32175,#32176,#32177,#32178,#32179,#32180,
#32181,#32182,#32183,#32184,#32185,#32186,#32187,#32188,#32189,#32190,#32191,
#32192,#32193,#32194),.UNSPECIFIED.,.F.,.F.,(4,3,3,3,3,3,3,3,3,3,3,3,3,
3,3,3,3,3,3,3,3,3,3,3,3,3,3,3,4),(0.,0.0219661245323709,0.0445435973437788,
0.0636200876317427,0.0720969450783383,0.0767544142172396,0.0810485394126128,
0.102995140020355,0.124771438188379,0.142867458553157,0.150422749787228,
0.153917805670854,0.15756664284234,0.178337401835923,0.197155519647491,
0.219426672701635,0.224328240299076,0.229401233191324,0.250066318299861,
0.27072713341503,0.285676242163978,0.296892236301983,0.30062314509683,0.320395498999285,
0.33430219613105,0.338768604407738,0.35779368297658,0.375324744080643,0.37862159683149),
 .UNSPECIFIED.);
#2611=B_SPLINE_CURVE_WITH_KNOTS('',3,(#32197,#32198,#32199,#32200,#32201,
#32202,#32203,#32204,#32205,#32206,#32207,#32208,#32209,#32210,#32211,#32212,
#32213,#32214,#32215,#32216,#32217,#32218,#32219,#32220,#32221,#32222,#32223,
#32224,#32225,#32226,#32227,#32228,#32229,#32230,#32231,#32232,#32233,#32234,
#32235,#32236,#32237,#32238,#32239,#32240,#32241,#32242,#32243,#32244,#32245,
#32246,#32247,#32248,#32249,#32250,#32251,#32252,#32253,#32254,#32255,#32256,
#32257,#32258,#32259,#32260,#32261,#32262,#32263,#32264,#32265,#32266,#32267,
#32268,#32269,#32270,#32271,#32272,#32273,#32274,#32275,#32276,#32277,#32278,
#32279,#32280,#32281,#32282,#32283,#32284),.UNSPECIFIED.,.F.,.F.,(4,3,3,
3,3,3,3,3,3,3,3,3,3,3,3,3,3,3,3,3,3,3,3,3,3,3,3,3,3,4),(-0.378621596831488,
-0.359797481501605,-0.347859545826129,-0.339721221124185,-0.335383627670914,
-0.315511917204206,-0.3011776216226,-0.297260622327209,-0.293227215665992,
-0.27282496017426,-0.252127303658145,-0.239304865881448,-0.228805565513104,
-0.224505139143286,-0.203200583084544,-0.200837552551356,-0.180350253956889,
-0.158310757112766,-0.154330327284575,-0.150809440304414,-0.129426169815667,
-0.10759199940592,-0.0856253777649029,-0.0802031337731618,-0.0759441802619393,
-0.0533966069861228,-0.030824437843487,-0.0087658011087857,-0.00403427920390734,
0.),.UNSPECIFIED.);
#2612=B_SPLINE_CURVE_WITH_KNOTS('',3,(#32285,#32286,#32287,#32288,#32289,
#32290,#32291,#32292,#32293,#32294,#32295,#32296,#32297,#32298,#32299,#32300,
#32301,#32302,#32303,#32304,#32305,#32306,#32307,#32308,#32309,#32310,#32311,
#32312,#32313,#32314,#32315,#32316,#32317,#32318,#32319,#32320,#32321,#32322,
#32323,#32324,#32325,#32326,#32327,#32328,#32329,#32330,#32331,#32332,#32333,
#32334,#32335,#32336,#32337,#32338,#32339,#32340,#32341,#32342,#32343,#32344,
#32345,#32346,#32347,#32348,#32349,#32350,#32351,#32352,#32353,#32354,#32355,
#32356,#32357,#32358,#32359,#32360,#32361,#32362,#32363,#32364,#32365,#32366,
#32367,#32368,#32369),.UNSPECIFIED.,.F.,.F.,(4,3,3,3,3,3,3,3,3,3,3,3,3,
3,3,3,3,3,3,3,3,3,3,3,3,3,3,3,4),(-0.376940817211602,-0.354634293861075,
-0.33291286533847,-0.328064572493281,-0.305815972928742,-0.290196834522679,
-0.284261035801492,-0.278600437373896,-0.256917267743233,-0.23569970803568,
-0.214947486273917,-0.208197201094579,-0.204402057890941,-0.18382592692174,
-0.180862865680237,-0.159880209131733,-0.140305785763948,-0.136021311207514,
-0.132587899444004,-0.112128580894037,-0.0917639906987552,-0.0718357453221696,
-0.067621652583724,-0.0636601371117171,-0.0441022523717969,-0.0249163234274699,
-0.00635336509323165,-0.00328482218945463,0.),.UNSPECIFIED.);
#2613=B_SPLINE_CURVE_WITH_KNOTS('',3,(#32371,#32372,#32373,#32374,#32375,
#32376,#32377,#32378,#32379,#32380,#32381),.UNSPECIFIED.,.F.,.F.,(4,1,1,
1,1,1,1,1,4),(15.7079632679489,15.851694142003,16.8492226764396,17.8467512108762,
18.8442797453128,19.8418082797494,20.839336814186,21.8368653486226,21.9911485751284),
 .UNSPECIFIED.);
#2614=B_SPLINE_CURVE_WITH_KNOTS('',3,(#32382,#32383,#32384,#32385,#32386,
#32387,#32388,#32389,#32390,#32391),.UNSPECIFIED.,.F.,.F.,(4,1,1,1,1,1,
1,4),(15.7079632679489,16.3931980816501,17.3907266160867,18.3882551505233,
19.3857836849599,20.3833122193965,21.3808407538331,21.9911485751284),
 .UNSPECIFIED.);
#2615=B_SPLINE_CURVE_WITH_KNOTS('',3,(#32808,#32809,#32810,#32811,#32812,
#32813,#32814,#32815,#32816,#32817,#32818,#32819,#32820,#32821,#32822,#32823,
#32824,#32825,#32826,#32827,#32828,#32829,#32830,#32831,#32832,#32833,#32834,
#32835,#32836,#32837,#32838,#32839,#32840,#32841,#32842,#32843,#32844,#32845,
#32846,#32847,#32848,#32849,#32850,#32851,#32852,#32853,#32854,#32855,#32856,
#32857,#32858,#32859,#32860,#32861,#32862,#32863,#32864,#32865,#32866,#32867,
#32868,#32869,#32870,#32871,#32872,#32873,#32874,#32875,#32876,#32877,#32878,
#32879,#32880,#32881,#32882,#32883,#32884,#32885,#32886,#32887,#32888,#32889),
 .UNSPECIFIED.,.F.,.F.,(4,3,3,3,3,3,3,3,3,3,3,3,3,3,3,3,3,3,3,3,3,3,3,3,
3,3,3,4),(0.,0.018597475715232,0.0384224454373358,0.0557692939441765,0.0644714217242545,
0.0684506017224621,0.0885047730237999,0.108914697191781,0.125985331266851,
0.133848209495266,0.137284586474664,0.158359468894701,0.177197233492062,
0.197725003512179,0.205649642568506,0.209125334915843,0.230131010156213,
0.251623262619965,0.268075192018812,0.278317579898386,0.28404464818755,
0.306313635980069,0.322966019399851,0.328172645794683,0.333184028513746,
0.355705443028296,0.372923169659198,0.376940817211644),.UNSPECIFIED.);
#2616=B_SPLINE_CURVE_WITH_KNOTS('',3,(#32890,#32891,#32892,#32893,#32894,
#32895,#32896,#32897,#32898,#32899,#32900,#32901,#32902,#32903,#32904,#32905,
#32906,#32907,#32908,#32909,#32910,#32911,#32912,#32913,#32914),
 .UNSPECIFIED.,.F.,.F.,(4,3,3,3,3,3,3,3,4),(-10.1295685708719,-9.975285344366,
-8.9777568099294,-7.9802282754928,-6.9826997410562,-5.9851712066196,-4.987642672183,
-3.9901141377464,-3.84638326369226),.UNSPECIFIED.);
#2617=B_SPLINE_CURVE_WITH_KNOTS('',3,(#33331,#33332,#33333,#33334,#33335,
#33336,#33337,#33338,#33339,#33340,#33341,#33342,#33343,#33344,#33345,#33346,
#33347,#33348,#33349,#33350,#33351,#33352),.UNSPECIFIED.,.F.,.F.,(4,3,3,
3,3,3,3,4),(7.59300756235149,7.9802282754928,8.97775680992939,9.975285344366,
10.9728138788026,11.9703424132392,12.9678709476758,13.8761928695311),
 .UNSPECIFIED.);
#2618=B_SPLINE_CURVE_WITH_KNOTS('',3,(#33353,#33354,#33355,#33356,#33357,
#33358,#33359,#33360,#33361,#33362,#33363,#33364,#33365,#33366,#33367,#33368,
#33369,#33370,#33371,#33372,#33373,#33374,#33375,#33376,#33377,#33378,#33379,
#33380,#33381,#33382,#33383,#33384,#33385,#33386,#33387,#33388,#33389,#33390,
#33391,#33392,#33393,#33394,#33395,#33396,#33397,#33398,#33399,#33400,#33401,
#33402,#33403,#33404,#33405,#33406,#33407,#33408,#33409,#33410,#33411,#33412,
#33413,#33414,#33415,#33416,#33417,#33418,#33419,#33420,#33421,#33422,#33423,
#33424,#33425,#33426,#33427,#33428,#33429,#33430,#33431,#33432,#33433,#33434,
#33435,#33436,#33437),.UNSPECIFIED.,.F.,.F.,(4,3,3,3,3,3,3,3,3,3,3,3,3,
3,3,3,3,3,3,3,3,3,3,3,3,3,3,3,4),(0.,0.021966136475729,0.0445436104424182,
0.0636200990930523,0.0720969484993908,0.076754421458333,0.0810485413537662,
0.102995141729322,0.124771436295877,0.142867457133781,0.150422750419918,
0.153917809521016,0.157566644049533,0.178337399455209,0.197155519647491,
0.219426672701638,0.224328239353299,0.229401233155315,0.250066318737277,
0.270727133433929,0.285676231370121,0.296892217575307,0.300623139776961,
0.320395489436602,0.334302180285225,0.338768589797073,0.357793661628995,
0.375324744080664,0.378621596831513),.UNSPECIFIED.);
#2619=B_SPLINE_CURVE_WITH_KNOTS('',3,(#33440,#33441,#33442,#33443,#33444,
#33445,#33446,#33447,#33448,#33449,#33450,#33451,#33452,#33453,#33454,#33455,
#33456,#33457,#33458,#33459,#33460,#33461,#33462,#33463,#33464,#33465,#33466,
#33467,#33468,#33469,#33470,#33471,#33472,#33473,#33474,#33475,#33476,#33477,
#33478,#33479,#33480,#33481,#33482,#33483,#33484,#33485,#33486,#33487,#33488,
#33489,#33490,#33491,#33492,#33493,#33494,#33495,#33496,#33497,#33498,#33499,
#33500,#33501,#33502,#33503,#33504,#33505,#33506,#33507,#33508,#33509,#33510,
#33511,#33512,#33513,#33514,#33515,#33516,#33517,#33518,#33519,#33520,#33521,
#33522,#33523,#33524,#33525,#33526,#33527),.UNSPECIFIED.,.F.,.F.,(4,3,3,
3,3,3,3,3,3,3,3,3,3,3,3,3,3,3,3,3,3,3,3,3,3,3,3,3,3,4),(-0.37862159683143,
-0.359797501318257,-0.347859596220205,-0.339721673305066,-0.335383849687154,
-0.315512157696412,-0.301177832053279,-0.297261100044044,-0.29322727751319,
-0.272825036004271,-0.252127377552038,-0.239304921301865,-0.228805647209281,
-0.224505165286516,-0.203200608394255,-0.200837552551346,-0.180350240469658,
-0.158310745311439,-0.154330248529997,-0.150809426102653,-0.129426144653503,
-0.107591969385708,-0.0856253476495468,-0.0802030812324167,-0.0759441620234358,
-0.0533965864690057,-0.0308244177267148,-0.00876577872099265,-0.00403427920390747,
0.),.UNSPECIFIED.);
#2620=B_SPLINE_CURVE_WITH_KNOTS('',3,(#33528,#33529,#33530,#33531,#33532,
#33533,#33534,#33535,#33536,#33537,#33538,#33539,#33540,#33541,#33542,#33543,
#33544,#33545,#33546,#33547,#33548,#33549,#33550,#33551,#33552,#33553,#33554,
#33555,#33556,#33557,#33558,#33559,#33560,#33561,#33562,#33563,#33564,#33565,
#33566,#33567,#33568,#33569,#33570,#33571,#33572,#33573,#33574,#33575,#33576,
#33577,#33578,#33579,#33580,#33581,#33582,#33583,#33584,#33585,#33586,#33587,
#33588,#33589,#33590,#33591,#33592,#33593,#33594,#33595,#33596,#33597,#33598,
#33599,#33600,#33601,#33602,#33603,#33604,#33605,#33606,#33607,#33608,#33609,
#33610,#33611,#33612),.UNSPECIFIED.,.F.,.F.,(4,3,3,3,3,3,3,3,3,3,3,3,3,
3,3,3,3,3,3,3,3,3,3,3,3,3,3,3,4),(-0.376940817211612,-0.354634290157469,
-0.332912862097815,-0.328064568788163,-0.305815969273377,-0.290196831324235,
-0.284261028697448,-0.278600437869163,-0.256917268853247,-0.235699710725379,
-0.214947489998165,-0.208197198698434,-0.204402058220254,-0.183825928780986,
-0.180862865680237,-0.159880209146386,-0.140305785776771,-0.136021313755173,
-0.132587901565395,-0.112128582775151,-0.0917639930231176,-0.0718357496511476,
-0.0676216646608822,-0.0636601411314518,-0.0441022574876565,-0.0249163309364235,
-0.00635337653324212,-0.00328482218946178,0.),.UNSPECIFIED.);
#2621=B_SPLINE_CURVE_WITH_KNOTS('',3,(#33614,#33615,#33616,#33617,#33618,
#33619,#33620,#33621,#33622,#33623,#33624),.UNSPECIFIED.,.F.,.F.,(4,1,1,
1,1,1,1,1,4),(15.7079632679489,15.851694142003,16.8492226764396,17.8467512108762,
18.8442797453128,19.8418082797494,20.839336814186,21.8368653486226,21.9911485751285),
 .UNSPECIFIED.);
#2622=B_SPLINE_CURVE_WITH_KNOTS('',3,(#33625,#33626,#33627,#33628,#33629,
#33630,#33631,#33632,#33633,#33634),.UNSPECIFIED.,.F.,.F.,(4,1,1,1,1,1,
1,4),(15.7079632679489,16.3931980816501,17.3907266160867,18.3882551505233,
19.3857836849599,20.3833122193965,21.3808407538331,21.9911485751285),
 .UNSPECIFIED.);
#2623=B_SPLINE_CURVE_WITH_KNOTS('',3,(#34051,#34052,#34053,#34054,#34055,
#34056,#34057,#34058,#34059,#34060,#34061,#34062,#34063,#34064,#34065,#34066,
#34067,#34068,#34069,#34070,#34071,#34072,#34073,#34074,#34075,#34076,#34077,
#34078,#34079,#34080,#34081,#34082,#34083,#34084,#34085,#34086,#34087,#34088,
#34089,#34090,#34091,#34092,#34093,#34094,#34095,#34096,#34097,#34098,#34099,
#34100,#34101,#34102,#34103,#34104,#34105,#34106,#34107,#34108,#34109,#34110,
#34111,#34112,#34113,#34114,#34115,#34116,#34117,#34118,#34119,#34120,#34121,
#34122,#34123,#34124,#34125,#34126,#34127,#34128,#34129,#34130,#34131,#34132),
 .UNSPECIFIED.,.F.,.F.,(4,3,3,3,3,3,3,3,3,3,3,3,3,3,3,3,3,3,3,3,3,3,3,3,
3,3,3,4),(0.,0.0185974817976789,0.038422450759474,0.0557692986010447,0.0644714297839629,
0.06845060381893,0.0885047794607919,0.108914705501413,0.12598533749907,
0.133848219307247,0.137284591577423,0.158359473431624,0.17719723349204,
0.197725000464005,0.205649640957615,0.209125333762854,0.230131005420896,
0.251623255998715,0.26807519355603,0.278317583444313,0.284044647320971,
0.306313634890073,0.322966018582345,0.328172643984831,0.333184027594933,
0.355705442137259,0.37292316965916,0.376940817211606),.UNSPECIFIED.);
#2624=B_SPLINE_CURVE_WITH_KNOTS('',3,(#34133,#34134,#34135,#34136,#34137,
#34138,#34139,#34140,#34141,#34142,#34143,#34144,#34145,#34146,#34147,#34148,
#34149,#34150,#34151,#34152,#34153,#34154,#34155,#34156,#34157),
 .UNSPECIFIED.,.F.,.F.,(4,3,3,3,3,3,3,3,4),(-10.1295685708719,-9.975285344366,
-8.9777568099294,-7.9802282754928,-6.9826997410562,-5.9851712066196,-4.98764267218299,
-3.9901141377464,-3.8463832636923),.UNSPECIFIED.);
#2625=B_SPLINE_CURVE_WITH_KNOTS('',3,(#34574,#34575,#34576,#34577,#34578,
#34579,#34580,#34581,#34582,#34583,#34584,#34585,#34586,#34587,#34588,#34589,
#34590,#34591,#34592,#34593,#34594,#34595),.UNSPECIFIED.,.F.,.F.,(4,3,3,
3,3,3,3,4),(7.59300756235153,7.98022827549279,8.97775680992939,9.97528534436599,
10.9728138788026,11.9703424132392,12.9678709476758,13.8761928695311),
 .UNSPECIFIED.);
#2626=B_SPLINE_CURVE_WITH_KNOTS('',3,(#34596,#34597,#34598,#34599,#34600,
#34601,#34602,#34603,#34604,#34605,#34606,#34607,#34608,#34609,#34610,#34611,
#34612,#34613,#34614,#34615,#34616,#34617,#34618,#34619,#34620,#34621,#34622,
#34623,#34624,#34625,#34626,#34627,#34628,#34629,#34630,#34631,#34632,#34633,
#34634,#34635,#34636,#34637,#34638,#34639,#34640,#34641,#34642,#34643,#34644,
#34645,#34646,#34647,#34648,#34649,#34650,#34651,#34652,#34653,#34654,#34655,
#34656,#34657,#34658,#34659,#34660,#34661,#34662,#34663,#34664,#34665,#34666,
#34667,#34668,#34669,#34670,#34671,#34672,#34673,#34674,#34675,#34676,#34677,
#34678,#34679,#34680),.UNSPECIFIED.,.F.,.F.,(4,3,3,3,3,3,3,3,3,3,3,3,3,
3,3,3,3,3,3,3,3,3,3,3,3,3,3,3,4),(0.,0.0219661192670637,0.0445435915688456,
0.063620082578671,0.0720969435699582,0.0767544110241794,0.0810485385530744,
0.102995139263397,0.124771439019085,0.142867459176176,0.150422749506048,
0.153917803983106,0.157566642311518,0.178337402886831,0.197155519647449,
0.219426672701589,0.224328240715824,0.229401233202951,0.250066318102677,
0.270727133401917,0.28567624690996,0.296892244536993,0.300623147437404,
0.32039550320955,0.33430220310881,0.33876861083147,0.357793692369518,0.375324744080569,
0.378621596831417),.UNSPECIFIED.);
#2627=B_SPLINE_CURVE_WITH_KNOTS('',3,(#35189,#35190,#35191,#35192,#35193,
#35194,#35195,#35196,#35197,#35198),.UNSPECIFIED.,.F.,.F.,(4,3,3,4),(-4.09254174883833,
-3.98934337020898,-2.99200752765673,-2.06514013327813),.UNSPECIFIED.);
#2628=B_SPLINE_CURVE_WITH_KNOTS('',3,(#35201,#35202,#35203,#35204,#35205,
#35206,#35207),.UNSPECIFIED.,.F.,.F.,(4,3,4),(0.,0.998006970630082,1.11419103802948),
 .UNSPECIFIED.);
#2629=B_SPLINE_CURVE_WITH_KNOTS('',3,(#35212,#35213,#35214,#35215,#35216,
#35217,#35218,#35219,#35220,#35221,#35222,#35223,#35224,#35225,#35226,#35227,
#35228,#35229,#35230,#35231,#35232,#35233),.UNSPECIFIED.,.F.,.F.,(4,3,3,
3,3,3,3,4),(-10.3757270560179,-9.97335842552244,-8.9760225829702,-7.97868674041795,
-6.9813508978657,-5.98401505531347,-4.98667921276122,-4.09254174883833),
 .UNSPECIFIED.);
#2630=B_SPLINE_CURVE_WITH_KNOTS('',3,(#35234,#35235,#35236,#35237,#35238,
#35239,#35240,#35241,#35242,#35243,#35244,#35245,#35246,#35247,#35248,#35249,
#35250,#35251,#35252,#35253,#35254,#35255),.UNSPECIFIED.,.F.,.F.,(4,3,3,
3,3,3,3,4),(1.11419103802948,1.99601394126018,2.99402091189026,3.99202788252035,
4.99003485315045,5.98804182378054,6.98604879441062,7.39737634520907),
 .UNSPECIFIED.);
#2631=B_SPLINE_CURVE_WITH_KNOTS('',3,(#35260,#35261,#35262,#35263,#35264,
#35265,#35266,#35267,#35268,#35269,#35270,#35271,#35272,#35273,#35274,#35275,
#35276,#35277,#35278,#35279,#35280,#35281),.UNSPECIFIED.,.F.,.F.,(4,3,3,
3,3,3,3,4),(-16.6589123631975,-15.9573734808359,-14.9600376382837,-13.9627017957314,
-12.9653659531792,-11.9680301106269,-10.9706942680747,-10.3757270560179),
 .UNSPECIFIED.);
#2632=B_SPLINE_CURVE_WITH_KNOTS('',3,(#35282,#35283,#35284,#35285,#35286,
#35287,#35288,#35289,#35290,#35291,#35292,#35293,#35294,#35295,#35296,#35297,
#35298,#35299,#35300,#35301,#35302,#35303),.UNSPECIFIED.,.F.,.F.,(4,3,3,
3,3,3,3,4),(7.39737634520907,7.98405576504071,8.9820627356708,9.98006970630089,
10.978076676931,11.9760836475611,12.9740906181912,13.6805616523887),
 .UNSPECIFIED.);
#2633=B_SPLINE_CURVE_WITH_KNOTS('',3,(#35308,#35309,#35310,#35311,#35312,
#35313,#35314,#35315,#35316,#35317,#35318,#35319,#35320,#35321,#35322,#35323,
#35324,#35325,#35326,#35327,#35328,#35329,#35330,#35331,#35332),
 .UNSPECIFIED.,.F.,.F.,(4,3,3,3,3,3,3,3,4),(-22.9420976703771,-22.9387243787016,
-21.9413885361494,-20.9440526935971,-19.9467168510449,-18.9493810084926,
-17.9520451659404,-16.9547093233881,-16.6589123631975),.UNSPECIFIED.);
#2634=B_SPLINE_CURVE_WITH_KNOTS('',3,(#35333,#35334,#35335,#35336,#35337,
#35338,#35339,#35340,#35341,#35342,#35343,#35344,#35345,#35346,#35347,#35348,
#35349,#35350,#35351,#35352,#35353,#35354,#35355,#35356,#35357),
 .UNSPECIFIED.,.F.,.F.,(4,3,3,3,3,3,3,3,4),(13.6805616523887,13.9720975888212,
14.9701045594513,15.9681115300814,16.9661185007115,17.9641254713416,18.9621324419717,
19.9601394126018,19.9637469595682),.UNSPECIFIED.);
#2635=B_SPLINE_CURVE_WITH_KNOTS('',3,(#35362,#35363,#35364,#35365,#35366,
#35367,#35368,#35369,#35370,#35371,#35372,#35373,#35374,#35375,#35376,#35377,
#35378,#35379,#35380,#35381,#35382,#35383),.UNSPECIFIED.,.F.,.F.,(4,3,3,
3,3,3,3,4),(-29.2252829775567,-28.9227394340151,-27.9254035914628,-26.9280677489106,
-25.9307319063583,-24.9333960638061,-23.9360602212539,-22.9420976703771),
 .UNSPECIFIED.);
#2636=B_SPLINE_CURVE_WITH_KNOTS('',3,(#35384,#35385,#35386,#35387,#35388,
#35389,#35390,#35391,#35392,#35393,#35394,#35395,#35396,#35397,#35398,#35399,
#35400,#35401,#35402,#35403,#35404,#35405),.UNSPECIFIED.,.F.,.F.,(4,3,3,
3,3,3,3,4),(19.9637469595682,20.9581463832319,21.956153353862,22.954160324492,
23.9521672951221,24.9501742657522,25.9481812363823,26.2469322667478),
 .UNSPECIFIED.);
#2637=B_SPLINE_CURVE_WITH_KNOTS('',3,(#35410,#35411,#35412,#35413,#35414,
#35415,#35416,#35417,#35418,#35419,#35420,#35421,#35422,#35423,#35424,#35425,
#35426,#35427,#35428,#35429,#35430,#35431),.UNSPECIFIED.,.F.,.F.,(4,3,3,
3,3,3,3,4),(-35.5084682847363,-34.9067544893285,-33.9094186467763,-32.9120828042241,
-31.9147469616718,-30.9174111191196,-29.9200752765673,-29.2252829775567),
 .UNSPECIFIED.);
#2638=B_SPLINE_CURVE_WITH_KNOTS('',3,(#35432,#35433,#35434,#35435,#35436,
#35437,#35438,#35439,#35440,#35441,#35442,#35443,#35444,#35445,#35446,#35447,
#35448,#35449,#35450,#35451,#35452,#35453),.UNSPECIFIED.,.F.,.F.,(4,3,3,
3,3,3,3,4),(26.2469322667478,26.9461882070124,27.9441951776425,28.9422021482726,
29.9402091189027,30.9382160895327,31.9362230601628,32.5301175739274),
 .UNSPECIFIED.);
#2639=B_SPLINE_CURVE_WITH_KNOTS('',3,(#35458,#35459,#35460,#35461,#35462,
#35463,#35464,#35465,#35466,#35467,#35468,#35469,#35470,#35471,#35472,#35473,
#35474,#35475,#35476,#35477,#35478,#35479),.UNSPECIFIED.,.F.,.F.,(4,3,3,
3,3,3,3,4),(-41.7916535919159,-40.890769544642,-39.8934337020898,-38.8960978595375,
-37.8987620169853,-36.901426174433,-35.9040903318808,-35.5084682847363),
 .UNSPECIFIED.);
#2640=B_SPLINE_CURVE_WITH_KNOTS('',3,(#35480,#35481,#35482,#35483,#35484,
#35485,#35486,#35487,#35488,#35489,#35490,#35491,#35492,#35493,#35494,#35495,
#35496,#35497,#35498,#35499,#35500,#35501),.UNSPECIFIED.,.F.,.F.,(4,3,3,
3,3,3,3,4),(32.5301175739274,32.9342300307929,33.932237001423,34.9302439720531,
35.9282509426832,36.9262579133133,37.9242648839434,38.813302881107),
 .UNSPECIFIED.);
#2641=B_SPLINE_CURVE_WITH_KNOTS('',3,(#35506,#35507,#35508,#35509,#35510,
#35511,#35512,#35513,#35514,#35515,#35516,#35517,#35518,#35519,#35520,#35521,
#35522,#35523,#35524,#35525,#35526,#35527,#35528,#35529,#35530),
 .UNSPECIFIED.,.F.,.F.,(4,3,3,3,3,3,3,3,4),(-48.0748388990955,-47.8721204425077,
-46.8747845999555,-45.8774487574032,-44.880112914851,-43.8827770722987,
-42.8854412297465,-41.8881053871943,-41.7916535919159),.UNSPECIFIED.);
#2642=B_SPLINE_CURVE_WITH_KNOTS('',3,(#35531,#35532,#35533,#35534,#35535,
#35536,#35537,#35538,#35539,#35540,#35541,#35542,#35543,#35544,#35545,#35546,
#35547,#35548,#35549,#35550,#35551,#35552,#35553,#35554,#35555),
 .UNSPECIFIED.,.F.,.F.,(4,3,3,3,3,3,3,3,4),(38.813302881107,38.9222718545735,
39.9202788252036,40.9182857958337,41.9162927664637,42.9142997370938,43.9123067077239,
44.910313678354,45.0964881882866),.UNSPECIFIED.);
#2643=B_SPLINE_CURVE_WITH_KNOTS('',3,(#35560,#35561,#35562,#35563,#35564,
#35565,#35566,#35567,#35568,#35569,#35570,#35571,#35572,#35573,#35574,#35575,
#35576,#35577,#35578,#35579,#35580,#35581),.UNSPECIFIED.,.F.,.F.,(4,3,3,
3,3,3,3,4),(-54.3580242062751,-53.8561354978212,-52.8587996552689,-51.8614638127167,
-50.8641279701645,-49.8667921276122,-48.86945628506,-48.0748388990955),
 .UNSPECIFIED.);
#2644=B_SPLINE_CURVE_WITH_KNOTS('',3,(#35582,#35583,#35584,#35585,#35586,
#35587,#35588,#35589,#35590,#35591,#35592,#35593,#35594,#35595,#35596,#35597,
#35598,#35599,#35600,#35601,#35602,#35603),.UNSPECIFIED.,.F.,.F.,(4,3,3,
3,3,3,3,4),(45.0964881882866,45.9083206489841,46.9063276196142,47.9043345902443,
48.9023415608744,49.9003485315045,50.8983555021345,51.3796734954662),
 .UNSPECIFIED.);
#2645=B_SPLINE_CURVE_WITH_KNOTS('',3,(#35608,#35609,#35610,#35611,#35612,
#35613,#35614,#35615,#35616,#35617,#35618,#35619,#35620,#35621,#35622,#35623,
#35624,#35625,#35626,#35627,#35628,#35629),.UNSPECIFIED.,.F.,.F.,(4,3,3,
3,3,3,3,4),(-60.6412095134546,-59.8401505531347,-58.8428147105824,-57.8454788680302,
-56.8481430254779,-55.8508071829257,-54.8534713403734,-54.3580242062751),
 .UNSPECIFIED.);
#2646=B_SPLINE_CURVE_WITH_KNOTS('',3,(#35630,#35631,#35632,#35633,#35634,
#35635,#35636,#35637,#35638,#35639,#35640,#35641,#35642,#35643,#35644,#35645,
#35646,#35647,#35648,#35649,#35650,#35651),.UNSPECIFIED.,.F.,.F.,(4,3,3,
3,3,3,3,4),(51.3796734954662,51.8963624727646,52.8943694433947,53.8923764140248,
54.8903833846549,55.888390355285,56.8863973259151,57.6628588026458),
 .UNSPECIFIED.);
#2647=B_SPLINE_CURVE_WITH_KNOTS('',3,(#35656,#35657,#35658,#35659,#35660,
#35661,#35662,#35663,#35664,#35665,#35666,#35667,#35668,#35669,#35670,#35671,
#35672,#35673,#35674,#35675,#35676,#35677,#35678,#35679,#35680),
 .UNSPECIFIED.,.F.,.F.,(4,3,3,3,3,3,3,3,4),(-66.9243948206342,-66.8215014510004,
-65.8241656084481,-64.8268297658959,-63.8294939233436,-62.8321580807914,
-61.8348222382391,-60.8374863956869,-60.6412095134546),.UNSPECIFIED.);
#2648=B_SPLINE_CURVE_WITH_KNOTS('',3,(#35681,#35682,#35683,#35684,#35685,
#35686,#35687,#35688,#35689,#35690,#35691,#35692,#35693,#35694,#35695,#35696,
#35697,#35698,#35699,#35700,#35701,#35702,#35703,#35704,#35705),
 .UNSPECIFIED.,.F.,.F.,(4,3,3,3,3,3,3,3,4),(57.6628588026458,57.8844042965452,
58.8824112671752,59.8804182378054,60.8784252084354,61.8764321790655,62.8744391496956,
63.8724461203257,63.9460441098254),.UNSPECIFIED.);
#2649=B_SPLINE_CURVE_WITH_KNOTS('',3,(#35710,#35711,#35712,#35713,#35714,
#35715,#35716,#35717,#35718,#35719,#35720,#35721,#35722,#35723,#35724,#35725,
#35726,#35727,#35728,#35729,#35730,#35731),.UNSPECIFIED.,.F.,.F.,(4,3,3,
3,3,3,3,4),(-73.2075801278138,-72.8055165063138,-71.8081806637616,-70.8108448212093,
-69.8135089786571,-68.8161731361048,-67.8188372935526,-66.9243948206342),
 .UNSPECIFIED.);
#2650=B_SPLINE_CURVE_WITH_KNOTS('',3,(#35732,#35733,#35734,#35735,#35736,
#35737,#35738,#35739,#35740,#35741,#35742,#35743,#35744,#35745,#35746,#35747,
#35748,#35749,#35750,#35751,#35752,#35753),.UNSPECIFIED.,.F.,.F.,(4,3,3,
3,3,3,3,4),(63.9460441098254,64.8704530909558,65.8684600615859,66.866467032216,
67.8644740028461,68.8624809734761,69.8604879441062,70.229229417005),
 .UNSPECIFIED.);
#2651=B_SPLINE_CURVE_WITH_KNOTS('',3,(#35758,#35759,#35760,#35761,#35762,
#35763,#35764,#35765,#35766,#35767,#35768,#35769,#35770,#35771,#35772,#35773,
#35774,#35775,#35776,#35777,#35778,#35779),.UNSPECIFIED.,.F.,.F.,(4,3,3,
3,3,3,3,4),(-79.4907654349934,-78.7895315616273,-77.792195719075,-76.7948598765228,
-75.7975240339705,-74.8001881914183,-73.802852348866,-73.2075801278138),
 .UNSPECIFIED.);
#2652=B_SPLINE_CURVE_WITH_KNOTS('',3,(#35780,#35781,#35782,#35783,#35784,
#35785,#35786,#35787,#35788,#35789,#35790,#35791,#35792,#35793,#35794,#35795,
#35796,#35797,#35798,#35799,#35800,#35801),.UNSPECIFIED.,.F.,.F.,(4,3,3,
3,3,3,3,4),(70.229229417005,70.8584949147363,71.8565018853664,72.8545088559965,
73.8525158266266,74.8505227972567,75.8485297678868,76.5124147241846),
 .UNSPECIFIED.);
#2653=B_SPLINE_CURVE_WITH_KNOTS('',3,(#35806,#35807,#35808,#35809,#35810,
#35811,#35812,#35813,#35814,#35815,#35816,#35817,#35818,#35819,#35820,#35821,
#35822,#35823,#35824,#35825,#35826,#35827,#35828,#35829,#35830),
 .UNSPECIFIED.,.F.,.F.,(4,3,3,3,3,3,3,3,4),(-85.773950742173,-85.770882459493,
-84.7735466169407,-83.7762107743885,-82.7788749318363,-81.781539089284,
-80.7842032467318,-79.7868674041795,-79.4907654349934),.UNSPECIFIED.);
#2654=B_SPLINE_CURVE_WITH_KNOTS('',3,(#35831,#35832,#35833,#35834,#35835,
#35836,#35837,#35838,#35839,#35840,#35841,#35842,#35843,#35844,#35845,#35846,
#35847,#35848,#35849,#35850,#35851,#35852),.UNSPECIFIED.,.F.,.F.,(4,3,3,
3,3,3,3,4),(76.5124147241846,76.8465367385169,77.8445437091469,78.842550679777,
79.8405576504071,80.8385646210372,81.8365715916673,82.7956000313642),
 .UNSPECIFIED.);
#2655=B_SPLINE_CURVE_WITH_KNOTS('',3,(#35857,#35858,#35859,#35860,#35861,
#35862,#35863,#35864,#35865,#35866,#35867,#35868,#35869,#35870,#35871,#35872,
#35873,#35874,#35875,#35876,#35877,#35878),.UNSPECIFIED.,.F.,.F.,(4,3,3,
3,3,3,3,4),(-92.0571360493526,-91.7548975148065,-90.7575616722542,-89.760225829702,
-88.7628899871497,-87.7655541445975,-86.7682183020452,-85.773950742173),
 .UNSPECIFIED.);
#2656=B_SPLINE_CURVE_WITH_KNOTS('',3,(#35879,#35880,#35881,#35882,#35883,
#35884,#35885,#35886,#35887,#35888,#35889,#35890,#35891,#35892,#35893,#35894,
#35895,#35896,#35897,#35898,#35899,#35900,#35901,#35902,#35903),
 .UNSPECIFIED.,.F.,.F.,(4,3,3,3,3,3,3,3,4),(82.7956000313642,82.8345785622974,
83.8325855329275,84.8305925035576,85.8285994741877,86.8266064448178,87.8246134154479,
88.822620386078,89.0787853385438),.UNSPECIFIED.);
#2657=B_SPLINE_CURVE_WITH_KNOTS('',3,(#35908,#35909,#35910,#35911,#35912,
#35913,#35914,#35915,#35916,#35917,#35918,#35919,#35920,#35921,#35922,#35923,
#35924,#35925,#35926,#35927,#35928,#35929),.UNSPECIFIED.,.F.,.F.,(4,3,3,
3,3,3,3,4),(-98.3403213565322,-97.7389125701199,-96.7415767275677,-95.7442408850154,
-94.7469050424632,-93.7495691999109,-92.7522333573587,-92.0571360493526),
 .UNSPECIFIED.);
#2658=B_SPLINE_CURVE_WITH_KNOTS('',3,(#35930,#35931,#35932,#35933,#35934,
#35935,#35936,#35937,#35938,#35939,#35940,#35941,#35942,#35943,#35944,#35945,
#35946,#35947,#35948,#35949,#35950,#35951),.UNSPECIFIED.,.F.,.F.,(4,3,3,
3,3,3,3,4),(89.0787853385438,89.820627356708,90.8186343273381,91.8166412979682,
92.8146482685983,93.8126552392284,94.8106622098585,95.3619706457233),
 .UNSPECIFIED.);
#2659=B_SPLINE_CURVE_WITH_KNOTS('',3,(#35957,#35958,#35959,#35960,#35961,
#35962,#35963,#35964),.UNSPECIFIED.,.F.,.F.,(4,1,1,1,1,4),(109.955742875643,
110.351669931783,111.349005774335,112.346341616887,113.343677459439,114.341013301992),
 .UNSPECIFIED.);
#2660=B_SPLINE_CURVE_WITH_KNOTS('',3,(#35967,#35968,#35969,#35970,#35971,
#35972,#35973),.UNSPECIFIED.,.F.,.F.,(4,1,1,1,4),(109.955742875643,110.107297927009,
111.105304897639,112.103311868269,113.101318838899),.UNSPECIFIED.);
#2661=B_SPLINE_CURVE_WITH_KNOTS('',3,(#35978,#35979,#35980,#35981,#35982,
#35983,#35984,#35985,#35986,#35987),.UNSPECIFIED.,.F.,.F.,(4,1,1,1,1,1,
1,4),(103.672557568463,104.367654876469,105.364990719021,106.362326561574,
107.359662404126,108.356998246678,109.35433408923,109.955742875643),
 .UNSPECIFIED.);
#2662=B_SPLINE_CURVE_WITH_KNOTS('',3,(#35988,#35989,#35990,#35991,#35992,
#35993,#35994,#35995,#35996,#35997),.UNSPECIFIED.,.F.,.F.,(4,1,1,1,1,1,
1,4),(103.672557568463,104.119256103228,105.117263073858,106.115270044488,
107.113277015118,108.111283985749,109.109290956379,109.955742875643),
 .UNSPECIFIED.);
#2663=B_SPLINE_CURVE_WITH_KNOTS('',3,(#36002,#36003,#36004,#36005,#36006,
#36007,#36008,#36009,#36010,#36011),.UNSPECIFIED.,.F.,.F.,(4,1,1,1,1,1,
1,4),(97.3893722612836,98.3836398211558,99.380975663708,100.37831150626,
101.375647348812,102.372983191365,103.370319033917,103.672557568463),
 .UNSPECIFIED.);
#2664=B_SPLINE_CURVE_WITH_KNOTS('',3,(#36012,#36013,#36014,#36015,#36016,
#36017,#36018,#36019,#36020,#36021),.UNSPECIFIED.,.F.,.F.,(4,1,1,1,1,1,
1,4),(97.3893722612836,98.1312142794477,99.1292212500778,100.127228220708,
101.125235191338,102.123242161968,103.121249132598,103.672557568463),
 .UNSPECIFIED.);
#2665=B_SPLINE_CURVE_WITH_KNOTS('',3,(#36026,#36027,#36028,#36029,#36030,
#36031,#36032,#36033,#36034,#36035,#36036),.UNSPECIFIED.,.F.,.F.,(4,1,1,
1,1,1,1,1,4),(91.106186954104,91.4022889232901,92.3996247658423,93.3969606083945,
94.3942964509468,95.391632293499,96.3889681360513,97.3863039786035,97.3893722612836),
 .UNSPECIFIED.);
#2666=B_SPLINE_CURVE_WITH_KNOTS('',3,(#36037,#36038,#36039,#36040,#36041,
#36042,#36043,#36044,#36045,#36046,#36047),.UNSPECIFIED.,.F.,.F.,(4,1,1,
1,1,1,1,1,4),(91.106186954104,91.1451654850371,92.1431724556672,93.1411794262973,
94.1391863969273,95.1371933675574,96.1352003381875,97.1332073088176,97.3893722612836),
 .UNSPECIFIED.);
#2667=B_SPLINE_CURVE_WITH_KNOTS('',3,(#36052,#36053,#36054,#36055,#36056,
#36057,#36058,#36059,#36060,#36061),.UNSPECIFIED.,.F.,.F.,(4,1,1,1,1,1,
1,4),(84.8230016469244,85.4182738679766,86.4156097105288,87.4129455530811,
88.4102813956333,89.4076172381856,90.4049530807378,91.106186954104),
 .UNSPECIFIED.);
#2668=B_SPLINE_CURVE_WITH_KNOTS('',3,(#36062,#36063,#36064,#36065,#36066,
#36067,#36068,#36069,#36070,#36071),.UNSPECIFIED.,.F.,.F.,(4,1,1,1,1,1,
1,4),(84.8230016469244,85.1571236612565,86.1551306318866,87.1531376025167,
88.1511445731468,89.1491515437769,90.147158514407,91.106186954104),
 .UNSPECIFIED.);
#2669=B_SPLINE_CURVE_WITH_KNOTS('',3,(#36076,#36077,#36078,#36079,#36080,
#36081,#36082,#36083,#36084,#36085),.UNSPECIFIED.,.F.,.F.,(4,1,1,1,1,1,
1,4),(78.5398163397448,79.4342588126631,80.4315946552154,81.4289304977676,
82.4262663403199,83.4236021828721,84.4209380254243,84.8230016469244),
 .UNSPECIFIED.);
#2670=B_SPLINE_CURVE_WITH_KNOTS('',3,(#36086,#36087,#36088,#36089,#36090,
#36091,#36092,#36093,#36094,#36095),.UNSPECIFIED.,.F.,.F.,(4,1,1,1,1,1,
1,4),(78.5398163397448,79.169081837476,80.1670888081061,81.1650957787362,
82.1631027493663,83.1611097199964,84.1591166906264,84.8230016469244),
 .UNSPECIFIED.);
#2671=B_SPLINE_CURVE_WITH_KNOTS('',3,(#36100,#36101,#36102,#36103,#36104,
#36105,#36106,#36107,#36108,#36109,#36110),.UNSPECIFIED.,.F.,.F.,(4,1,1,
1,1,1,1,1,4),(72.2566310325652,72.4529079147974,73.4502437573497,74.4475795999019,
75.4449154424541,76.4422512850064,77.4395871275586,78.4369229701109,78.5398163397448),
 .UNSPECIFIED.);
#2672=B_SPLINE_CURVE_WITH_KNOTS('',3,(#36111,#36112,#36113,#36114,#36115,
#36116,#36117,#36118,#36119,#36120),.UNSPECIFIED.,.F.,.F.,(4,1,1,1,1,1,
1,4),(72.2566310325652,73.1810400136955,74.1790469843256,75.1770539549557,
76.1750609255857,77.1730678962158,78.1710748668459,78.5398163397448),
 .UNSPECIFIED.);
#2673=B_SPLINE_CURVE_WITH_KNOTS('',3,(#36125,#36126,#36127,#36128,#36129,
#36130,#36131,#36132,#36133,#36134),.UNSPECIFIED.,.F.,.F.,(4,1,1,1,1,1,
1,4),(65.9734457253856,66.468892859484,67.4662287020362,68.4635645445884,
69.4609003871407,70.4582362296929,71.4555720722452,72.2566310325652),
 .UNSPECIFIED.);
#2674=B_SPLINE_CURVE_WITH_KNOTS('',3,(#36135,#36136,#36137,#36138,#36139,
#36140,#36141,#36142,#36143,#36144,#36145),.UNSPECIFIED.,.F.,.F.,(4,1,1,
1,1,1,1,1,4),(65.9734457253856,66.1949912192848,67.1929981899149,68.191005160545,
69.1890121311751,70.1870191018052,71.1850260724353,72.1830330430654,72.2566310325652),
 .UNSPECIFIED.);
#2675=B_SPLINE_CURVE_WITH_KNOTS('',3,(#36150,#36151,#36152,#36153,#36154,
#36155,#36156,#36157,#36158,#36159),.UNSPECIFIED.,.F.,.F.,(4,1,1,1,1,1,
1,4),(59.690260418206,60.4848778041705,61.4822136467227,62.479549489275,
63.4768853318272,64.4742211743795,65.4715570169317,65.9734457253856),
 .UNSPECIFIED.);
#2676=B_SPLINE_CURVE_WITH_KNOTS('',3,(#36160,#36161,#36162,#36163,#36164,
#36165,#36166,#36167,#36168,#36169),.UNSPECIFIED.,.F.,.F.,(4,1,1,1,1,1,
1,4),(59.690260418206,60.2069493955043,61.2049563661344,62.2029633367645,
63.2009703073946,64.1989772780247,65.1969842486548,65.9734457253856),
 .UNSPECIFIED.);
#2677=B_SPLINE_CURVE_WITH_KNOTS('',3,(#36174,#36175,#36176,#36177,#36178,
#36179,#36180,#36181,#36182,#36183,#36184),.UNSPECIFIED.,.F.,.F.,(4,1,1,
1,1,1,1,1,4),(53.4070751110265,53.5035269063048,54.500862748857,55.4981985914093,
56.4955344339615,57.4928702765138,58.490206119066,59.4875419616182,59.690260418206),
 .UNSPECIFIED.);
#2678=B_SPLINE_CURVE_WITH_KNOTS('',3,(#36185,#36186,#36187,#36188,#36189,
#36190,#36191,#36192,#36193,#36194),.UNSPECIFIED.,.F.,.F.,(4,1,1,1,1,1,
1,4),(53.4070751110264,54.2189075717238,55.2169145423539,56.214921512984,
57.212928483614,58.2109354542441,59.2089424248742,59.690260418206),
 .UNSPECIFIED.);
#2679=B_SPLINE_CURVE_WITH_KNOTS('',3,(#36199,#36200,#36201,#36202,#36203,
#36204,#36205,#36206,#36207,#36208),.UNSPECIFIED.,.F.,.F.,(4,1,1,1,1,1,
1,4),(47.1238898038469,47.5195118509913,48.5168476935436,49.5141835360958,
50.5115193786481,51.5088552212003,52.5061910637525,53.4070751110265),
 .UNSPECIFIED.);
#2680=B_SPLINE_CURVE_WITH_KNOTS('',3,(#36209,#36210,#36211,#36212,#36213,
#36214,#36215,#36216,#36217,#36218,#36219),.UNSPECIFIED.,.F.,.F.,(4,1,1,
1,1,1,1,1,4),(47.1238898038468,47.2328587773132,48.2308657479432,49.2288727185733,
50.2268796892034,51.2248866598335,52.2228936304636,53.2209006010937,53.4070751110264),
 .UNSPECIFIED.);
#2681=B_SPLINE_CURVE_WITH_KNOTS('',3,(#36224,#36225,#36226,#36227,#36228,
#36229,#36230,#36231,#36232,#36233),.UNSPECIFIED.,.F.,.F.,(4,1,1,1,1,1,
1,4),(40.8407044966673,41.5354967956779,42.5328326382301,43.5301684807823,
44.5275043233346,45.5248401658868,46.5221760084391,47.1238898038469),
 .UNSPECIFIED.);
#2682=B_SPLINE_CURVE_WITH_KNOTS('',3,(#36234,#36235,#36236,#36237,#36238,
#36239,#36240,#36241,#36242,#36243),.UNSPECIFIED.,.F.,.F.,(4,1,1,1,1,1,
1,4),(40.8407044966672,41.2448169535326,42.2428239241627,43.2408308947928,
44.2388378654229,45.236844836053,46.2348518066831,47.1238898038468),
 .UNSPECIFIED.);
#2683=B_SPLINE_CURVE_WITH_KNOTS('',3,(#36248,#36249,#36250,#36251,#36252,
#36253,#36254,#36255,#36256,#36257),.UNSPECIFIED.,.F.,.F.,(4,1,1,1,1,1,
1,4),(34.5575191894877,35.5514817403644,36.5488175829166,37.5461534254689,
38.5434892680211,39.5408251105734,40.5381609531256,40.8407044966673),
 .UNSPECIFIED.);
#2684=B_SPLINE_CURVE_WITH_KNOTS('',3,(#36258,#36259,#36260,#36261,#36262,
#36263,#36264,#36265,#36266,#36267),.UNSPECIFIED.,.F.,.F.,(4,1,1,1,1,1,
1,4),(34.5575191894876,35.2567751297521,36.2547821003822,37.2527890710123,
38.2507960416424,39.2488030122724,40.2468099829025,40.8407044966672),
 .UNSPECIFIED.);
#2685=B_SPLINE_CURVE_WITH_KNOTS('',3,(#36272,#36273,#36274,#36275,#36276,
#36277,#36278,#36279,#36280,#36281,#36282),.UNSPECIFIED.,.F.,.F.,(4,1,1,
1,1,1,1,1,4),(28.2743338823081,28.5701308424987,29.5674666850509,30.5648025276032,
31.5621383701554,32.5594742127077,33.5568100552599,34.5541458978121,34.5575191894877),
 .UNSPECIFIED.);
#2686=B_SPLINE_CURVE_WITH_KNOTS('',3,(#36283,#36284,#36285,#36286,#36287,
#36288,#36289,#36290,#36291,#36292),.UNSPECIFIED.,.F.,.F.,(4,1,1,1,1,1,
1,4),(28.274333882308,29.2687333059716,30.2667402766016,31.2647472472317,
32.2627542178618,33.2607611884919,34.258768159122,34.5575191894876),
 .UNSPECIFIED.);
#2687=B_SPLINE_CURVE_WITH_KNOTS('',3,(#36297,#36298,#36299,#36300,#36301,
#36302,#36303,#36304,#36305,#36306),.UNSPECIFIED.,.F.,.F.,(4,1,1,1,1,1,
1,4),(21.9911485751285,22.5861157871852,23.5834516297375,24.5807874722897,
25.5781233148419,26.5754591573942,27.5727949999464,28.2743338823081),
 .UNSPECIFIED.);
#2688=B_SPLINE_CURVE_WITH_KNOTS('',3,(#36307,#36308,#36309,#36310,#36311,
#36312,#36313,#36314,#36315,#36316,#36317),.UNSPECIFIED.,.F.,.F.,(4,1,1,
1,1,1,1,1,4),(21.9911485751285,22.2826845115609,23.280691482191,24.2786984528211,
25.2767054234512,26.2747123940813,27.2727193647114,28.2707263353415,28.274333882308),
 .UNSPECIFIED.);
#2689=B_SPLINE_CURVE_WITH_KNOTS('',3,(#36322,#36323,#36324,#36325,#36326,
#36327,#36328,#36329,#36330,#36331),.UNSPECIFIED.,.F.,.F.,(4,1,1,1,1,1,
1,4),(15.7079632679489,16.6021007318718,17.599436574424,18.5967724169762,
19.5941082595285,20.5914441020807,21.588779944633,21.9911485751285),
 .UNSPECIFIED.);
#2690=B_SPLINE_CURVE_WITH_KNOTS('',3,(#36332,#36333,#36334,#36335,#36336,
#36337,#36338,#36339,#36340,#36341),.UNSPECIFIED.,.F.,.F.,(4,1,1,1,1,1,
1,4),(15.7079632679489,16.2946426877804,17.2926496584105,18.2906566290406,
19.2886635996707,20.2866705703008,21.2846775409308,21.9911485751285),
 .UNSPECIFIED.);
#2691=B_SPLINE_CURVE_WITH_KNOTS('',3,(#36344,#36345,#36346,#36347,#36348,
#36349,#36350,#36351,#36352,#36353,#36354,#36355,#36356,#36357,#36358,#36359,
#36360,#36361,#36362,#36363,#36364,#36365,#36366,#36367,#36368,#36369,#36370,
#36371,#36372,#36373,#36374,#36375,#36376,#36377,#36378,#36379,#36380,#36381,
#36382,#36383,#36384,#36385,#36386,#36387,#36388,#36389,#36390,#36391,#36392,
#36393,#36394,#36395,#36396,#36397,#36398,#36399,#36400,#36401,#36402,#36403,
#36404,#36405,#36406,#36407,#36408,#36409,#36410,#36411,#36412,#36413,#36414,
#36415,#36416,#36417,#36418,#36419,#36420,#36421,#36422,#36423,#36424,#36425,
#36426,#36427,#36428,#36429,#36430,#36431,#36432,#36433,#36434,#36435,#36436,
#36437,#36438,#36439,#36440,#36441,#36442,#36443,#36444,#36445,#36446,#36447,
#36448,#36449,#36450,#36451,#36452,#36453,#36454,#36455,#36456,#36457,#36458,
#36459,#36460,#36461,#36462,#36463,#36464,#36465,#36466,#36467,#36468,#36469,
#36470),.UNSPECIFIED.,.F.,.F.,(4,3,3,3,3,3,3,3,3,3,3,3,3,3,3,3,3,3,3,3,
3,3,3,3,3,3,3,3,3,3,3,3,3,3,3,3,3,3,3,3,3,3,4),(-0.996917990983956,-0.978871588953361,
-0.96111138213616,-0.951572166884024,-0.94788730271085,-0.928958746515757,
-0.909876465942473,-0.904936500084987,-0.901848009849201,-0.882541837721487,
-0.863353532865677,-0.850071733640713,-0.842096384739765,-0.838733342910066,
-0.836789934415749,-0.818254783653573,-0.798902591036692,-0.782735584954257,
-0.778204258927876,-0.774298497031817,-0.75473106557298,-0.734923369072796,
-0.7185841623989,-0.712646708603056,-0.709110058221935,-0.689189804001172,
-0.669566542377212,-0.649891129487148,-0.644972000047888,-0.641670824784499,
-0.621885476350888,-0.601705353300825,-0.588427767916722,-0.579820295317846,
-0.575107459303169,-0.554609906499435,-0.53420632583291,-0.514845498030454,
-0.510394870356688,-0.506773348856668,-0.495484670227998,-0.475532816008266,
-0.468408511919796),.UNSPECIFIED.);
#2692=B_SPLINE_CURVE_WITH_KNOTS('',3,(#36472,#36473,#36474,#36475,#36476,
#36477,#36478,#36479,#36480,#36481,#36482,#36483,#36484,#36485,#36486,#36487,
#36488,#36489,#36490,#36491,#36492,#36493,#36494,#36495,#36496,#36497,#36498,
#36499,#36500,#36501,#36502,#36503,#36504,#36505,#36506,#36507,#36508,#36509,
#36510,#36511,#36512,#36513,#36514,#36515,#36516,#36517,#36518,#36519,#36520,
#36521,#36522,#36523,#36524,#36525,#36526,#36527,#36528,#36529),
 .UNSPECIFIED.,.F.,.F.,(4,3,3,3,3,3,3,3,3,3,3,3,3,3,3,3,3,3,3,4),(-0.271362855059921,
-0.249815156703991,-0.228817954605844,-0.214757059032555,-0.202695986178297,
-0.199258382274391,-0.179079040584676,-0.172574372312687,-0.151002575773601,
-0.132127253801901,-0.128545223737615,-0.108660382312346,-0.0889046320299183,
-0.0695673553379917,-0.0643976613730527,-0.0611873083345303,-0.0424332578302701,
-0.0240014673407122,-0.00610701619818059,0.),.UNSPECIFIED.);
#2693=B_SPLINE_CURVE_WITH_KNOTS('',3,(#36532,#36533,#36534,#36535,#36536,
#36537,#36538,#36539,#36540,#36541,#36542,#36543,#36544,#36545,#36546,#36547,
#36548,#36549,#36550,#36551,#36552,#36553,#36554,#36555,#36556,#36557,#36558,
#36559,#36560,#36561,#36562,#36563,#36564,#36565,#36566,#36567,#36568,#36569,
#36570,#36571,#36572,#36573,#36574,#36575,#36576,#36577,#36578,#36579,#36580,
#36581,#36582,#36583,#36584,#36585,#36586,#36587,#36588,#36589,#36590,#36591,
#36592,#36593,#36594,#36595,#36596,#36597,#36598,#36599,#36600,#36601,#36602,
#36603,#36604,#36605,#36606,#36607,#36608,#36609,#36610,#36611,#36612,#36613,
#36614,#36615,#36616,#36617,#36618,#36619,#36620,#36621,#36622,#36623,#36624,
#36625,#36626,#36627,#36628,#36629,#36630,#36631,#36632,#36633,#36634),
 .UNSPECIFIED.,.F.,.F.,(4,3,3,3,3,3,3,3,3,3,3,3,3,3,3,3,3,3,3,3,3,3,3,3,
3,3,3,3,3,3,3,3,3,3,4),(-0.468408511919796,-0.449159592277506,-0.442679572366002,
-0.439139523917826,-0.418501747794262,-0.397540534942074,-0.376759689901926,
-0.369408338867191,-0.366188435771172,-0.344993296658329,-0.324164935680159,
-0.314417154781481,-0.302674036643168,-0.298303152413865,-0.294792657786698,
-0.273759483634418,-0.252453791079512,-0.23671297526563,-0.228622459040654,
-0.22484613779528,-0.221071692886511,-0.199520974492535,-0.177947952659577,
-0.156760757052952,-0.151824997028116,-0.148277425274246,-0.12652726456846,
-0.105236270462937,-0.0835127492652271,-0.0784406535722348,-0.0733870619889256,
-0.0516031153801045,-0.029512914496819,-0.0074997402847098,0.),
 .UNSPECIFIED.);
#2694=B_SPLINE_CURVE_WITH_KNOTS('',3,(#37063,#37064,#37065,#37066,#37067,
#37068,#37069,#37070),.UNSPECIFIED.,.F.,.F.,(4,1,1,1,1,4),(11.6154215191105,
12.6127573616628,13.610093204215,14.6074290467673,15.6047648893195,15.7079632679489),
 .UNSPECIFIED.);
#2695=B_SPLINE_CURVE_WITH_KNOTS('',3,(#37071,#37072,#37073,#37074,#37075,
#37076,#37077,#37078,#37079,#37080,#37081,#37082,#37083,#37084,#37085,#37086,
#37087,#37088,#37089,#37090,#37091,#37092,#37093,#37094,#37095,#37096,#37097,
#37098,#37099,#37100,#37101,#37102,#37103,#37104,#37105,#37106,#37107,#37108,
#37109,#37110,#37111,#37112,#37113,#37114,#37115,#37116,#37117,#37118,#37119,
#37120,#37121,#37122,#37123,#37124,#37125,#37126,#37127,#37128,#37129,#37130,
#37131,#37132,#37133,#37134,#37135,#37136,#37137,#37138,#37139,#37140,#37141,
#37142,#37143,#37144,#37145,#37146,#37147,#37148,#37149,#37150,#37151,#37152,
#37153,#37154,#37155),.UNSPECIFIED.,.F.,.F.,(4,3,3,3,3,3,3,3,3,3,3,3,3,
3,3,3,3,3,3,3,3,3,3,3,3,3,3,3,4),(-0.364629307890661,-0.350885759085945,
-0.329296488089375,-0.318978386270927,-0.313741431878983,-0.309365163672801,
-0.288042901568511,-0.272809238661881,-0.264006177467146,-0.26029818106468,
-0.239567096461013,-0.219346880276472,-0.206053559786221,-0.194876880502573,
-0.191399047668888,-0.171813366976952,-0.166173598315468,-0.145401898526034,
-0.126706873608775,-0.123379860192083,-0.103925496661725,-0.0845481894111439,
-0.065567586070534,-0.0621782887363481,-0.05894467115978,-0.0403543924373443,
-0.0220984153978596,-0.00442511140790438,0.),.UNSPECIFIED.);
#2696=B_SPLINE_CURVE_WITH_KNOTS('',3,(#37156,#37157,#37158,#37159,#37160,
#37161,#37162,#37163,#37164,#37165,#37166,#37167,#37168),.UNSPECIFIED.,
 .F.,.F.,(4,3,3,3,4),(-101.213804280572,-100.730920097777,-99.7335842552244,
-98.7362484126722,-98.3403213565322),.UNSPECIFIED.);
#2697=B_SPLINE_CURVE_WITH_KNOTS('',3,(#37171,#37172,#37173,#37174,#37175,
#37176,#37177,#37178,#37179),.UNSPECIFIED.,.F.,.F.,(4,1,1,1,1,1,4),(10.3757270560178,
11.30460783463,12.30261480526,13.3006217758901,14.2986287465202,15.2966357171503,
15.7079632679489),.UNSPECIFIED.);
#2698=B_SPLINE_CURVE_WITH_KNOTS('',3,(#37613,#37614,#37615,#37616,#37617,
#37618,#37619,#37620,#37621,#37622,#37623,#37624,#37625,#37626,#37627,#37628),
 .UNSPECIFIED.,.F.,.F.,(4,3,3,3,3,4),(95.3619706457233,95.8086691804886,
96.8066761511186,97.8046831217487,98.8026900923788,99.1486641472938),
 .UNSPECIFIED.);
#2699=B_SPLINE_CURVE_WITH_KNOTS('',3,(#37629,#37630,#37631,#37632,#37633,
#37634,#37635,#37636,#37637,#37638,#37639,#37640,#37641,#37642,#37643,#37644,
#37645,#37646,#37647,#37648,#37649,#37650,#37651,#37652,#37653,#37654,#37655,
#37656,#37657,#37658,#37659,#37660,#37661,#37662,#37663,#37664,#37665,#37666,
#37667,#37668,#37669,#37670,#37671,#37672,#37673,#37674,#37675,#37676,#37677,
#37678,#37679,#37680,#37681,#37682,#37683,#37684,#37685,#37686,#37687,#37688,
#37689,#37690,#37691,#37692,#37693,#37694,#37695,#37696,#37697,#37698,#37699,
#37700,#37701,#37702,#37703,#37704,#37705,#37706,#37707,#37708,#37709,#37710,
#37711,#37712,#37713),.UNSPECIFIED.,.F.,.F.,(4,3,3,3,3,3,3,3,3,3,3,3,3,
3,3,3,3,3,3,3,3,3,3,3,3,3,3,3,4),(-0.366397579005845,-0.355461226466819,
-0.337490969642209,-0.327214164040339,-0.321649482146298,-0.302840833811487,
-0.288386907394637,-0.281257238921911,-0.277593927902022,-0.258153123971634,
-0.238335729520815,-0.225554152759783,-0.218411056976172,-0.214856426708649,
-0.194426531587897,-0.187209422476688,-0.167504451243421,-0.156894426252658,
-0.149523127563347,-0.145921626399787,-0.125494957624892,-0.104619107174947,
-0.0835512936559854,-0.0752831225832569,-0.0721648689176682,-0.0505208253811386,
-0.028827309118007,-0.00759789023731293,0.),.UNSPECIFIED.);
#2700=B_SPLINE_CURVE_WITH_KNOTS('',3,(#37767,#37768,#37769,#37770,#37771,
#37772,#37773,#37774,#37775,#37776),.UNSPECIFIED.,.F.,.F.,(4,3,3,4),(-4.09293042013066,
-3.9493215972006,-2.96199119790045,-2.06863817490914),.UNSPECIFIED.);
#2701=B_SPLINE_CURVE_WITH_KNOTS('',3,(#37779,#37780,#37781,#37782,#37783,
#37784,#37785),.UNSPECIFIED.,.F.,.F.,(4,3,4),(0.,0.988566943725272,1.11730040836823),
 .UNSPECIFIED.);
#2702=B_SPLINE_CURVE_WITH_KNOTS('',3,(#37790,#37791,#37792,#37793,#37794,
#37795,#37796,#37797,#37798,#37799,#37800,#37801,#37802,#37803,#37804,#37805,
#37806,#37807,#37808,#37809,#37810,#37811),.UNSPECIFIED.,.F.,.F.,(4,3,3,
3,3,3,3,4),(-10.3761157273102,-9.87330399300149,-8.88597359370134,-7.89864319440119,
-6.91131279510104,-5.92398239580089,-4.93665199650074,-4.09293042013066),
 .UNSPECIFIED.);
#2703=B_SPLINE_CURVE_WITH_KNOTS('',3,(#37812,#37813,#37814,#37815,#37816,
#37817,#37818,#37819,#37820,#37821,#37822,#37823,#37824,#37825,#37826,#37827,
#37828,#37829,#37830,#37831,#37832,#37833),.UNSPECIFIED.,.F.,.F.,(4,3,3,
3,3,3,3,4),(1.11730040836823,1.97713388745054,2.9657008311758,3.95426777490106,
4.94283471862632,5.93140166235159,6.91996860607685,7.40048571554782),
 .UNSPECIFIED.);
#2704=B_SPLINE_CURVE_WITH_KNOTS('',3,(#37838,#37839,#37840,#37841,#37842,
#37843,#37844,#37845,#37846,#37847,#37848,#37849,#37850,#37851,#37852,#37853,
#37854,#37855,#37856,#37857,#37858,#37859),.UNSPECIFIED.,.F.,.F.,(4,3,3,
3,3,3,3,4),(-16.6593010344898,-15.7972863888024,-14.8099559895022,-13.8226255902021,
-12.8352951909019,-11.8479647916018,-10.8606343923016,-10.3761157273102),
 .UNSPECIFIED.);
#2705=B_SPLINE_CURVE_WITH_KNOTS('',3,(#37860,#37861,#37862,#37863,#37864,
#37865,#37866,#37867,#37868,#37869,#37870,#37871,#37872,#37873,#37874,#37875,
#37876,#37877,#37878,#37879,#37880,#37881),.UNSPECIFIED.,.F.,.F.,(4,3,3,
3,3,3,3,4),(7.40048571554782,7.90853554980211,8.89710249352738,9.88566943725264,
10.8742363809779,11.8628033247032,12.8513702684284,13.6836710227274),
 .UNSPECIFIED.);
#2706=B_SPLINE_CURVE_WITH_KNOTS('',3,(#37886,#37887,#37888,#37889,#37890,
#37891,#37892,#37893,#37894,#37895,#37896,#37897,#37898,#37899,#37900,#37901,
#37902,#37903,#37904,#37905,#37906,#37907,#37908,#37909,#37910),
 .UNSPECIFIED.,.F.,.F.,(4,3,3,3,3,3,3,3,4),(-22.9424863416694,-22.7085991839034,
-21.7212687846033,-20.7339383853031,-19.746607986003,-18.7592775867028,
-17.7719471874027,-16.7846167881025,-16.6593010344898),.UNSPECIFIED.);
#2707=B_SPLINE_CURVE_WITH_KNOTS('',3,(#37911,#37912,#37913,#37914,#37915,
#37916,#37917,#37918,#37919,#37920,#37921,#37922,#37923,#37924,#37925,#37926,
#37927,#37928,#37929,#37930,#37931,#37932,#37933,#37934,#37935),
 .UNSPECIFIED.,.F.,.F.,(4,3,3,3,3,3,3,3,4),(13.6836710227274,13.8399372121537,
14.828504155879,15.8170710996042,16.8056380433295,17.7942049870548,18.78277193078,
19.7713388745053,19.966856329907),.UNSPECIFIED.);
#2708=B_SPLINE_CURVE_WITH_KNOTS('',3,(#37940,#37941,#37942,#37943,#37944,
#37945,#37946,#37947,#37948,#37949,#37950,#37951,#37952,#37953,#37954,#37955,
#37956,#37957,#37958,#37959,#37960,#37961),.UNSPECIFIED.,.F.,.F.,(4,3,3,
3,3,3,3,4),(-29.225671648849,-28.6325815797043,-27.6452511804042,-26.657920781104,
-25.6705903818039,-24.6832599825037,-23.6959295832036,-22.9424863416694),
 .UNSPECIFIED.);
#2709=B_SPLINE_CURVE_WITH_KNOTS('',3,(#37962,#37963,#37964,#37965,#37966,
#37967,#37968,#37969,#37970,#37971,#37972,#37973,#37974,#37975,#37976,#37977,
#37978,#37979,#37980,#37981,#37982,#37983),.UNSPECIFIED.,.F.,.F.,(4,3,3,
3,3,3,3,4),(19.966856329907,20.7599058182306,21.7484727619558,22.7370397056811,
23.7256066494064,24.7141735931316,25.7027405368569,26.2500416370866),
 .UNSPECIFIED.);
#2710=B_SPLINE_CURVE_WITH_KNOTS('',3,(#37988,#37989,#37990,#37991,#37992,
#37993,#37994,#37995,#37996,#37997,#37998,#37999,#38000,#38001,#38002,#38003,
#38004,#38005,#38006,#38007,#38008,#38009),.UNSPECIFIED.,.F.,.F.,(4,3,3,
3,3,3,3,4),(-35.5088569560286,-34.5565639755052,-33.5692335762051,-32.5819031769049,
-31.5945727776048,-30.6072423783046,-29.6199119790045,-29.225671648849),
 .UNSPECIFIED.);
#2711=B_SPLINE_CURVE_WITH_KNOTS('',3,(#38010,#38011,#38012,#38013,#38014,
#38015,#38016,#38017,#38018,#38019,#38020,#38021,#38022,#38023,#38024,#38025,
#38026,#38027,#38028,#38029,#38030,#38031),.UNSPECIFIED.,.F.,.F.,(4,3,3,
3,3,3,3,4),(26.2500416370866,26.6913074805822,27.6798744243074,28.6684413680327,
29.6570083117579,30.6455752554832,31.6341421992085,32.5332269442662),
 .UNSPECIFIED.);
#2712=B_SPLINE_CURVE_WITH_KNOTS('',3,(#38036,#38037,#38038,#38039,#38040,
#38041,#38042,#38043,#38044,#38045,#38046,#38047,#38048,#38049,#38050,#38051,
#38052,#38053,#38054,#38055,#38056,#38057,#38058,#38059,#38060),
 .UNSPECIFIED.,.F.,.F.,(4,3,3,3,3,3,3,3,4),(-41.7920422632082,-41.4678767706063,
-40.4805463713061,-39.4932159720059,-38.5058855727058,-37.5185551734057,
-36.5312247741055,-35.5438943748054,-35.5088569560286),.UNSPECIFIED.);
#2713=B_SPLINE_CURVE_WITH_KNOTS('',3,(#38061,#38062,#38063,#38064,#38065,
#38066,#38067,#38068,#38069,#38070,#38071,#38072,#38073,#38074,#38075,#38076,
#38077,#38078,#38079,#38080,#38081,#38082,#38083,#38084,#38085),
 .UNSPECIFIED.,.F.,.F.,(4,3,3,3,3,3,3,3,4),(32.5332269442662,32.6227091429337,
33.611276086659,34.5998430303843,35.5884099741095,36.5769769178348,37.5655438615601,
38.5541108052853,38.8164122514458),.UNSPECIFIED.);
#2714=B_SPLINE_CURVE_WITH_KNOTS('',3,(#38090,#38091,#38092,#38093,#38094,
#38095,#38096,#38097,#38098,#38099,#38100,#38101,#38102,#38103,#38104,#38105,
#38106,#38107,#38108,#38109,#38110,#38111),.UNSPECIFIED.,.F.,.F.,(4,3,3,
3,3,3,3,4),(-48.0752275703878,-47.3918591664071,-46.404528767107,-45.4171983678069,
-44.4298679685067,-43.4425375692066,-42.4552071699064,-41.7920422632082),
 .UNSPECIFIED.);
#2715=B_SPLINE_CURVE_WITH_KNOTS('',3,(#38112,#38113,#38114,#38115,#38116,
#38117,#38118,#38119,#38120,#38121,#38122,#38123,#38124,#38125,#38126,#38127,
#38128,#38129,#38130,#38131,#38132,#38133),.UNSPECIFIED.,.F.,.F.,(4,3,3,
3,3,3,3,4),(38.8164122514458,39.5426777490106,40.5312446927359,41.5198116364611,
42.5083785801864,43.4969455239117,44.4855124676369,45.0995975586253),
 .UNSPECIFIED.);
#2716=B_SPLINE_CURVE_WITH_KNOTS('',3,(#38138,#38139,#38140,#38141,#38142,
#38143,#38144,#38145,#38146,#38147,#38148,#38149,#38150,#38151,#38152,#38153,
#38154,#38155,#38156,#38157,#38158,#38159,#38160,#38161,#38162),
 .UNSPECIFIED.,.F.,.F.,(4,3,3,3,3,3,3,3,4),(-54.3584128775674,-54.3031719615082,
-53.315841562208,-52.3285111629079,-51.3411807636077,-50.3538503643076,
-49.3665199650074,-48.3791895657073,-48.0752275703878),.UNSPECIFIED.);
#2717=B_SPLINE_CURVE_WITH_KNOTS('',3,(#38163,#38164,#38165,#38166,#38167,
#38168,#38169,#38170,#38171,#38172,#38173,#38174,#38175,#38176,#38177,#38178,
#38179,#38180,#38181,#38182,#38183,#38184),.UNSPECIFIED.,.F.,.F.,(4,3,3,
3,3,3,3,4),(45.0995975586253,45.4740794113622,46.4626463550875,47.4512132988127,
48.439780242538,49.4283471862633,50.4169141299885,51.3827828658049),
 .UNSPECIFIED.);
#2718=B_SPLINE_CURVE_WITH_KNOTS('',3,(#38189,#38190,#38191,#38192,#38193,
#38194,#38195,#38196,#38197,#38198,#38199,#38200,#38201,#38202,#38203,#38204,
#38205,#38206,#38207,#38208,#38209,#38210),.UNSPECIFIED.,.F.,.F.,(4,3,3,
3,3,3,3,4),(-60.641598184747,-60.2271543573091,-59.2398239580089,-58.2524935587088,
-57.2651631594086,-56.2778327601085,-55.2905023608083,-54.3584128775674),
 .UNSPECIFIED.);
#2719=B_SPLINE_CURVE_WITH_KNOTS('',3,(#38211,#38212,#38213,#38214,#38215,
#38216,#38217,#38218,#38219,#38220,#38221,#38222,#38223,#38224,#38225,#38226,
#38227,#38228,#38229,#38230,#38231,#38232,#38233,#38234,#38235),
 .UNSPECIFIED.,.F.,.F.,(4,3,3,3,3,3,3,3,4),(51.3827828658049,51.4054810737138,
52.394048017439,53.3826149611643,54.3711819048896,55.3597488486148,56.3483157923401,
57.3368827360654,57.6659681729845),.UNSPECIFIED.);
#2720=B_SPLINE_CURVE_WITH_KNOTS('',3,(#38240,#38241,#38242,#38243,#38244,
#38245,#38246,#38247,#38248,#38249,#38250,#38251,#38252,#38253,#38254,#38255,
#38256,#38257,#38258,#38259,#38260,#38261),.UNSPECIFIED.,.F.,.F.,(4,3,3,
3,3,3,3,4),(-66.9247834919266,-66.15113675311,-65.1638063538098,-64.1764759545097,
-63.1891455552095,-62.2018151559094,-61.2144847566092,-60.641598184747),
 .UNSPECIFIED.);
#2721=B_SPLINE_CURVE_WITH_KNOTS('',3,(#38262,#38263,#38264,#38265,#38266,
#38267,#38268,#38269,#38270,#38271,#38272,#38273,#38274,#38275,#38276,#38277,
#38278,#38279,#38280,#38281,#38282,#38283),.UNSPECIFIED.,.F.,.F.,(4,3,3,
3,3,3,3,4),(57.6659681729845,58.3254496797906,59.3140166235159,60.3025835672412,
61.2911505109664,62.2797174546917,63.268284398417,63.9491534801641),
 .UNSPECIFIED.);
#2722=B_SPLINE_CURVE_WITH_KNOTS('',3,(#38289,#38290,#38291,#38292,#38293,
#38294,#38295,#38296,#38297,#38298),.UNSPECIFIED.,.F.,.F.,(4,1,1,1,1,1,
1,4),(78.5398163397448,78.7535000002284,79.7408303995285,80.7281607988287,
81.7154911981288,82.702821597429,83.6901519967291,84.6774823960293),
 .UNSPECIFIED.);
#2723=B_SPLINE_CURVE_WITH_KNOTS('',3,(#38301,#38302,#38303,#38304,#38305,
#38306,#38307,#38308),.UNSPECIFIED.,.F.,.F.,(4,1,1,1,1,4),(78.5398163397448,
79.4842975006201,80.4728644443454,81.4614313880706,82.4499983317959,83.4385652755212),
 .UNSPECIFIED.);
#2724=B_SPLINE_CURVE_WITH_KNOTS('',3,(#38313,#38314,#38315,#38316,#38317,
#38318,#38319,#38320,#38321,#38322),.UNSPECIFIED.,.F.,.F.,(4,1,1,1,1,1,
1,4),(72.2566310325653,72.8295176044275,73.8168480037276,74.8041784030278,
75.7915088023279,76.7788392016281,77.7661696009282,78.5398163397448),
 .UNSPECIFIED.);
#2725=B_SPLINE_CURVE_WITH_KNOTS('',3,(#38323,#38324,#38325,#38326,#38327,
#38328,#38329,#38330,#38331,#38332,#38333),.UNSPECIFIED.,.F.,.F.,(4,1,1,
1,1,1,1,1,4),(72.2566310325652,72.5643288945433,73.5528958382685,74.5414627819938,
75.530029725719,76.5185966694443,77.5071636131696,78.4957305568948,78.5398163397448),
 .UNSPECIFIED.);
#2726=B_SPLINE_CURVE_WITH_KNOTS('',3,(#38338,#38339,#38340,#38341,#38342,
#38343,#38344,#38345,#38346,#38347),.UNSPECIFIED.,.F.,.F.,(4,1,1,1,1,1,
1,4),(65.9734457253856,66.9055352086266,67.8928656079267,68.8801960072269,
69.867526406527,70.8548568058272,71.8421872051273,72.2566310325653),
 .UNSPECIFIED.);
#2727=B_SPLINE_CURVE_WITH_KNOTS('',3,(#38348,#38349,#38350,#38351,#38352,
#38353,#38354,#38355,#38356,#38357),.UNSPECIFIED.,.F.,.F.,(4,1,1,1,1,1,
1,4),(65.9734457253856,66.6329272321917,67.6214941759169,68.6100611196422,
69.5986280633675,70.5871950070927,71.575761950818,72.2566310325652),
 .UNSPECIFIED.);
#2728=B_SPLINE_CURVE_WITH_KNOTS('',3,(#38362,#38363,#38364,#38365,#38366,
#38367,#38368,#38369,#38370,#38371,#38372),.UNSPECIFIED.,.F.,.F.,(4,1,1,
1,1,1,1,1,4),(59.6902604182061,59.9942224135255,60.9815528128257,61.9688832121258,
62.956213611426,63.9435440107261,64.9308744100263,65.9182048093264,65.9734457253856),
 .UNSPECIFIED.);
#2729=B_SPLINE_CURVE_WITH_KNOTS('',3,(#38373,#38374,#38375,#38376,#38377,
#38378,#38379,#38380,#38381,#38382,#38383),.UNSPECIFIED.,.F.,.F.,(4,1,1,
1,1,1,1,1,4),(59.6902604182061,59.7129586261148,60.7015255698401,61.6900925135653,
62.6786594572906,63.6672264010159,64.6557933447411,65.6443602884664,65.9734457253856),
 .UNSPECIFIED.);
#2730=B_SPLINE_CURVE_WITH_KNOTS('',3,(#38388,#38389,#38390,#38391,#38392,
#38393,#38394,#38395,#38396,#38397),.UNSPECIFIED.,.F.,.F.,(4,1,1,1,1,1,
1,4),(53.4070751110265,54.0702400177247,55.0575704170248,56.0449008163249,
57.0322312156251,58.0195616149252,59.0068920142254,59.6902604182061),
 .UNSPECIFIED.);
#2731=B_SPLINE_CURVE_WITH_KNOTS('',3,(#38398,#38399,#38400,#38401,#38402,
#38403,#38404,#38405,#38406,#38407),.UNSPECIFIED.,.F.,.F.,(4,1,1,1,1,1,
1,4),(53.4070751110265,53.7815569637632,54.7701239074885,55.7586908512138,
56.747257794939,57.7358247386643,58.7243916823895,59.6902604182061),
 .UNSPECIFIED.);
#2732=B_SPLINE_CURVE_WITH_KNOTS('',3,(#38412,#38413,#38414,#38415,#38416,
#38417,#38418,#38419,#38420,#38421,#38422),.UNSPECIFIED.,.F.,.F.,(4,1,1,
1,1,1,1,1,4),(47.1238898038469,47.1589272226236,48.1462576219238,49.1335880212239,
50.1209184205241,51.1082488198242,52.0955792191244,53.0829096184245,53.4070751110265),
 .UNSPECIFIED.);
#2733=B_SPLINE_CURVE_WITH_KNOTS('',3,(#38423,#38424,#38425,#38426,#38427,
#38428,#38429,#38430,#38431,#38432),.UNSPECIFIED.,.F.,.F.,(4,1,1,1,1,1,
1,4),(47.1238898038469,47.8501553014116,48.8387222451369,49.8272891888622,
50.8158561325874,51.8044230763127,52.792990020038,53.4070751110265),
 .UNSPECIFIED.);
#2734=B_SPLINE_CURVE_WITH_KNOTS('',3,(#38437,#38438,#38439,#38440,#38441,
#38442,#38443,#38444,#38445,#38446),.UNSPECIFIED.,.F.,.F.,(4,1,1,1,1,1,
1,4),(40.8407044966673,41.2349448268227,42.2222752261229,43.209605625423,
44.1969360247232,45.1842664240233,46.1715968233235,47.1238898038469),
 .UNSPECIFIED.);
#2735=B_SPLINE_CURVE_WITH_KNOTS('',3,(#38447,#38448,#38449,#38450,#38451,
#38452,#38453,#38454,#38455,#38456,#38457),.UNSPECIFIED.,.F.,.F.,(4,1,1,
1,1,1,1,1,4),(40.8407044966673,40.9301866953348,41.91875363906,42.9073205827853,
43.8958875265106,44.8844544702358,45.8730214139611,46.8615883576864,47.1238898038469),
 .UNSPECIFIED.);
#2736=B_SPLINE_CURVE_WITH_KNOTS('',3,(#38462,#38463,#38464,#38465,#38466,
#38467,#38468,#38469,#38470,#38471),.UNSPECIFIED.,.F.,.F.,(4,1,1,1,1,1,
1,4),(34.5575191894877,35.3109624310218,36.298292830322,37.2856232296221,
38.2729536289223,39.2602840282224,40.2476144275226,40.8407044966673),
 .UNSPECIFIED.);
#2737=B_SPLINE_CURVE_WITH_KNOTS('',3,(#38472,#38473,#38474,#38475,#38476,
#38477,#38478,#38479,#38480,#38481),.UNSPECIFIED.,.F.,.F.,(4,1,1,1,1,1,
1,4),(34.5575191894877,34.9987850329832,35.9873519767085,36.9759189204337,
37.964485864159,38.9530528078842,39.9416197516095,40.8407044966673),
 .UNSPECIFIED.);
#2738=B_SPLINE_CURVE_WITH_KNOTS('',3,(#38486,#38487,#38488,#38489,#38490,
#38491,#38492,#38493,#38494,#38495,#38496),.UNSPECIFIED.,.F.,.F.,(4,1,1,
1,1,1,1,1,4),(28.2743338823081,28.3996496359208,29.3869800352209,30.3743104345211,
31.3616408338212,32.3489712331214,33.3363016324215,34.3236320317217,34.5575191894877),
 .UNSPECIFIED.);
#2739=B_SPLINE_CURVE_WITH_KNOTS('',3,(#38497,#38498,#38499,#38500,#38501,
#38502,#38503,#38504,#38505,#38506),.UNSPECIFIED.,.F.,.F.,(4,1,1,1,1,1,
1,4),(28.2743338823081,29.0673833706316,30.0559503143569,31.0445172580821,
32.0330842018074,33.0216511455327,34.0102180892579,34.5575191894877),
 .UNSPECIFIED.);
#2740=B_SPLINE_CURVE_WITH_KNOTS('',3,(#38511,#38512,#38513,#38514,#38515,
#38516,#38517,#38518,#38519,#38520),.UNSPECIFIED.,.F.,.F.,(4,1,1,1,1,1,
1,4),(21.9911485751285,22.4756672401199,23.46299763942,24.4503280387202,
25.4376584380203,26.4249888373205,27.4123192366206,28.2743338823081),
 .UNSPECIFIED.);
#2741=B_SPLINE_CURVE_WITH_KNOTS('',3,(#38521,#38522,#38523,#38524,#38525,
#38526,#38527,#38528,#38529,#38530,#38531),.UNSPECIFIED.,.F.,.F.,(4,1,1,
1,1,1,1,1,4),(21.9911485751285,22.1474147645547,23.13598170828,24.1245486520053,
25.1131155957305,26.1016825394558,27.0902494831811,28.0788164269063,28.2743338823081),
 .UNSPECIFIED.);
#2742=B_SPLINE_CURVE_WITH_KNOTS('',3,(#38536,#38537,#38538,#38539,#38540,
#38541,#38542,#38543,#38544,#38545),.UNSPECIFIED.,.F.,.F.,(4,1,1,1,1,1,
1,4),(15.7079632679489,16.551684844319,17.5390152436191,18.5263456429193,
19.5136760422194,20.5010064415196,21.4883368408197,21.9911485751285),
 .UNSPECIFIED.);
#2743=B_SPLINE_CURVE_WITH_KNOTS('',3,(#38546,#38547,#38548,#38549,#38550,
#38551,#38552,#38553,#38554,#38555),.UNSPECIFIED.,.F.,.F.,(4,1,1,1,1,1,
1,4),(15.7079632679489,16.2160131022032,17.2045800459284,18.1931469896537,
19.181713933379,20.1702808771042,21.1588478208295,21.9911485751285),
 .UNSPECIFIED.);
#2744=B_SPLINE_CURVE_WITH_KNOTS('',3,(#38558,#38559,#38560,#38561,#38562,
#38563,#38564,#38565,#38566,#38567,#38568,#38569,#38570,#38571,#38572,#38573,
#38574,#38575,#38576,#38577,#38578,#38579,#38580,#38581,#38582,#38583,#38584,
#38585,#38586,#38587,#38588,#38589,#38590,#38591,#38592,#38593,#38594,#38595,
#38596,#38597,#38598,#38599,#38600,#38601,#38602,#38603,#38604,#38605,#38606,
#38607,#38608,#38609,#38610,#38611,#38612,#38613,#38614,#38615,#38616,#38617,
#38618,#38619,#38620,#38621,#38622,#38623,#38624,#38625,#38626,#38627,#38628,
#38629,#38630,#38631,#38632,#38633,#38634,#38635,#38636,#38637,#38638,#38639,
#38640,#38641,#38642,#38643,#38644,#38645,#38646,#38647,#38648,#38649,#38650,
#38651,#38652,#38653,#38654,#38655,#38656,#38657,#38658,#38659,#38660,#38661,
#38662,#38663,#38664,#38665,#38666,#38667,#38668,#38669,#38670,#38671,#38672,
#38673,#38674,#38675,#38676,#38677,#38678,#38679,#38680,#38681,#38682,#38683,
#38684,#38685,#38686,#38687,#38688,#38689,#38690,#38691,#38692,#38693,#38694,
#38695,#38696,#38697,#38698,#38699,#38700,#38701,#38702,#38703,#38704,#38705,
#38706,#38707,#38708,#38709,#38710,#38711,#38712,#38713,#38714,#38715,#38716,
#38717,#38718,#38719,#38720,#38721,#38722,#38723,#38724,#38725,#38726,#38727,
#38728,#38729,#38730,#38731,#38732,#38733,#38734,#38735,#38736,#38737,#38738,
#38739,#38740,#38741,#38742,#38743,#38744,#38745,#38746,#38747,#38748,#38749,
#38750,#38751,#38752,#38753,#38754,#38755,#38756,#38757,#38758,#38759,#38760,
#38761,#38762,#38763,#38764,#38765,#38766,#38767,#38768,#38769,#38770,#38771,
#38772,#38773,#38774),.UNSPECIFIED.,.F.,.F.,(4,3,3,3,3,3,3,3,3,3,3,3,3,
3,3,3,3,3,3,3,3,3,3,3,3,3,3,3,3,3,3,3,3,3,3,3,3,3,3,3,3,3,3,3,3,3,3,3,3,
3,3,3,3,3,3,3,3,3,3,3,3,3,3,3,3,3,3,3,3,3,3,3,4),(-1.51155304937228,-1.48679174718013,
-1.46137597198077,-1.44942691521821,-1.44205848651244,-1.43724119559823,
-1.41130764113729,-1.38514768961224,-1.36936593028954,-1.36512230166791,
-1.33867581137855,-1.31235917608035,-1.29127511993008,-1.28073309185494,
-1.2739086628828,-1.27019106377981,-1.24488979836553,-1.21884130205047,
-1.19384888620637,-1.18291470427457,-1.17641188206357,-1.17130697868968,
-1.14451640582175,-1.11742561305122,-1.09279470361283,-1.08177565945417,
-1.07670730294613,-1.07245364414871,-1.0452101587782,-1.01890197529764,
-0.992076665792053,-0.977095538498891,-0.971310437727824,-0.944262984582137,
-0.91671696123902,-0.889051349044572,-0.8786107219546,-0.873404326505122,
-0.869185758667877,-0.841205731090746,-0.813331817877821,-0.785648584359967,
-0.771436006282574,-0.765308450445371,-0.757965350842113,-0.731019445974318,
-0.703340715547858,-0.676331238706378,-0.668063308133434,-0.663247880961674,
-0.658967945513649,-0.630690110839631,-0.602089962339152,-0.573383696958367,
-0.562618847440572,-0.556352694911719,-0.55203012393032,-0.523164492059728,
-0.494713544949419,-0.487264900816012,-0.45884309987075,-0.449622389577847,
-0.445165938771905,-0.416742684601646,-0.387755299334011,-0.358563756837841,
-0.34211828207705,-0.337697582134308,-0.308241853281341,-0.278784672736061,
-0.25000255453776,-0.226999958751515,-0.219677966288006),.UNSPECIFIED.);
#2745=B_SPLINE_CURVE_WITH_KNOTS('',3,(#38776,#38777,#38778,#38779,#38780,
#38781,#38782,#38783,#38784,#38785,#38786,#38787,#38788,#38789,#38790,#38791,
#38792,#38793,#38794,#38795,#38796,#38797,#38798,#38799,#38800,#38801,#38802,
#38803,#38804,#38805,#38806,#38807,#38808,#38809,#38810,#38811,#38812,#38813,
#38814,#38815,#38816,#38817,#38818,#38819,#38820,#38821,#38822,#38823,#38824,
#38825,#38826,#38827,#38828,#38829,#38830,#38831,#38832,#38833,#38834,#38835,
#38836),.UNSPECIFIED.,.F.,.F.,(4,3,3,3,3,3,3,3,3,3,3,3,3,3,3,3,3,3,3,3,
4),(-0.410648750432938,-0.381294613665594,-0.352267124576947,-0.328792823836752,
-0.311187098281605,-0.306018425011984,-0.301691296836585,-0.274143229574461,
-0.258369921616165,-0.230117472373342,-0.201352788326674,-0.195525900786732,
-0.16833922287309,-0.141249160586392,-0.114615533759621,-0.100282139063474,
-0.0960342097686789,-0.0702554174629941,-0.0448546715641945,-0.0201984500449382,
0.),.UNSPECIFIED.);
#2746=B_SPLINE_CURVE_WITH_KNOTS('',3,(#38839,#38840,#38841,#38842,#38843,
#38844,#38845,#38846,#38847,#38848,#38849,#38850,#38851,#38852,#38853,#38854,
#38855,#38856,#38857,#38858,#38859,#38860,#38861,#38862,#38863,#38864,#38865,
#38866,#38867,#38868,#38869),.UNSPECIFIED.,.F.,.F.,(4,3,3,3,3,3,3,3,3,3,
4),(-0.219677966288006,-0.206985183547511,-0.178213580556878,-0.148819200354015,
-0.130216800309763,-0.118450459252591,-0.113866160083042,-0.0841488051349767,
-0.0540951018364117,-0.0242019686830237,0.),.UNSPECIFIED.);
#2747=B_SPLINE_CURVE_WITH_KNOTS('',3,(#39182,#39183,#39184,#39185,#39186,
#39187,#39188,#39189),.UNSPECIFIED.,.F.,.F.,(4,1,1,1,1,4),(11.6150328478182,
12.6023632471184,13.5896936464185,14.5770240457187,15.5643544450188,15.7079632679489),
 .UNSPECIFIED.);
#2748=B_SPLINE_CURVE_WITH_KNOTS('',3,(#39190,#39191,#39192,#39193,#39194,
#39195,#39196,#39197,#39198,#39199,#39200,#39201,#39202,#39203,#39204,#39205,
#39206,#39207,#39208,#39209,#39210,#39211,#39212,#39213,#39214,#39215,#39216,
#39217,#39218,#39219,#39220,#39221,#39222,#39223,#39224,#39225,#39226,#39227,
#39228,#39229,#39230,#39231,#39232,#39233,#39234,#39235,#39236,#39237,#39238,
#39239,#39240,#39241,#39242,#39243,#39244,#39245,#39246,#39247,#39248,#39249,
#39250,#39251,#39252,#39253,#39254,#39255,#39256,#39257,#39258,#39259,#39260,
#39261,#39262,#39263,#39264,#39265,#39266,#39267,#39268,#39269,#39270,#39271,
#39272,#39273,#39274,#39275,#39276,#39277),.UNSPECIFIED.,.F.,.F.,(4,3,3,
3,3,3,3,3,3,3,3,3,3,3,3,3,3,3,3,3,3,3,3,3,3,3,3,3,3,4),(-0.55274537837504,
-0.525174630400016,-0.495740003900857,-0.479498227927527,-0.472105972866577,
-0.443064611280178,-0.418881458903182,-0.408301329738247,-0.401969450637142,
-0.397429868442983,-0.369124488132221,-0.341064938672273,-0.313899750226951,
-0.29772704364586,-0.291366968188088,-0.264559598151202,-0.249599392264211,
-0.222215347947115,-0.194438429453726,-0.189292991414398,-0.162670593649827,
-0.136062352557756,-0.109859916217256,-0.101879142728474,-0.0950850259724172,
-0.09115324392662,-0.0655931049079899,-0.0404250325776628,-0.0160423336449029,
0.),.UNSPECIFIED.);
#2749=B_SPLINE_CURVE_WITH_KNOTS('',3,(#39278,#39279,#39280,#39281,#39282,
#39283,#39284,#39285,#39286,#39287,#39288,#39289,#39290,#39291,#39292,#39293,
#39294,#39295,#39296),.UNSPECIFIED.,.F.,.F.,(4,3,3,3,3,3,4),(-71.548101301701,
-71.0877887496107,-70.1004583503106,-69.1131279510104,-68.1257975517103,
-67.1384671524101,-66.9247834919266),.UNSPECIFIED.);
#2750=B_SPLINE_CURVE_WITH_KNOTS('',3,(#39299,#39300,#39301,#39302,#39303,
#39304,#39305,#39306,#39307),.UNSPECIFIED.,.F.,.F.,(4,1,1,1,1,1,4),(10.3761157273102,
11.2731783835768,12.2617453273021,13.2503122710274,14.2388792147526,15.2274461584779,
15.7079632679489),.UNSPECIFIED.);
#2751=B_SPLINE_CURVE_WITH_KNOTS('',3,(#39625,#39626,#39627,#39628,#39629,
#39630,#39631,#39632,#39633,#39634,#39635,#39636,#39637,#39638,#39639,#39640,
#39641,#39642,#39643,#39644,#39645,#39646),.UNSPECIFIED.,.F.,.F.,(4,3,3,
3,3,3,3,4),(63.9491534801641,64.2568513421422,65.2454182858675,66.2339852295928,
67.222552173318,68.2111191170433,69.1996860607685,69.4794631267919),
 .UNSPECIFIED.);
#2752=B_SPLINE_CURVE_WITH_KNOTS('',3,(#39647,#39648,#39649,#39650,#39651,
#39652,#39653,#39654,#39655,#39656,#39657,#39658,#39659,#39660,#39661,#39662,
#39663,#39664,#39665,#39666,#39667,#39668,#39669,#39670,#39671,#39672,#39673,
#39674,#39675,#39676,#39677,#39678,#39679,#39680,#39681,#39682,#39683,#39684,
#39685,#39686,#39687,#39688,#39689,#39690,#39691,#39692,#39693,#39694,#39695,
#39696,#39697,#39698,#39699,#39700,#39701,#39702,#39703,#39704,#39705,#39706,
#39707,#39708,#39709,#39710,#39711,#39712,#39713,#39714,#39715,#39716,#39717,
#39718,#39719,#39720,#39721,#39722,#39723,#39724,#39725,#39726,#39727,#39728,
#39729,#39730,#39731,#39732,#39733,#39734),.UNSPECIFIED.,.F.,.F.,(4,3,3,
3,3,3,3,3,3,3,3,3,3,3,3,3,3,3,3,3,3,3,3,3,3,3,3,3,3,4),(-0.555272788399385,
-0.533197712400843,-0.50841200558917,-0.492097097422296,-0.487698425831477,
-0.461722637175749,-0.438993822101987,-0.427671428401512,-0.42202191869945,
-0.395458071621424,-0.368431943977533,-0.346296987129563,-0.329695769493585,
-0.32517826205158,-0.321068892319616,-0.293156561268766,-0.279892116585652,
-0.25291117159626,-0.225403496298925,-0.221057334466692,-0.216708298034074,
-0.188764735094145,-0.160284152968102,-0.131561788206246,-0.114355289595352,
-0.109564750157472,-0.0800994390258527,-0.050557237845911,-0.0215776241374192,
0.),.UNSPECIFIED.);
#2753=B_SPLINE_CURVE_WITH_KNOTS('',3,(#39788,#39789,#39790,#39791,#39792,
#39793,#39794,#39795,#39796,#39797,#39798,#39799,#39800,#39801,#39802,#39803),
 .UNSPECIFIED.,.F.,.F.,(4,3,3,3,3,4),(-4.09323272002468,-3.98127355678459,
-3.48361436218651,-2.98595516758844,-2.48829597299037,-2.07135887395548),
 .UNSPECIFIED.);
#2754=B_SPLINE_CURVE_WITH_KNOTS('',3,(#39806,#39807,#39808,#39809,#39810,
#39811,#39812,#39813,#39814,#39815),.UNSPECIFIED.,.F.,.F.,(4,3,3,4),(0.,
0.497659194598067,0.995318389196143,1.11971880752056),.UNSPECIFIED.);
#2755=B_SPLINE_CURVE_WITH_KNOTS('',3,(#39820,#39821,#39822,#39823,#39824,
#39825,#39826,#39827,#39828,#39829,#39830,#39831,#39832,#39833,#39834,#39835,
#39836,#39837,#39838,#39839,#39840,#39841,#39842,#39843,#39844,#39845,#39846,
#39847,#39848,#39849,#39850,#39851,#39852,#39853,#39854,#39855,#39856,#39857,
#39858,#39859),.UNSPECIFIED.,.F.,.F.,(4,3,3,3,3,3,3,3,3,3,3,3,3,4),(-10.3764180272043,
-9.95318389196147,-9.45552469736339,-8.95786550276532,-8.46020630816725,
-7.96254711356918,-7.4648879189711,-6.96722872437303,-6.46956952977495,
-5.97191033517688,-5.47425114057881,-4.97659194598073,-4.47893275138266,
-4.09323272002468),.UNSPECIFIED.);
#2756=B_SPLINE_CURVE_WITH_KNOTS('',3,(#39860,#39861,#39862,#39863,#39864,
#39865,#39866,#39867,#39868,#39869,#39870,#39871,#39872,#39873,#39874,#39875,
#39876,#39877,#39878,#39879,#39880,#39881,#39882,#39883,#39884,#39885,#39886,
#39887,#39888,#39889,#39890,#39891,#39892,#39893,#39894,#39895,#39896,#39897,
#39898,#39899),.UNSPECIFIED.,.F.,.F.,(4,3,3,3,3,3,3,3,3,3,3,3,3,4),(1.11971880752056,
1.49297758379422,1.99063677839229,2.48829597299036,2.98595516758844,3.48361436218651,
3.98127355678458,4.47893275138265,4.97659194598073,5.4742511405788,5.97191033517688,
6.46956952977495,6.96722872437302,7.40290411470015),.UNSPECIFIED.);
#2757=B_SPLINE_CURVE_WITH_KNOTS('',3,(#39904,#39905,#39906,#39907,#39908,
#39909,#39910,#39911,#39912,#39913,#39914,#39915,#39916,#39917,#39918,#39919,
#39920,#39921,#39922,#39923,#39924,#39925,#39926,#39927,#39928,#39929,#39930,
#39931,#39932,#39933,#39934,#39935,#39936,#39937,#39938,#39939,#39940,#39941,
#39942,#39943,#39944,#39945,#39946),.UNSPECIFIED.,.F.,.F.,(4,3,3,3,3,3,
3,3,3,3,3,3,3,3,4),(-16.6596033343839,-16.4227534217364,-15.9250942271383,
-15.4274350325403,-14.9297758379422,-14.4321166433441,-13.9344574487461,
-13.436798254148,-12.9391390595499,-12.4414798649518,-11.9438206703538,
-11.4461614757557,-10.9485022811576,-10.4508430865595,-10.3764180272043),
 .UNSPECIFIED.);
#2758=B_SPLINE_CURVE_WITH_KNOTS('',3,(#39947,#39948,#39949,#39950,#39951,
#39952,#39953,#39954,#39955,#39956,#39957,#39958,#39959,#39960,#39961,#39962,
#39963,#39964,#39965,#39966,#39967,#39968,#39969,#39970,#39971,#39972,#39973,
#39974,#39975,#39976,#39977,#39978,#39979,#39980,#39981,#39982,#39983,#39984,
#39985,#39986,#39987,#39988,#39989),.UNSPECIFIED.,.F.,.F.,(4,3,3,3,3,3,
3,3,3,3,3,3,3,3,4),(7.40290411470015,7.4648879189711,7.96254711356917,8.46020630816724,
8.95786550276532,9.45552469736339,9.95318389196146,10.4508430865595,10.9485022811576,
11.4461614757557,11.9438206703538,12.4414798649518,12.9391390595499,13.436798254148,
13.6860894218797),.UNSPECIFIED.);
#2759=B_SPLINE_CURVE_WITH_KNOTS('',3,(#39994,#39995,#39996,#39997,#39998,
#39999,#40000,#40001,#40002,#40003,#40004,#40005,#40006,#40007,#40008,#40009,
#40010,#40011,#40012,#40013,#40014,#40015,#40016,#40017,#40018,#40019,#40020,
#40021,#40022,#40023,#40024,#40025,#40026,#40027,#40028,#40029,#40030,#40031,
#40032,#40033,#40034,#40035,#40036),.UNSPECIFIED.,.F.,.F.,(4,3,3,3,3,3,
3,3,3,3,3,3,3,3,4),(-22.9427886415634,-22.8923229515114,-22.3946637569133,
-21.8970045623152,-21.3993453677171,-20.9016861731191,-20.404026978521,
-19.9063677839229,-19.4087085893249,-18.9110493947268,-18.4133902001287,
-17.9157310055306,-17.4180718109326,-16.9204126163345,-16.6596033343839),
 .UNSPECIFIED.);
#2760=B_SPLINE_CURVE_WITH_KNOTS('',3,(#40037,#40038,#40039,#40040,#40041,
#40042,#40043,#40044,#40045,#40046,#40047,#40048,#40049,#40050,#40051,#40052,
#40053,#40054,#40055,#40056,#40057,#40058,#40059,#40060,#40061,#40062,#40063,
#40064,#40065,#40066,#40067,#40068,#40069,#40070,#40071,#40072,#40073,#40074,
#40075,#40076,#40077,#40078,#40079),.UNSPECIFIED.,.F.,.F.,(4,3,3,3,3,3,
3,3,3,3,3,3,3,3,4),(13.6860894218797,13.934457448746,14.4321166433441,14.9297758379422,
15.4274350325403,15.9250942271383,16.4227534217364,16.9204126163345,17.4180718109326,
17.9157310055306,18.4133902001287,18.9110493947268,19.4087085893249,19.9063677839229,
19.9692747290593),.UNSPECIFIED.);
#2761=B_SPLINE_CURVE_WITH_KNOTS('',3,(#40084,#40085,#40086,#40087,#40088,
#40089,#40090,#40091,#40092,#40093,#40094,#40095,#40096,#40097,#40098,#40099,
#40100,#40101,#40102,#40103,#40104,#40105,#40106,#40107,#40108,#40109,#40110,
#40111,#40112,#40113,#40114,#40115,#40116,#40117,#40118,#40119,#40120,#40121,
#40122,#40123),.UNSPECIFIED.,.F.,.F.,(4,3,3,3,3,3,3,3,3,3,3,3,3,4),(-29.225973948743,
-28.8642332866883,-28.3665740920902,-27.8689148974921,-27.371255702894,
-26.873596508296,-26.3759373136979,-25.8782781190998,-25.3806189245017,
-24.8829597299037,-24.3853005353056,-23.8876413407075,-23.3899821461094,
-22.9427886415634),.UNSPECIFIED.);
#2762=B_SPLINE_CURVE_WITH_KNOTS('',3,(#40124,#40125,#40126,#40127,#40128,
#40129,#40130,#40131,#40132,#40133,#40134,#40135,#40136,#40137,#40138,#40139,
#40140,#40141,#40142,#40143,#40144,#40145,#40146,#40147,#40148,#40149,#40150,
#40151,#40152,#40153,#40154,#40155,#40156,#40157,#40158,#40159,#40160,#40161,
#40162,#40163),.UNSPECIFIED.,.F.,.F.,(4,3,3,3,3,3,3,3,3,3,3,3,3,4),(19.9692747290593,
20.404026978521,20.9016861731191,21.3993453677172,21.8970045623152,22.3946637569133,
22.8923229515114,23.3899821461095,23.8876413407075,24.3853005353056,24.8829597299037,
25.3806189245017,25.8782781190998,26.2524600362389),.UNSPECIFIED.);
#2763=B_SPLINE_CURVE_WITH_KNOTS('',3,(#40168,#40169,#40170,#40171,#40172,
#40173,#40174,#40175,#40176,#40177,#40178,#40179,#40180,#40181,#40182,#40183,
#40184,#40185,#40186,#40187,#40188,#40189,#40190,#40191,#40192,#40193,#40194,
#40195,#40196,#40197,#40198,#40199,#40200,#40201,#40202,#40203,#40204,#40205,
#40206,#40207,#40208,#40209,#40210),.UNSPECIFIED.,.F.,.F.,(4,3,3,3,3,3,
3,3,3,3,3,3,3,3,4),(-35.5091592559226,-35.3338028164632,-34.8361436218651,
-34.3384844272671,-33.840825232669,-33.3431660380709,-32.8455068434729,
-32.3478476488748,-31.8501884542767,-31.3525292596786,-30.8548700650806,
-30.3572108704825,-29.8595516758844,-29.3618924812863,-29.225973948743),
 .UNSPECIFIED.);
#2764=B_SPLINE_CURVE_WITH_KNOTS('',3,(#40211,#40212,#40213,#40214,#40215,
#40216,#40217,#40218,#40219,#40220,#40221,#40222,#40223,#40224,#40225,#40226,
#40227,#40228,#40229,#40230,#40231,#40232,#40233,#40234,#40235,#40236,#40237,
#40238,#40239,#40240,#40241,#40242,#40243,#40244,#40245,#40246,#40247,#40248,
#40249,#40250,#40251,#40252,#40253),.UNSPECIFIED.,.F.,.F.,(4,3,3,3,3,3,
3,3,3,3,3,3,3,3,4),(26.2524600362389,26.3759373136979,26.873596508296,27.371255702894,
27.8689148974921,28.3665740920902,28.8642332866883,29.3618924812863,29.8595516758844,
30.3572108704825,30.8548700650806,31.3525292596786,31.8501884542767,32.3478476488748,
32.5356453434185),.UNSPECIFIED.);
#2765=B_SPLINE_CURVE_WITH_KNOTS('',3,(#40258,#40259,#40260,#40261,#40262,
#40263,#40264,#40265,#40266,#40267,#40268,#40269,#40270,#40271,#40272,#40273,
#40274,#40275,#40276,#40277,#40278,#40279,#40280,#40281,#40282,#40283,#40284,
#40285,#40286,#40287,#40288,#40289,#40290,#40291,#40292,#40293,#40294,#40295,
#40296,#40297),.UNSPECIFIED.,.F.,.F.,(4,3,3,3,3,3,3,3,3,3,3,3,3,4),(-41.7923445631022,
-41.3057131516401,-40.808053957042,-40.3103947624439,-39.8127355678459,
-39.3150763732478,-38.8174171786497,-38.3197579840517,-37.8220987894536,
-37.3244395948555,-36.8267804002574,-36.3291212056594,-35.8314620110613,
-35.5091592559226),.UNSPECIFIED.);
#2766=B_SPLINE_CURVE_WITH_KNOTS('',3,(#40298,#40299,#40300,#40301,#40302,
#40303,#40304,#40305,#40306,#40307,#40308,#40309,#40310,#40311,#40312,#40313,
#40314,#40315,#40316,#40317,#40318,#40319,#40320,#40321,#40322,#40323,#40324,
#40325,#40326,#40327,#40328,#40329,#40330,#40331,#40332,#40333,#40334,#40335,
#40336,#40337,#40338,#40339,#40340),.UNSPECIFIED.,.F.,.F.,(4,3,3,3,3,3,
3,3,3,3,3,3,3,3,4),(32.5356453434185,32.8455068434728,33.3431660380709,
33.840825232669,34.3384844272671,34.8361436218651,35.3338028164632,35.8314620110613,
36.3291212056594,36.8267804002574,37.3244395948555,37.8220987894536,38.3197579840516,
38.8174171786497,38.8188306505981),.UNSPECIFIED.);
#2767=B_SPLINE_CURVE_WITH_KNOTS('',3,(#40345,#40346,#40347,#40348,#40349,
#40350,#40351,#40352,#40353,#40354,#40355,#40356,#40357,#40358,#40359,#40360,
#40361,#40362,#40363,#40364,#40365,#40366,#40367,#40368,#40369,#40370,#40371,
#40372,#40373,#40374,#40375,#40376,#40377,#40378,#40379,#40380,#40381,#40382,
#40383,#40384,#40385,#40386,#40387),.UNSPECIFIED.,.F.,.F.,(4,3,3,3,3,3,
3,3,3,3,3,3,3,3,4),(-48.0755298702818,-47.7752826814151,-47.277623486817,
-46.7799642922189,-46.2823050976208,-45.7846459030228,-45.2869867084247,
-44.7893275138266,-44.2916683192285,-43.7940091246305,-43.2963499300324,
-42.7986907354343,-42.3010315408362,-41.8033723462382,-41.7923445631022),
 .UNSPECIFIED.);
#2768=B_SPLINE_CURVE_WITH_KNOTS('',3,(#40388,#40389,#40390,#40391,#40392,
#40393,#40394,#40395,#40396,#40397,#40398,#40399,#40400,#40401,#40402,#40403,
#40404,#40405,#40406,#40407,#40408,#40409,#40410,#40411,#40412,#40413,#40414,
#40415,#40416,#40417,#40418,#40419,#40420,#40421,#40422,#40423,#40424,#40425,
#40426,#40427),.UNSPECIFIED.,.F.,.F.,(4,3,3,3,3,3,3,3,3,3,3,3,3,4),(38.8188306505981,
39.3150763732478,39.8127355678459,40.3103947624439,40.808053957042,41.3057131516401,
41.8033723462382,42.3010315408362,42.7986907354343,43.2963499300324,43.7940091246304,
44.2916683192285,44.7893275138266,45.1020159577777),.UNSPECIFIED.);
#2769=B_SPLINE_CURVE_WITH_KNOTS('',3,(#40432,#40433,#40434,#40435,#40436,
#40437,#40438,#40439,#40440,#40441,#40442,#40443,#40444,#40445,#40446,#40447,
#40448,#40449,#40450,#40451,#40452,#40453,#40454,#40455,#40456,#40457,#40458,
#40459,#40460,#40461,#40462,#40463,#40464,#40465,#40466,#40467,#40468,#40469,
#40470,#40471,#40472,#40473,#40474),.UNSPECIFIED.,.F.,.F.,(4,3,3,3,3,3,
3,3,3,3,3,3,3,3,4),(-54.3587151774614,-54.24485221119,-53.7471930165919,
-53.2495338219939,-52.7518746273958,-52.2542154327977,-51.7565562381996,
-51.2588970436016,-50.7612378490035,-50.2635786544054,-49.7659194598073,
-49.2682602652093,-48.7706010706112,-48.2729418760131,-48.0755298702818),
 .UNSPECIFIED.);
#2770=B_SPLINE_CURVE_WITH_KNOTS('',3,(#40475,#40476,#40477,#40478,#40479,
#40480,#40481,#40482,#40483,#40484,#40485,#40486,#40487,#40488,#40489,#40490,
#40491,#40492,#40493,#40494,#40495,#40496,#40497,#40498,#40499,#40500,#40501,
#40502,#40503,#40504,#40505,#40506,#40507,#40508,#40509,#40510,#40511,#40512,
#40513,#40514,#40515,#40516,#40517),.UNSPECIFIED.,.F.,.F.,(4,3,3,3,3,3,
3,3,3,3,3,3,3,3,4),(45.1020159577777,45.2869867084247,45.7846459030227,
46.2823050976208,46.7799642922189,47.277623486817,47.775282681415,48.2729418760131,
48.7706010706112,49.2682602652093,49.7659194598073,50.2635786544054,50.7612378490035,
51.2588970436016,51.3852012649573),.UNSPECIFIED.);
#2771=B_SPLINE_CURVE_WITH_KNOTS('',3,(#40522,#40523,#40524,#40525,#40526,
#40527,#40528,#40529,#40530,#40531,#40532,#40533,#40534,#40535,#40536,#40537,
#40538,#40539,#40540,#40541,#40542,#40543,#40544,#40545,#40546,#40547,#40548,
#40549,#40550,#40551,#40552,#40553,#40554,#40555,#40556,#40557,#40558,#40559,
#40560,#40561),.UNSPECIFIED.,.F.,.F.,(4,3,3,3,3,3,3,3,3,3,3,3,3,4),(-60.641900484641,
-60.2167625463669,-59.7191033517688,-59.2214441571707,-58.7237849625727,
-58.2261257679746,-57.7284665733765,-57.2308073787784,-56.7331481841804,
-56.2354889895823,-55.7378297949842,-55.2401706003861,-54.7425114057881,
-54.3587151774614),.UNSPECIFIED.);
#2772=B_SPLINE_CURVE_WITH_KNOTS('',3,(#40562,#40563,#40564,#40565,#40566,
#40567,#40568,#40569,#40570,#40571,#40572,#40573,#40574,#40575,#40576,#40577,
#40578,#40579,#40580,#40581,#40582,#40583,#40584,#40585,#40586,#40587,#40588,
#40589,#40590,#40591,#40592,#40593,#40594,#40595,#40596,#40597,#40598,#40599,
#40600,#40601),.UNSPECIFIED.,.F.,.F.,(4,3,3,3,3,3,3,3,3,3,3,3,3,4),(51.3852012649573,
51.7565562381996,52.2542154327977,52.7518746273958,53.2495338219938,53.7471930165919,
54.24485221119,54.7425114057881,55.2401706003861,55.7378297949842,56.2354889895823,
56.7331481841804,57.2308073787784,57.6683865721369),.UNSPECIFIED.);
#2773=B_SPLINE_CURVE_WITH_KNOTS('',3,(#40607,#40608,#40609,#40610,#40611,
#40612,#40613,#40614,#40615,#40616,#40617,#40618),.UNSPECIFIED.,.F.,.F.,
(4,1,1,1,1,1,1,1,1,4),(65.9734457253856,66.3572419537123,66.8549011483104,
67.3525603429085,67.8502195375065,68.3478787321046,68.8455379267027,69.3431971213007,
69.8408563158988,70.2577934149337),.UNSPECIFIED.);
#2774=B_SPLINE_CURVE_WITH_KNOTS('',3,(#40621,#40622,#40623,#40624,#40625,
#40626,#40627,#40628,#40629,#40630),.UNSPECIFIED.,.F.,.F.,(4,1,1,1,1,1,
1,4),(65.9734457253856,66.0335257266252,66.5311849212233,67.0288441158214,
67.5265033104195,68.0241625050175,68.5218216996156,69.0194808942137),
 .UNSPECIFIED.);
#2775=B_SPLINE_CURVE_WITH_KNOTS('',3,(#40635,#40636,#40637,#40638,#40639,
#40640,#40641,#40642,#40643,#40644,#40645,#40646,#40647,#40648,#40649,#40650,
#40651),.UNSPECIFIED.,.F.,.F.,(4,1,1,1,1,1,1,1,1,1,1,1,1,1,4),(59.690260418206,
59.8876724239374,60.3853316185354,60.8829908131335,61.3806500077316,61.8783092023296,
62.3759683969277,62.8736275915258,63.3712867861239,63.8689459807219,64.36660517532,
64.8642643699181,65.3619235645162,65.8595827591142,65.9734457253856),
 .UNSPECIFIED.);
#2776=B_SPLINE_CURVE_WITH_KNOTS('',3,(#40652,#40653,#40654,#40655,#40656,
#40657,#40658,#40659,#40660,#40661,#40662,#40663,#40664,#40665,#40666,#40667),
 .UNSPECIFIED.,.F.,.F.,(4,1,1,1,1,1,1,1,1,1,1,1,1,4),(59.6902604182061,
60.0616153914484,60.5592745860464,61.0569337806445,61.5545929752426,62.0522521698407,
62.5499113644387,63.0475705590368,63.5452297536349,64.042888948233,64.540548142831,
65.0382073374291,65.5358665320272,65.9734457253856),.UNSPECIFIED.);
#2777=B_SPLINE_CURVE_WITH_KNOTS('',3,(#40672,#40673,#40674,#40675,#40676,
#40677,#40678,#40679,#40680,#40681,#40682,#40683,#40684,#40685,#40686,#40687,
#40688),.UNSPECIFIED.,.F.,.F.,(4,1,1,1,1,1,1,1,1,1,1,1,1,1,4),(53.4070751110265,
53.4181028941624,53.9157620887605,54.4134212833585,54.9110804779566,55.4087396725547,
55.9063988671528,56.4040580617508,56.9017172563489,57.399376450947,57.8970356455451,
58.3946948401431,58.8923540347412,59.3900132293393,59.690260418206),
 .UNSPECIFIED.);
#2778=B_SPLINE_CURVE_WITH_KNOTS('',3,(#40689,#40690,#40691,#40692,#40693,
#40694,#40695,#40696,#40697,#40698,#40699,#40700,#40701,#40702,#40703,#40704,
#40705),.UNSPECIFIED.,.F.,.F.,(4,1,1,1,1,1,1,1,1,1,1,1,1,1,4),(53.4070751110265,
53.5920458616734,54.0897050562715,54.5873642508696,55.0850234454676,55.5826826400657,
56.0803418346638,56.5780010292619,57.0756602238599,57.573319418458,58.0709786130561,
58.5686378076541,59.0662970022522,59.5639561968503,59.6902604182061),
 .UNSPECIFIED.);
#2779=B_SPLINE_CURVE_WITH_KNOTS('',3,(#40710,#40711,#40712,#40713,#40714,
#40715,#40716,#40717,#40718,#40719,#40720,#40721,#40722,#40723,#40724,#40725),
 .UNSPECIFIED.,.F.,.F.,(4,1,1,1,1,1,1,1,1,1,1,1,1,4),(47.1238898038469,
47.4461925589855,47.9438517535836,48.4415109481817,48.9391701427797,49.4368293373778,
49.9344885319759,50.432147726574,50.929806921172,51.4274661157701,51.9251253103682,
52.4227845049663,52.9204436995643,53.4070751110265),.UNSPECIFIED.);
#2780=B_SPLINE_CURVE_WITH_KNOTS('',3,(#40726,#40727,#40728,#40729,#40730,
#40731,#40732,#40733,#40734,#40735,#40736,#40737,#40738,#40739,#40740,#40741),
 .UNSPECIFIED.,.F.,.F.,(4,1,1,1,1,1,1,1,1,1,1,1,1,4),(47.1238898038469,
47.6201355264965,48.1177947210946,48.6154539156927,49.1131131102908,49.6107723048888,
50.1084314994869,50.606090694085,51.103749888683,51.6014090832811,52.0990682778792,
52.5967274724773,53.0943866670753,53.4070751110265),.UNSPECIFIED.);
#2781=B_SPLINE_CURVE_WITH_KNOTS('',3,(#40746,#40747,#40748,#40749,#40750,
#40751,#40752,#40753,#40754,#40755,#40756,#40757,#40758,#40759,#40760,#40761,
#40762),.UNSPECIFIED.,.F.,.F.,(4,1,1,1,1,1,1,1,1,1,1,1,1,1,4),(40.8407044966673,
40.9766230292106,41.4742822238086,41.9719414184067,42.4696006130048,42.9672598076029,
43.4649190022009,43.962578196799,44.4602373913971,44.9578965859952,45.4555557805932,
45.9532149751913,46.4508741697894,46.9485333643874,47.1238898038469),
 .UNSPECIFIED.);
#2782=B_SPLINE_CURVE_WITH_KNOTS('',3,(#40763,#40764,#40765,#40766,#40767,
#40768,#40769,#40770,#40771,#40772,#40773,#40774,#40775,#40776,#40777,#40778,
#40779),.UNSPECIFIED.,.F.,.F.,(4,1,1,1,1,1,1,1,1,1,1,1,1,1,4),(40.8407044966673,
41.1505659967216,41.6482251913197,42.1458843859177,42.6435435805158,43.1412027751139,
43.638861969712,44.13652116431,44.6341803589081,45.1318395535062,45.6294987481042,
46.1271579427023,46.6248171373004,47.1224763318985,47.1238898038469),
 .UNSPECIFIED.);
#2783=B_SPLINE_CURVE_WITH_KNOTS('',3,(#40784,#40785,#40786,#40787,#40788,
#40789,#40790,#40791,#40792,#40793,#40794,#40795,#40796,#40797,#40798,#40799),
 .UNSPECIFIED.,.F.,.F.,(4,1,1,1,1,1,1,1,1,1,1,1,1,4),(34.5575191894877,
35.0047126940337,35.5023718886318,36.0000310832298,36.4976902778279,36.995349472426,
37.4930086670241,37.9906678616221,38.4883270562202,38.9859862508183,39.4836454454163,
39.9813046400144,40.4789638346125,40.8407044966673),.UNSPECIFIED.);
#2784=B_SPLINE_CURVE_WITH_KNOTS('',3,(#40800,#40801,#40802,#40803,#40804,
#40805,#40806,#40807,#40808,#40809,#40810,#40811,#40812,#40813,#40814,#40815,
#40816),.UNSPECIFIED.,.F.,.F.,(4,1,1,1,1,1,1,1,1,1,1,1,1,1,4),(34.5575191894877,
34.6809964669466,35.1786556615447,35.6763148561428,36.1739740507409,36.6716332453389,
37.169292439937,37.6669516345351,38.1646108291331,38.6622700237312,39.1599292183293,
39.6575884129274,40.1552476075254,40.6529068021235,40.8407044966673),
 .UNSPECIFIED.);
#2785=B_SPLINE_CURVE_WITH_KNOTS('',3,(#40821,#40822,#40823,#40824,#40825,
#40826,#40827,#40828,#40829,#40830,#40831,#40832,#40833,#40834,#40835,#40836,
#40837),.UNSPECIFIED.,.F.,.F.,(4,1,1,1,1,1,1,1,1,1,1,1,1,1,4),(28.2743338823081,
28.5351431642587,29.0328023588568,29.5304615534549,30.0281207480529,30.525779942651,
31.0234391372491,31.5210983318472,32.0187575264452,32.5164167210433,33.0140759156414,
33.5117351102395,34.0093943048375,34.5070534994356,34.5575191894877),
 .UNSPECIFIED.);
#2786=B_SPLINE_CURVE_WITH_KNOTS('',3,(#40838,#40839,#40840,#40841,#40842,
#40843,#40844,#40845,#40846,#40847,#40848,#40849,#40850,#40851,#40852,#40853),
 .UNSPECIFIED.,.F.,.F.,(4,1,1,1,1,1,1,1,1,1,1,1,1,4),(28.2743338823081,
28.7090861317698,29.2067453263678,29.7044045209659,30.202063715564,30.699722910162,
31.1973821047601,31.6950412993582,32.1927004939563,32.6903596885543,33.1880188831524,
33.6856780777505,34.1833372723486,34.5575191894877),.UNSPECIFIED.);
#2787=B_SPLINE_CURVE_WITH_KNOTS('',3,(#40858,#40859,#40860,#40861,#40862,
#40863,#40864,#40865,#40866,#40867,#40868,#40869,#40870,#40871,#40872,#40873,
#40874),.UNSPECIFIED.,.F.,.F.,(4,1,1,1,1,1,1,1,1,1,1,1,1,1,4),(21.9911485751285,
22.0655736344838,22.5632328290818,23.0608920236799,23.558551218278,24.0562104128761,
24.5538696074741,25.0515288020722,25.5491879966703,26.0468471912684,26.5445063858664,
27.0421655804645,27.5398247750626,28.0374839696607,28.2743338823081),
 .UNSPECIFIED.);
#2788=B_SPLINE_CURVE_WITH_KNOTS('',3,(#40875,#40876,#40877,#40878,#40879,
#40880,#40881,#40882,#40883,#40884,#40885,#40886,#40887,#40888,#40889,#40890,
#40891),.UNSPECIFIED.,.F.,.F.,(4,1,1,1,1,1,1,1,1,1,1,1,1,1,4),(21.9911485751285,
22.2395166019948,22.7371757965929,23.2348349911909,23.732494185789,24.2301533803871,
24.7278125749852,25.2254717695832,25.7231309641813,26.2207901587794,26.7184493533775,
27.2161085479755,27.7137677425736,28.2114269371717,28.2743338823081),
 .UNSPECIFIED.);
#2789=B_SPLINE_CURVE_WITH_KNOTS('',3,(#40896,#40897,#40898,#40899,#40900,
#40901,#40902,#40903,#40904,#40905,#40906,#40907,#40908,#40909,#40910,#40911),
 .UNSPECIFIED.,.F.,.F.,(4,1,1,1,1,1,1,1,1,1,1,1,1,4),(15.7079632679489,
16.0936632993069,16.591322493905,17.088981688503,17.5866408831011,18.0843000776992,
18.5819592722973,19.0796184668953,19.5772776614934,20.0749368560915,20.5725960506896,
21.0702552452876,21.5679144398857,21.9911485751285),.UNSPECIFIED.);
#2790=B_SPLINE_CURVE_WITH_KNOTS('',3,(#40912,#40913,#40914,#40915,#40916,
#40917,#40918,#40919,#40920,#40921,#40922,#40923,#40924,#40925,#40926,#40927,
#40928),.UNSPECIFIED.,.F.,.F.,(4,1,1,1,1,1,1,1,1,1,1,1,1,1,4),(15.7079632679489,
15.7699470722198,16.2676062668179,16.765265461416,17.2629246560141,17.7605838506121,
18.2582430452102,18.7559022398083,19.2535614344064,19.7512206290044,20.2488798236025,
20.7465390182006,21.2441982127987,21.7418574073967,21.9911485751285),
 .UNSPECIFIED.);
#2791=B_SPLINE_CURVE_WITH_KNOTS('',3,(#41430,#41431,#41432,#41433,#41434,
#41435,#41436,#41437,#41438,#41439,#41440,#41441,#41442,#41443,#41444,#41445,
#41446,#41447,#41448,#41449,#41450,#41451,#41452,#41453,#41454,#41455,#41456,
#41457,#41458,#41459,#41460,#41461,#41462,#41463,#41464,#41465,#41466,#41467,
#41468,#41469,#41470,#41471,#41472,#41473,#41474,#41475,#41476,#41477,#41478,
#41479,#41480,#41481,#41482,#41483,#41484,#41485,#41486,#41487,#41488,#41489,
#41490,#41491,#41492,#41493,#41494,#41495,#41496,#41497,#41498,#41499,#41500,
#41501,#41502,#41503,#41504,#41505,#41506,#41507,#41508,#41509,#41510,#41511,
#41512,#41513,#41514,#41515,#41516,#41517,#41518,#41519,#41520,#41521,#41522,
#41523,#41524,#41525,#41526,#41527,#41528,#41529,#41530,#41531,#41532,#41533,
#41534,#41535,#41536,#41537,#41538,#41539,#41540,#41541,#41542,#41543,#41544,
#41545,#41546,#41547),.UNSPECIFIED.,.F.,.F.,(4,3,3,3,3,3,3,3,3,3,3,3,3,
3,3,3,3,3,3,3,3,3,3,3,3,3,3,3,3,3,3,3,3,3,3,3,3,3,3,4),(0.,0.0640389508670487,
0.126232635496461,0.188657039277152,0.250776918005212,0.301501483646333,
0.311103047329612,0.372484856250651,0.43360723014164,0.453675180569697,
0.515140939082644,0.576285345103759,0.594633063449029,0.605631449437402,
0.61301147768363,0.673473436401074,0.733894290152365,0.793562507830594,
0.833267193557858,0.879431537146101,0.893527612392673,0.900861755744641,
0.959992814090244,1.02064009613363,1.07986501715205,1.14122347970793,1.17190271098587,
1.1856790179708,1.19313842944556,1.2025819422638,1.26115034772533,1.31989387337031,
1.35006824439312,1.3643068112087,1.37388684239216,1.38132579651358,1.43936588678999,
1.49709102825393,1.55390796987554,1.56128884155279),.UNSPECIFIED.);
#2792=B_SPLINE_CURVE_WITH_KNOTS('',3,(#41548,#41549,#41550,#41551,#41552,
#41553,#41554,#41555,#41556,#41557),.UNSPECIFIED.,.F.,.F.,(4,3,3,4),(57.6683865721369,
57.7284665733765,58.2261257679746,58.6430628670095),.UNSPECIFIED.);
#2793=B_SPLINE_CURVE_WITH_KNOTS('',3,(#41559,#41560,#41561,#41562,#41563,
#41564,#41565,#41566,#41567,#41568,#41569,#41570,#41571,#41572,#41573,#41574,
#41575,#41576,#41577,#41578,#41579,#41580,#41581,#41582,#41583,#41584,#41585,
#41586,#41587,#41588,#41589,#41590,#41591,#41592,#41593,#41594,#41595,#41596,
#41597,#41598,#41599,#41600,#41601,#41602,#41603,#41604,#41605,#41606,#41607,
#41608,#41609,#41610,#41611,#41612,#41613,#41614,#41615,#41616,#41617,#41618,
#41619,#41620,#41621,#41622,#41623,#41624,#41625,#41626,#41627,#41628,#41629,
#41630,#41631,#41632,#41633,#41634,#41635,#41636,#41637,#41638,#41639,#41640,
#41641,#41642,#41643,#41644,#41645,#41646,#41647,#41648,#41649,#41650,#41651,
#41652,#41653,#41654,#41655,#41656,#41657,#41658,#41659,#41660,#41661,#41662,
#41663,#41664,#41665,#41666,#41667,#41668,#41669,#41670,#41671,#41672,#41673),
 .UNSPECIFIED.,.F.,.F.,(4,3,3,3,3,3,3,3,3,3,3,3,3,3,3,3,3,3,3,3,3,3,3,3,
3,3,3,3,3,3,3,3,3,3,3,3,3,3,4),(-1.5612888415528,-1.50381997927053,-1.44626607638451,
-1.40841603929727,-1.38397573253337,-1.37502188808332,-1.31651898058331,
-1.25777459806667,-1.2006201888766,-1.18830429954325,-1.18030734756907,
-1.14346577968654,-1.08500221787391,-1.0257955428698,-0.966253568289297,
-0.91777400672482,-0.906613929613625,-0.89902907381174,-0.838953330303881,
-0.778441026219316,-0.77233532203139,-0.712209997853756,-0.651759029464709,
-0.619175485541018,-0.60908817917268,-0.601432360210168,-0.540468743341305,
-0.479070773468726,-0.417730405453208,-0.391090678075187,-0.342204343315789,
-0.320816571858552,-0.310234380897366,-0.301157505671209,-0.239985909763509,
-0.177711909468721,-0.11529068844521,-0.0534506659119964,0.),
 .UNSPECIFIED.);
#2794=B_SPLINE_CURVE_WITH_KNOTS('',3,(#41674,#41675,#41676,#41677,#41678,
#41679,#41680,#41681,#41682,#41683,#41684,#41685,#41686,#41687),
 .UNSPECIFIED.,.F.,.F.,(4,1,1,1,1,1,1,1,1,1,1,4),(10.3764180272042,10.7933551262391,
11.2910143208372,11.7886735154353,12.2863327100333,12.7839919046314,13.2816510992295,
13.7793102938275,14.2769694884256,14.7746286830237,15.2722878776218,15.7079632679489),
 .UNSPECIFIED.);
#2795=B_SPLINE_CURVE_WITH_KNOTS('',3,(#41691,#41692,#41693,#41694,#41695,
#41696,#41697,#41698,#41699,#41700,#41701,#41702),.UNSPECIFIED.,.F.,.F.,
(4,1,1,1,1,1,1,1,1,4),(11.6147305479242,12.1123897425223,12.6100489371204,
13.1077081317185,13.6053673263165,14.1030265209146,14.6006857155127,15.0983449101107,
15.5960041047088,15.7079632679489),.UNSPECIFIED.);
#2796=B_SPLINE_CURVE_WITH_KNOTS('',3,(#42204,#42205,#42206,#42207,#42208,
#42209,#42210,#42211,#42212,#42213,#42214,#42215,#42216,#42217,#42218,#42219,
#42220,#42221,#42222,#42223,#42224,#42225,#42226,#42227,#42228,#42229,#42230,
#42231,#42232,#42233,#42234,#42235,#42236,#42237,#42238,#42239,#42240,#42241,
#42242,#42243,#42244,#42245,#42246,#42247,#42248,#42249,#42250,#42251,#42252,
#42253,#42254,#42255,#42256,#42257,#42258,#42259,#42260,#42261,#42262,#42263,
#42264,#42265,#42266,#42267,#42268,#42269,#42270,#42271,#42272,#42273,#42274,
#42275,#42276,#42277,#42278,#42279,#42280,#42281,#42282,#42283,#42284,#42285,
#42286,#42287,#42288,#42289,#42290,#42291,#42292,#42293,#42294,#42295,#42296,
#42297,#42298,#42299,#42300,#42301,#42302,#42303,#42304,#42305,#42306,#42307,
#42308,#42309,#42310,#42311,#42312,#42313,#42314,#42315,#42316,#42317,#42318,
#42319,#42320,#42321),.UNSPECIFIED.,.F.,.F.,(4,3,3,3,3,3,3,3,3,3,3,3,3,
3,3,3,3,3,3,3,3,3,3,3,3,3,3,3,3,3,3,3,3,3,3,3,3,3,3,4),(0.,0.0573839578688757,
0.114590484122352,0.172466904307786,0.230588407369637,0.277342780760038,
0.283471950450586,0.342148786594638,0.401253301161324,0.417605900931242,
0.476403667266598,0.535433861034147,0.552517961785708,0.561030348077734,
0.568192904833271,0.627729231249355,0.68770609069227,0.747626730537876,
0.787875082072579,0.835383058713792,0.846478499762998,0.853725938073134,
0.86163476712092,0.921384582649023,0.983023160787337,1.04403071219776,1.10598480370002,
1.13696184945115,1.14862783597345,1.15683895023771,1.16793889520228,1.22874774584585,
1.29023148370971,1.32364607620725,1.3501106960563,1.35906742929627,1.42129775631956,
1.48369851743659,1.54568460253334,1.55754822368998),.UNSPECIFIED.);
#2797=B_SPLINE_CURVE_WITH_KNOTS('',3,(#42322,#42323,#42324,#42325,#42326,
#42327,#42328,#42329,#42330,#42331,#42332,#42333,#42334,#42335,#42336,#42337,
#42338,#42339,#42340,#42341,#42342,#42343,#42344,#42345,#42346,#42347,#42348,
#42349,#42350,#42351,#42352,#42353,#42354,#42355,#42356,#42357,#42358,#42359,
#42360,#42361,#42362,#42363,#42364,#42365,#42366,#42367,#42368,#42369,#42370,
#42371,#42372,#42373,#42374,#42375,#42376,#42377,#42378,#42379,#42380,#42381,
#42382,#42383,#42384,#42385,#42386,#42387,#42388,#42389,#42390,#42391,#42392,
#42393,#42394,#42395,#42396,#42397,#42398,#42399,#42400,#42401,#42402,#42403,
#42404,#42405,#42406,#42407,#42408,#42409,#42410,#42411,#42412,#42413,#42414,
#42415,#42416,#42417,#42418,#42419,#42420,#42421,#42422,#42423,#42424,#42425,
#42426,#42427,#42428,#42429,#42430,#42431,#42432,#42433,#42434,#42435,#42436),
 .UNSPECIFIED.,.F.,.F.,(4,3,3,3,3,3,3,3,3,3,3,3,3,3,3,3,3,3,3,3,3,3,3,3,
3,3,3,3,3,3,3,3,3,3,3,3,3,3,4),(-1.55754822368999,-1.49369030775179,-1.4313235190698,
-1.39062308635,-1.36715669998756,-1.35596433121764,-1.34727309230324,-1.2855394700848,
-1.2240883864807,-1.16490422189603,-1.15492087119867,-1.14664991405737,
-1.10572005731137,-1.04502187930064,-0.984006782056958,-0.92320309422318,
-0.874174440126947,-0.855865305758246,-0.848822556599067,-0.787955517218659,
-0.72708847783825,-0.667031022725293,-0.607206878858597,-0.576110200997875,
-0.565145179110016,-0.558975853547965,-0.499936666610499,-0.44095175273352,
-0.382672386577637,-0.358433455972822,-0.313629273976219,-0.294027444352705,
-0.283755524046394,-0.27394190140763,-0.216143666927953,-0.158030747047698,
-0.100247716305122,-0.0435718312192328,0.),.UNSPECIFIED.);
#2798=B_SPLINE_CURVE_WITH_KNOTS('',3,(#42437,#42438,#42439,#42440),
 .UNSPECIFIED.,.F.,.F.,(4,4),(-60.714421740965,-60.641900484641),
 .UNSPECIFIED.);
#2799=LINE('',#13453,#3337);
#2800=LINE('',#13482,#3338);
#2801=LINE('',#13509,#3339);
#2802=LINE('',#13560,#3340);
#2803=LINE('',#13608,#3341);
#2804=LINE('',#13659,#3342);
#2805=LINE('',#13710,#3343);
#2806=LINE('',#13758,#3344);
#2807=LINE('',#13806,#3345);
#2808=LINE('',#13857,#3346);
#2809=LINE('',#13905,#3347);
#2810=LINE('',#13953,#3348);
#2811=LINE('',#14004,#3349);
#2812=LINE('',#14055,#3350);
#2813=LINE('',#14103,#3351);
#2814=LINE('',#14154,#3352);
#2815=LINE('',#14193,#3353);
#2816=LINE('',#14213,#3354);
#2817=LINE('',#14237,#3355);
#2818=LINE('',#14262,#3356);
#2819=LINE('',#14287,#3357);
#2820=LINE('',#14311,#3358);
#2821=LINE('',#14336,#3359);
#2822=LINE('',#14360,#3360);
#2823=LINE('',#14385,#3361);
#2824=LINE('',#14410,#3362);
#2825=LINE('',#14434,#3363);
#2826=LINE('',#14459,#3364);
#2827=LINE('',#14483,#3365);
#2828=LINE('',#14508,#3366);
#2829=LINE('',#14533,#3367);
#2830=LINE('',#14557,#3368);
#2831=LINE('',#14574,#3369);
#2832=LINE('',#14603,#3370);
#2833=LINE('',#14630,#3371);
#2834=LINE('',#14681,#3372);
#2835=LINE('',#14729,#3373);
#2836=LINE('',#14780,#3374);
#2837=LINE('',#14831,#3375);
#2838=LINE('',#14879,#3376);
#2839=LINE('',#14927,#3377);
#2840=LINE('',#14978,#3378);
#2841=LINE('',#15026,#3379);
#2842=LINE('',#15074,#3380);
#2843=LINE('',#15125,#3381);
#2844=LINE('',#15176,#3382);
#2845=LINE('',#15224,#3383);
#2846=LINE('',#15275,#3384);
#2847=LINE('',#15314,#3385);
#2848=LINE('',#15334,#3386);
#2849=LINE('',#15358,#3387);
#2850=LINE('',#15383,#3388);
#2851=LINE('',#15408,#3389);
#2852=LINE('',#15432,#3390);
#2853=LINE('',#15457,#3391);
#2854=LINE('',#15481,#3392);
#2855=LINE('',#15506,#3393);
#2856=LINE('',#15531,#3394);
#2857=LINE('',#15555,#3395);
#2858=LINE('',#15580,#3396);
#2859=LINE('',#15604,#3397);
#2860=LINE('',#15629,#3398);
#2861=LINE('',#15654,#3399);
#2862=LINE('',#15678,#3400);
#2863=LINE('',#15695,#3401);
#2864=LINE('',#15724,#3402);
#2865=LINE('',#15751,#3403);
#2866=LINE('',#15802,#3404);
#2867=LINE('',#15850,#3405);
#2868=LINE('',#15901,#3406);
#2869=LINE('',#15952,#3407);
#2870=LINE('',#16000,#3408);
#2871=LINE('',#16048,#3409);
#2872=LINE('',#16099,#3410);
#2873=LINE('',#16147,#3411);
#2874=LINE('',#16195,#3412);
#2875=LINE('',#16246,#3413);
#2876=LINE('',#16297,#3414);
#2877=LINE('',#16345,#3415);
#2878=LINE('',#16396,#3416);
#2879=LINE('',#16435,#3417);
#2880=LINE('',#16455,#3418);
#2881=LINE('',#16479,#3419);
#2882=LINE('',#16504,#3420);
#2883=LINE('',#16529,#3421);
#2884=LINE('',#16553,#3422);
#2885=LINE('',#16578,#3423);
#2886=LINE('',#16602,#3424);
#2887=LINE('',#16627,#3425);
#2888=LINE('',#16652,#3426);
#2889=LINE('',#16676,#3427);
#2890=LINE('',#16701,#3428);
#2891=LINE('',#16725,#3429);
#2892=LINE('',#16750,#3430);
#2893=LINE('',#16775,#3431);
#2894=LINE('',#16799,#3432);
#2895=LINE('',#16816,#3433);
#2896=LINE('',#16845,#3434);
#2897=LINE('',#16872,#3435);
#2898=LINE('',#16923,#3436);
#2899=LINE('',#16971,#3437);
#2900=LINE('',#17022,#3438);
#2901=LINE('',#17073,#3439);
#2902=LINE('',#17121,#3440);
#2903=LINE('',#17169,#3441);
#2904=LINE('',#17220,#3442);
#2905=LINE('',#17268,#3443);
#2906=LINE('',#17316,#3444);
#2907=LINE('',#17367,#3445);
#2908=LINE('',#17418,#3446);
#2909=LINE('',#17466,#3447);
#2910=LINE('',#17517,#3448);
#2911=LINE('',#17556,#3449);
#2912=LINE('',#17576,#3450);
#2913=LINE('',#17600,#3451);
#2914=LINE('',#17625,#3452);
#2915=LINE('',#17650,#3453);
#2916=LINE('',#17674,#3454);
#2917=LINE('',#17699,#3455);
#2918=LINE('',#17723,#3456);
#2919=LINE('',#17748,#3457);
#2920=LINE('',#17773,#3458);
#2921=LINE('',#17797,#3459);
#2922=LINE('',#17822,#3460);
#2923=LINE('',#17846,#3461);
#2924=LINE('',#17871,#3462);
#2925=LINE('',#17896,#3463);
#2926=LINE('',#17920,#3464);
#2927=LINE('',#17937,#3465);
#2928=LINE('',#17980,#3466);
#2929=LINE('',#18031,#3467);
#2930=LINE('',#18082,#3468);
#2931=LINE('',#18130,#3469);
#2932=LINE('',#18181,#3470);
#2933=LINE('',#18232,#3471);
#2934=LINE('',#18280,#3472);
#2935=LINE('',#18331,#3473);
#2936=LINE('',#18382,#3474);
#2937=LINE('',#18430,#3475);
#2938=LINE('',#18481,#3476);
#2939=LINE('',#18532,#3477);
#2940=LINE('',#18580,#3478);
#2941=LINE('',#18631,#3479);
#2942=LINE('',#18670,#3480);
#2943=LINE('',#18713,#3481);
#2944=LINE('',#18764,#3482);
#2945=LINE('',#18815,#3483);
#2946=LINE('',#18863,#3484);
#2947=LINE('',#18914,#3485);
#2948=LINE('',#18965,#3486);
#2949=LINE('',#19013,#3487);
#2950=LINE('',#19064,#3488);
#2951=LINE('',#19115,#3489);
#2952=LINE('',#19163,#3490);
#2953=LINE('',#19214,#3491);
#2954=LINE('',#19265,#3492);
#2955=LINE('',#19313,#3493);
#2956=LINE('',#19364,#3494);
#2957=LINE('',#19403,#3495);
#2958=LINE('',#19427,#3496);
#2959=LINE('',#19451,#3497);
#2960=LINE('',#19476,#3498);
#2961=LINE('',#19501,#3499);
#2962=LINE('',#19525,#3500);
#2963=LINE('',#19550,#3501);
#2964=LINE('',#19575,#3502);
#2965=LINE('',#19599,#3503);
#2966=LINE('',#19624,#3504);
#2967=LINE('',#19649,#3505);
#2968=LINE('',#19673,#3506);
#2969=LINE('',#19698,#3507);
#2970=LINE('',#19723,#3508);
#2971=LINE('',#19747,#3509);
#2972=LINE('',#19764,#3510);
#2973=LINE('',#19788,#3511);
#2974=LINE('',#19812,#3512);
#2975=LINE('',#19837,#3513);
#2976=LINE('',#19862,#3514);
#2977=LINE('',#19886,#3515);
#2978=LINE('',#19911,#3516);
#2979=LINE('',#19936,#3517);
#2980=LINE('',#19960,#3518);
#2981=LINE('',#19985,#3519);
#2982=LINE('',#20010,#3520);
#2983=LINE('',#20034,#3521);
#2984=LINE('',#20059,#3522);
#2985=LINE('',#20084,#3523);
#2986=LINE('',#20108,#3524);
#2987=LINE('',#20125,#3525);
#2988=LINE('',#20134,#3526);
#2989=LINE('',#20151,#3527);
#2990=LINE('',#20202,#3528);
#2991=LINE('',#20253,#3529);
#2992=LINE('',#20301,#3530);
#2993=LINE('',#20352,#3531);
#2994=LINE('',#20403,#3532);
#2995=LINE('',#20451,#3533);
#2996=LINE('',#20502,#3534);
#2997=LINE('',#20553,#3535);
#2998=LINE('',#20601,#3536);
#2999=LINE('',#20652,#3537);
#3000=LINE('',#20703,#3538);
#3001=LINE('',#20751,#3539);
#3002=LINE('',#20802,#3540);
#3003=LINE('',#20841,#3541);
#3004=LINE('',#20865,#3542);
#3005=LINE('',#20889,#3543);
#3006=LINE('',#20914,#3544);
#3007=LINE('',#20939,#3545);
#3008=LINE('',#20963,#3546);
#3009=LINE('',#20988,#3547);
#3010=LINE('',#21013,#3548);
#3011=LINE('',#21037,#3549);
#3012=LINE('',#21062,#3550);
#3013=LINE('',#21087,#3551);
#3014=LINE('',#21111,#3552);
#3015=LINE('',#21136,#3553);
#3016=LINE('',#21161,#3554);
#3017=LINE('',#21185,#3555);
#3018=LINE('',#21202,#3556);
#3019=LINE('',#21211,#3557);
#3020=LINE('',#21228,#3558);
#3021=LINE('',#21279,#3559);
#3022=LINE('',#21330,#3560);
#3023=LINE('',#21378,#3561);
#3024=LINE('',#21429,#3562);
#3025=LINE('',#21480,#3563);
#3026=LINE('',#21528,#3564);
#3027=LINE('',#21579,#3565);
#3028=LINE('',#21630,#3566);
#3029=LINE('',#21678,#3567);
#3030=LINE('',#21729,#3568);
#3031=LINE('',#21780,#3569);
#3032=LINE('',#21828,#3570);
#3033=LINE('',#21879,#3571);
#3034=LINE('',#21918,#3572);
#3035=LINE('',#21942,#3573);
#3036=LINE('',#21966,#3574);
#3037=LINE('',#21991,#3575);
#3038=LINE('',#22016,#3576);
#3039=LINE('',#22040,#3577);
#3040=LINE('',#22065,#3578);
#3041=LINE('',#22090,#3579);
#3042=LINE('',#22114,#3580);
#3043=LINE('',#22139,#3581);
#3044=LINE('',#22164,#3582);
#3045=LINE('',#22188,#3583);
#3046=LINE('',#22213,#3584);
#3047=LINE('',#22238,#3585);
#3048=LINE('',#22262,#3586);
#3049=LINE('',#22279,#3587);
#3050=LINE('',#22348,#3588);
#3051=LINE('',#22438,#3589);
#3052=LINE('',#22525,#3590);
#3053=LINE('',#22615,#3591);
#3054=LINE('',#22702,#3592);
#3055=LINE('',#22792,#3593);
#3056=LINE('',#22879,#3594);
#3057=LINE('',#22912,#3595);
#3058=LINE('',#22946,#3596);
#3059=LINE('',#22982,#3597);
#3060=LINE('',#23020,#3598);
#3061=LINE('',#23058,#3599);
#3062=LINE('',#23095,#3600);
#3063=LINE('',#23132,#3601);
#3064=LINE('',#23170,#3602);
#3065=LINE('',#24650,#3603);
#3066=LINE('',#24654,#3604);
#3067=LINE('',#24656,#3605);
#3068=LINE('',#24658,#3606);
#3069=LINE('',#24659,#3607);
#3070=LINE('',#27520,#3608);
#3071=LINE('',#27554,#3609);
#3072=LINE('',#27683,#3610);
#3073=LINE('',#27686,#3611);
#3074=LINE('',#28614,#3612);
#3075=LINE('',#28648,#3613);
#3076=LINE('',#28777,#3614);
#3077=LINE('',#28780,#3615);
#3078=LINE('',#34690,#3616);
#3079=LINE('',#34696,#3617);
#3080=LINE('',#34702,#3618);
#3081=LINE('',#34708,#3619);
#3082=LINE('',#34714,#3620);
#3083=LINE('',#34720,#3621);
#3084=LINE('',#34726,#3622);
#3085=LINE('',#34732,#3623);
#3086=LINE('',#34737,#3624);
#3087=LINE('',#34739,#3625);
#3088=LINE('',#34745,#3626);
#3089=LINE('',#34751,#3627);
#3090=LINE('',#34757,#3628);
#3091=LINE('',#34763,#3629);
#3092=LINE('',#34769,#3630);
#3093=LINE('',#34775,#3631);
#3094=LINE('',#34781,#3632);
#3095=LINE('',#34786,#3633);
#3096=LINE('',#34788,#3634);
#3097=LINE('',#34794,#3635);
#3098=LINE('',#34799,#3636);
#3099=LINE('',#34801,#3637);
#3100=LINE('',#34803,#3638);
#3101=LINE('',#34804,#3639);
#3102=LINE('',#34807,#3640);
#3103=LINE('',#34809,#3641);
#3104=LINE('',#34810,#3642);
#3105=LINE('',#34813,#3643);
#3106=LINE('',#34815,#3644);
#3107=LINE('',#34816,#3645);
#3108=LINE('',#34818,#3646);
#3109=LINE('',#34819,#3647);
#3110=LINE('',#34823,#3648);
#3111=LINE('',#34825,#3649);
#3112=LINE('',#34826,#3650);
#3113=LINE('',#34829,#3651);
#3114=LINE('',#34830,#3652);
#3115=LINE('',#34833,#3653);
#3116=LINE('',#34834,#3654);
#3117=LINE('',#34836,#3655);
#3118=LINE('',#34843,#3656);
#3119=LINE('',#34849,#3657);
#3120=LINE('',#34855,#3658);
#3121=LINE('',#34861,#3659);
#3122=LINE('',#34866,#3660);
#3123=LINE('',#34868,#3661);
#3124=LINE('',#34870,#3662);
#3125=LINE('',#34871,#3663);
#3126=LINE('',#34874,#3664);
#3127=LINE('',#34876,#3665);
#3128=LINE('',#34877,#3666);
#3129=LINE('',#34880,#3667);
#3130=LINE('',#34882,#3668);
#3131=LINE('',#34883,#3669);
#3132=LINE('',#34885,#3670);
#3133=LINE('',#34886,#3671);
#3134=LINE('',#34894,#3672);
#3135=LINE('',#34900,#3673);
#3136=LINE('',#34906,#3674);
#3137=LINE('',#34912,#3675);
#3138=LINE('',#34917,#3676);
#3139=LINE('',#34919,#3677);
#3140=LINE('',#34921,#3678);
#3141=LINE('',#34922,#3679);
#3142=LINE('',#34925,#3680);
#3143=LINE('',#34927,#3681);
#3144=LINE('',#34928,#3682);
#3145=LINE('',#34931,#3683);
#3146=LINE('',#34933,#3684);
#3147=LINE('',#34934,#3685);
#3148=LINE('',#34936,#3686);
#3149=LINE('',#34937,#3687);
#3150=LINE('',#34941,#3688);
#3151=LINE('',#34943,#3689);
#3152=LINE('',#34945,#3690);
#3153=LINE('',#34946,#3691);
#3154=LINE('',#34949,#3692);
#3155=LINE('',#34951,#3693);
#3156=LINE('',#34952,#3694);
#3157=LINE('',#34955,#3695);
#3158=LINE('',#34957,#3696);
#3159=LINE('',#34958,#3697);
#3160=LINE('',#34960,#3698);
#3161=LINE('',#34961,#3699);
#3162=LINE('',#34969,#3700);
#3163=LINE('',#34975,#3701);
#3164=LINE('',#34984,#3702);
#3165=LINE('',#34990,#3703);
#3166=LINE('',#34996,#3704);
#3167=LINE('',#35002,#3705);
#3168=LINE('',#35008,#3706);
#3169=LINE('',#35014,#3707);
#3170=LINE('',#35020,#3708);
#3171=LINE('',#35026,#3709);
#3172=LINE('',#35032,#3710);
#3173=LINE('',#35038,#3711);
#3174=LINE('',#35044,#3712);
#3175=LINE('',#35050,#3713);
#3176=LINE('',#35056,#3714);
#3177=LINE('',#35062,#3715);
#3178=LINE('',#35068,#3716);
#3179=LINE('',#35074,#3717);
#3180=LINE('',#35080,#3718);
#3181=LINE('',#35086,#3719);
#3182=LINE('',#35091,#3720);
#3183=LINE('',#35093,#3721);
#3184=LINE('',#35095,#3722);
#3185=LINE('',#35096,#3723);
#3186=LINE('',#35099,#3724);
#3187=LINE('',#35101,#3725);
#3188=LINE('',#35102,#3726);
#3189=LINE('',#35105,#3727);
#3190=LINE('',#35107,#3728);
#3191=LINE('',#35108,#3729);
#3192=LINE('',#35110,#3730);
#3193=LINE('',#35111,#3731);
#3194=LINE('',#35119,#3732);
#3195=LINE('',#35125,#3733);
#3196=LINE('',#35131,#3734);
#3197=LINE('',#35137,#3735);
#3198=LINE('',#35143,#3736);
#3199=LINE('',#35149,#3737);
#3200=LINE('',#35155,#3738);
#3201=LINE('',#35160,#3739);
#3202=LINE('',#35162,#3740);
#3203=LINE('',#35164,#3741);
#3204=LINE('',#35165,#3742);
#3205=LINE('',#35168,#3743);
#3206=LINE('',#35170,#3744);
#3207=LINE('',#35171,#3745);
#3208=LINE('',#35174,#3746);
#3209=LINE('',#35176,#3747);
#3210=LINE('',#35177,#3748);
#3211=LINE('',#35179,#3749);
#3212=LINE('',#35180,#3750);
#3213=LINE('',#35187,#3751);
#3214=LINE('',#35211,#3752);
#3215=LINE('',#35259,#3753);
#3216=LINE('',#35307,#3754);
#3217=LINE('',#35361,#3755);
#3218=LINE('',#35409,#3756);
#3219=LINE('',#35457,#3757);
#3220=LINE('',#35505,#3758);
#3221=LINE('',#35559,#3759);
#3222=LINE('',#35607,#3760);
#3223=LINE('',#35655,#3761);
#3224=LINE('',#35709,#3762);
#3225=LINE('',#35757,#3763);
#3226=LINE('',#35805,#3764);
#3227=LINE('',#35856,#3765);
#3228=LINE('',#35907,#3766);
#3229=LINE('',#35955,#3767);
#3230=LINE('',#35977,#3768);
#3231=LINE('',#36001,#3769);
#3232=LINE('',#36025,#3770);
#3233=LINE('',#36051,#3771);
#3234=LINE('',#36075,#3772);
#3235=LINE('',#36099,#3773);
#3236=LINE('',#36124,#3774);
#3237=LINE('',#36149,#3775);
#3238=LINE('',#36173,#3776);
#3239=LINE('',#36198,#3777);
#3240=LINE('',#36223,#3778);
#3241=LINE('',#36247,#3779);
#3242=LINE('',#36271,#3780);
#3243=LINE('',#36296,#3781);
#3244=LINE('',#36321,#3782);
#3245=LINE('',#36636,#3783);
#3246=LINE('',#37718,#3784);
#3247=LINE('',#37720,#3785);
#3248=LINE('',#37722,#3786);
#3249=LINE('',#37723,#3787);
#3250=LINE('',#37726,#3788);
#3251=LINE('',#37728,#3789);
#3252=LINE('',#37729,#3790);
#3253=LINE('',#37732,#3791);
#3254=LINE('',#37734,#3792);
#3255=LINE('',#37735,#3793);
#3256=LINE('',#37738,#3794);
#3257=LINE('',#37740,#3795);
#3258=LINE('',#37741,#3796);
#3259=LINE('',#37744,#3797);
#3260=LINE('',#37746,#3798);
#3261=LINE('',#37747,#3799);
#3262=LINE('',#37749,#3800);
#3263=LINE('',#37750,#3801);
#3264=LINE('',#37757,#3802);
#3265=LINE('',#37765,#3803);
#3266=LINE('',#37789,#3804);
#3267=LINE('',#37837,#3805);
#3268=LINE('',#37885,#3806);
#3269=LINE('',#37939,#3807);
#3270=LINE('',#37987,#3808);
#3271=LINE('',#38035,#3809);
#3272=LINE('',#38089,#3810);
#3273=LINE('',#38137,#3811);
#3274=LINE('',#38188,#3812);
#3275=LINE('',#38239,#3813);
#3276=LINE('',#38287,#3814);
#3277=LINE('',#38312,#3815);
#3278=LINE('',#38337,#3816);
#3279=LINE('',#38361,#3817);
#3280=LINE('',#38387,#3818);
#3281=LINE('',#38411,#3819);
#3282=LINE('',#38436,#3820);
#3283=LINE('',#38461,#3821);
#3284=LINE('',#38485,#3822);
#3285=LINE('',#38510,#3823);
#3286=LINE('',#38535,#3824);
#3287=LINE('',#38871,#3825);
#3288=LINE('',#39739,#3826);
#3289=LINE('',#39741,#3827);
#3290=LINE('',#39743,#3828);
#3291=LINE('',#39744,#3829);
#3292=LINE('',#39747,#3830);
#3293=LINE('',#39749,#3831);
#3294=LINE('',#39750,#3832);
#3295=LINE('',#39753,#3833);
#3296=LINE('',#39755,#3834);
#3297=LINE('',#39756,#3835);
#3298=LINE('',#39759,#3836);
#3299=LINE('',#39761,#3837);
#3300=LINE('',#39762,#3838);
#3301=LINE('',#39765,#3839);
#3302=LINE('',#39767,#3840);
#3303=LINE('',#39768,#3841);
#3304=LINE('',#39770,#3842);
#3305=LINE('',#39771,#3843);
#3306=LINE('',#39778,#3844);
#3307=LINE('',#39786,#3845);
#3308=LINE('',#39819,#3846);
#3309=LINE('',#39903,#3847);
#3310=LINE('',#39993,#3848);
#3311=LINE('',#40083,#3849);
#3312=LINE('',#40167,#3850);
#3313=LINE('',#40257,#3851);
#3314=LINE('',#40344,#3852);
#3315=LINE('',#40431,#3853);
#3316=LINE('',#40521,#3854);
#3317=LINE('',#40605,#3855);
#3318=LINE('',#40634,#3856);
#3319=LINE('',#40671,#3857);
#3320=LINE('',#40709,#3858);
#3321=LINE('',#40745,#3859);
#3322=LINE('',#40783,#3860);
#3323=LINE('',#40820,#3861);
#3324=LINE('',#40857,#3862);
#3325=LINE('',#40895,#3863);
#3326=LINE('',#42454,#3864);
#3327=LINE('',#42457,#3865);
#3328=LINE('',#42468,#3866);
#3329=LINE('',#42471,#3867);
#3330=LINE('',#42482,#3868);
#3331=LINE('',#42485,#3869);
#3332=LINE('',#42490,#3870);
#3333=LINE('',#42499,#3871);
#3334=LINE('',#42505,#3872);
#3335=LINE('',#42512,#3873);
#3336=LINE('',#42518,#3874);
#3337=VECTOR('',#11312,2.);
#3338=VECTOR('',#11315,2.);
#3339=VECTOR('',#11320,2.);
#3340=VECTOR('',#11323,2.);
#3341=VECTOR('',#11326,2.);
#3342=VECTOR('',#11329,2.);
#3343=VECTOR('',#11332,2.);
#3344=VECTOR('',#11335,2.);
#3345=VECTOR('',#11338,2.);
#3346=VECTOR('',#11341,2.);
#3347=VECTOR('',#11344,2.);
#3348=VECTOR('',#11347,2.);
#3349=VECTOR('',#11350,2.);
#3350=VECTOR('',#11353,2.);
#3351=VECTOR('',#11356,2.);
#3352=VECTOR('',#11359,2.);
#3353=VECTOR('',#11364,2.05475000000001);
#3354=VECTOR('',#11369,2.05475000000001);
#3355=VECTOR('',#11372,2.05475000000001);
#3356=VECTOR('',#11375,2.05475000000001);
#3357=VECTOR('',#11378,2.05475000000001);
#3358=VECTOR('',#11381,2.05475000000001);
#3359=VECTOR('',#11384,2.05475000000001);
#3360=VECTOR('',#11387,2.05475000000001);
#3361=VECTOR('',#11390,2.05475000000001);
#3362=VECTOR('',#11393,2.05475000000001);
#3363=VECTOR('',#11396,2.05475000000001);
#3364=VECTOR('',#11399,2.05475000000001);
#3365=VECTOR('',#11402,2.05475000000001);
#3366=VECTOR('',#11405,2.05475000000001);
#3367=VECTOR('',#11408,2.05475000000001);
#3368=VECTOR('',#11411,2.05475000000001);
#3369=VECTOR('',#11416,2.);
#3370=VECTOR('',#11419,2.);
#3371=VECTOR('',#11424,2.);
#3372=VECTOR('',#11427,2.);
#3373=VECTOR('',#11430,2.);
#3374=VECTOR('',#11433,2.);
#3375=VECTOR('',#11436,2.);
#3376=VECTOR('',#11439,2.);
#3377=VECTOR('',#11442,2.);
#3378=VECTOR('',#11445,2.);
#3379=VECTOR('',#11448,2.);
#3380=VECTOR('',#11451,2.);
#3381=VECTOR('',#11454,2.);
#3382=VECTOR('',#11457,2.);
#3383=VECTOR('',#11460,2.);
#3384=VECTOR('',#11463,2.);
#3385=VECTOR('',#11468,2.05475);
#3386=VECTOR('',#11473,2.05475);
#3387=VECTOR('',#11476,2.05475);
#3388=VECTOR('',#11479,2.05475);
#3389=VECTOR('',#11482,2.05475);
#3390=VECTOR('',#11485,2.05475);
#3391=VECTOR('',#11488,2.05475);
#3392=VECTOR('',#11491,2.05475);
#3393=VECTOR('',#11494,2.05475);
#3394=VECTOR('',#11497,2.05475);
#3395=VECTOR('',#11500,2.05475);
#3396=VECTOR('',#11503,2.05475);
#3397=VECTOR('',#11506,2.05475);
#3398=VECTOR('',#11509,2.05475);
#3399=VECTOR('',#11512,2.05475);
#3400=VECTOR('',#11515,2.05475);
#3401=VECTOR('',#11520,2.);
#3402=VECTOR('',#11523,2.);
#3403=VECTOR('',#11528,2.);
#3404=VECTOR('',#11531,2.);
#3405=VECTOR('',#11534,2.);
#3406=VECTOR('',#11537,2.);
#3407=VECTOR('',#11540,2.);
#3408=VECTOR('',#11543,2.);
#3409=VECTOR('',#11546,2.);
#3410=VECTOR('',#11549,2.);
#3411=VECTOR('',#11552,2.);
#3412=VECTOR('',#11555,2.);
#3413=VECTOR('',#11558,2.);
#3414=VECTOR('',#11561,2.);
#3415=VECTOR('',#11564,2.);
#3416=VECTOR('',#11567,2.);
#3417=VECTOR('',#11572,2.05475000000001);
#3418=VECTOR('',#11577,2.05475000000001);
#3419=VECTOR('',#11580,2.05475000000001);
#3420=VECTOR('',#11583,2.05475000000001);
#3421=VECTOR('',#11586,2.05475000000001);
#3422=VECTOR('',#11589,2.05475000000001);
#3423=VECTOR('',#11592,2.05475000000001);
#3424=VECTOR('',#11595,2.05475000000001);
#3425=VECTOR('',#11598,2.05475000000001);
#3426=VECTOR('',#11601,2.05475000000001);
#3427=VECTOR('',#11604,2.05475000000001);
#3428=VECTOR('',#11607,2.05475000000001);
#3429=VECTOR('',#11610,2.05475000000001);
#3430=VECTOR('',#11613,2.05475000000001);
#3431=VECTOR('',#11616,2.05475000000001);
#3432=VECTOR('',#11619,2.05475000000001);
#3433=VECTOR('',#11624,2.);
#3434=VECTOR('',#11627,2.);
#3435=VECTOR('',#11632,2.);
#3436=VECTOR('',#11635,2.);
#3437=VECTOR('',#11638,2.);
#3438=VECTOR('',#11641,2.);
#3439=VECTOR('',#11644,2.);
#3440=VECTOR('',#11647,2.);
#3441=VECTOR('',#11650,2.);
#3442=VECTOR('',#11653,2.);
#3443=VECTOR('',#11656,2.);
#3444=VECTOR('',#11659,2.);
#3445=VECTOR('',#11662,2.);
#3446=VECTOR('',#11665,2.);
#3447=VECTOR('',#11668,2.);
#3448=VECTOR('',#11671,2.);
#3449=VECTOR('',#11676,2.05475);
#3450=VECTOR('',#11681,2.05475);
#3451=VECTOR('',#11684,2.05475);
#3452=VECTOR('',#11687,2.05475);
#3453=VECTOR('',#11690,2.05475);
#3454=VECTOR('',#11693,2.05475);
#3455=VECTOR('',#11696,2.05475);
#3456=VECTOR('',#11699,2.05475);
#3457=VECTOR('',#11702,2.05475);
#3458=VECTOR('',#11705,2.05475);
#3459=VECTOR('',#11708,2.05475);
#3460=VECTOR('',#11711,2.05475);
#3461=VECTOR('',#11714,2.05475);
#3462=VECTOR('',#11717,2.05475);
#3463=VECTOR('',#11720,2.05475);
#3464=VECTOR('',#11723,2.05475);
#3465=VECTOR('',#11728,3.);
#3466=VECTOR('',#11735,3.);
#3467=VECTOR('',#11738,3.);
#3468=VECTOR('',#11741,3.);
#3469=VECTOR('',#11744,3.);
#3470=VECTOR('',#11747,3.);
#3471=VECTOR('',#11750,3.);
#3472=VECTOR('',#11753,3.);
#3473=VECTOR('',#11756,3.);
#3474=VECTOR('',#11759,3.);
#3475=VECTOR('',#11762,3.);
#3476=VECTOR('',#11765,3.);
#3477=VECTOR('',#11768,3.);
#3478=VECTOR('',#11771,3.);
#3479=VECTOR('',#11774,3.);
#3480=VECTOR('',#11779,3.);
#3481=VECTOR('',#11786,3.);
#3482=VECTOR('',#11789,3.);
#3483=VECTOR('',#11792,3.);
#3484=VECTOR('',#11795,3.);
#3485=VECTOR('',#11798,3.);
#3486=VECTOR('',#11801,3.);
#3487=VECTOR('',#11804,3.);
#3488=VECTOR('',#11807,3.);
#3489=VECTOR('',#11810,3.);
#3490=VECTOR('',#11813,3.);
#3491=VECTOR('',#11816,3.);
#3492=VECTOR('',#11819,3.);
#3493=VECTOR('',#11822,3.);
#3494=VECTOR('',#11825,3.);
#3495=VECTOR('',#11830,3.0735);
#3496=VECTOR('',#11835,3.0735);
#3497=VECTOR('',#11838,3.0735);
#3498=VECTOR('',#11841,3.0735);
#3499=VECTOR('',#11844,3.0735);
#3500=VECTOR('',#11847,3.0735);
#3501=VECTOR('',#11850,3.0735);
#3502=VECTOR('',#11853,3.0735);
#3503=VECTOR('',#11856,3.0735);
#3504=VECTOR('',#11859,3.0735);
#3505=VECTOR('',#11862,3.0735);
#3506=VECTOR('',#11865,3.0735);
#3507=VECTOR('',#11868,3.0735);
#3508=VECTOR('',#11871,3.0735);
#3509=VECTOR('',#11874,3.0735);
#3510=VECTOR('',#11879,3.0735);
#3511=VECTOR('',#11884,3.0735);
#3512=VECTOR('',#11887,3.0735);
#3513=VECTOR('',#11890,3.0735);
#3514=VECTOR('',#11893,3.0735);
#3515=VECTOR('',#11896,3.0735);
#3516=VECTOR('',#11899,3.0735);
#3517=VECTOR('',#11902,3.0735);
#3518=VECTOR('',#11905,3.0735);
#3519=VECTOR('',#11908,3.0735);
#3520=VECTOR('',#11911,3.0735);
#3521=VECTOR('',#11914,3.0735);
#3522=VECTOR('',#11917,3.0735);
#3523=VECTOR('',#11920,3.0735);
#3524=VECTOR('',#11923,3.0735);
#3525=VECTOR('',#11928,3.);
#3526=VECTOR('',#11931,3.);
#3527=VECTOR('',#11938,3.);
#3528=VECTOR('',#11941,3.);
#3529=VECTOR('',#11944,3.);
#3530=VECTOR('',#11947,3.);
#3531=VECTOR('',#11950,3.);
#3532=VECTOR('',#11953,3.);
#3533=VECTOR('',#11956,3.);
#3534=VECTOR('',#11959,3.);
#3535=VECTOR('',#11962,3.);
#3536=VECTOR('',#11965,3.);
#3537=VECTOR('',#11968,3.);
#3538=VECTOR('',#11971,3.);
#3539=VECTOR('',#11974,3.);
#3540=VECTOR('',#11977,3.);
#3541=VECTOR('',#11982,3.0735);
#3542=VECTOR('',#11987,3.0735);
#3543=VECTOR('',#11990,3.0735);
#3544=VECTOR('',#11993,3.0735);
#3545=VECTOR('',#11996,3.0735);
#3546=VECTOR('',#11999,3.0735);
#3547=VECTOR('',#12002,3.0735);
#3548=VECTOR('',#12005,3.0735);
#3549=VECTOR('',#12008,3.0735);
#3550=VECTOR('',#12011,3.0735);
#3551=VECTOR('',#12014,3.0735);
#3552=VECTOR('',#12017,3.0735);
#3553=VECTOR('',#12020,3.0735);
#3554=VECTOR('',#12023,3.0735);
#3555=VECTOR('',#12026,3.0735);
#3556=VECTOR('',#12031,3.);
#3557=VECTOR('',#12034,3.);
#3558=VECTOR('',#12041,3.);
#3559=VECTOR('',#12044,3.);
#3560=VECTOR('',#12047,3.);
#3561=VECTOR('',#12050,3.);
#3562=VECTOR('',#12053,3.);
#3563=VECTOR('',#12056,3.);
#3564=VECTOR('',#12059,3.);
#3565=VECTOR('',#12062,3.);
#3566=VECTOR('',#12065,3.);
#3567=VECTOR('',#12068,3.);
#3568=VECTOR('',#12071,3.);
#3569=VECTOR('',#12074,3.);
#3570=VECTOR('',#12077,3.);
#3571=VECTOR('',#12080,3.);
#3572=VECTOR('',#12085,3.0735);
#3573=VECTOR('',#12090,3.0735);
#3574=VECTOR('',#12093,3.0735);
#3575=VECTOR('',#12096,3.0735);
#3576=VECTOR('',#12099,3.0735);
#3577=VECTOR('',#12102,3.0735);
#3578=VECTOR('',#12105,3.0735);
#3579=VECTOR('',#12108,3.0735);
#3580=VECTOR('',#12111,3.0735);
#3581=VECTOR('',#12114,3.0735);
#3582=VECTOR('',#12117,3.0735);
#3583=VECTOR('',#12120,3.0735);
#3584=VECTOR('',#12123,3.0735);
#3585=VECTOR('',#12126,3.0735);
#3586=VECTOR('',#12129,3.0735);
#3587=VECTOR('',#12134,8.);
#3588=VECTOR('',#12139,8.);
#3589=VECTOR('',#12142,8.);
#3590=VECTOR('',#12145,8.);
#3591=VECTOR('',#12148,8.);
#3592=VECTOR('',#12151,8.);
#3593=VECTOR('',#12154,8.);
#3594=VECTOR('',#12157,8.);
#3595=VECTOR('',#12162,8.1015);
#3596=VECTOR('',#12167,8.1015);
#3597=VECTOR('',#12170,8.1015);
#3598=VECTOR('',#12173,8.1015);
#3599=VECTOR('',#12176,8.1015);
#3600=VECTOR('',#12179,8.1015);
#3601=VECTOR('',#12182,8.1015);
#3602=VECTOR('',#12185,8.1015);
#3603=VECTOR('',#12200,12.);
#3604=VECTOR('',#12203,10.);
#3605=VECTOR('',#12204,10.);
#3606=VECTOR('',#12205,10.);
#3607=VECTOR('',#12206,10.);
#3608=VECTOR('',#12221,10.);
#3609=VECTOR('',#12224,10.);
#3610=VECTOR('',#12225,10.);
#3611=VECTOR('',#12230,10.);
#3612=VECTOR('',#12237,10.);
#3613=VECTOR('',#12240,10.);
#3614=VECTOR('',#12241,10.);
#3615=VECTOR('',#12246,10.);
#3616=VECTOR('',#12295,5.);
#3617=VECTOR('',#12302,5.);
#3618=VECTOR('',#12309,5.);
#3619=VECTOR('',#12316,5.);
#3620=VECTOR('',#12323,5.);
#3621=VECTOR('',#12330,5.);
#3622=VECTOR('',#12337,5.);
#3623=VECTOR('',#12344,5.);
#3624=VECTOR('',#12351,5.);
#3625=VECTOR('',#12352,5.);
#3626=VECTOR('',#12359,5.);
#3627=VECTOR('',#12366,5.);
#3628=VECTOR('',#12373,5.);
#3629=VECTOR('',#12380,5.);
#3630=VECTOR('',#12387,5.);
#3631=VECTOR('',#12394,5.);
#3632=VECTOR('',#12401,5.);
#3633=VECTOR('',#12408,5.);
#3634=VECTOR('',#12409,5.);
#3635=VECTOR('',#12416,5.);
#3636=VECTOR('',#12421,10.);
#3637=VECTOR('',#12422,10.);
#3638=VECTOR('',#12423,10.);
#3639=VECTOR('',#12424,10.);
#3640=VECTOR('',#12427,10.);
#3641=VECTOR('',#12428,10.);
#3642=VECTOR('',#12429,10.);
#3643=VECTOR('',#12432,10.);
#3644=VECTOR('',#12433,10.);
#3645=VECTOR('',#12434,10.);
#3646=VECTOR('',#12437,10.);
#3647=VECTOR('',#12438,10.);
#3648=VECTOR('',#12443,10.);
#3649=VECTOR('',#12444,10.);
#3650=VECTOR('',#12445,10.);
#3651=VECTOR('',#12448,10.);
#3652=VECTOR('',#12449,10.);
#3653=VECTOR('',#12452,10.);
#3654=VECTOR('',#12453,10.);
#3655=VECTOR('',#12456,10.);
#3656=VECTOR('',#12465,2.5);
#3657=VECTOR('',#12472,2.5);
#3658=VECTOR('',#12479,2.5);
#3659=VECTOR('',#12486,2.5);
#3660=VECTOR('',#12491,10.);
#3661=VECTOR('',#12492,10.);
#3662=VECTOR('',#12493,10.);
#3663=VECTOR('',#12494,10.);
#3664=VECTOR('',#12497,10.);
#3665=VECTOR('',#12498,10.);
#3666=VECTOR('',#12499,10.);
#3667=VECTOR('',#12502,10.);
#3668=VECTOR('',#12503,10.);
#3669=VECTOR('',#12504,10.);
#3670=VECTOR('',#12507,10.);
#3671=VECTOR('',#12508,10.);
#3672=VECTOR('',#12519,2.5);
#3673=VECTOR('',#12526,2.5);
#3674=VECTOR('',#12533,2.5);
#3675=VECTOR('',#12540,2.5);
#3676=VECTOR('',#12545,10.);
#3677=VECTOR('',#12546,10.);
#3678=VECTOR('',#12547,10.);
#3679=VECTOR('',#12548,10.);
#3680=VECTOR('',#12551,10.);
#3681=VECTOR('',#12552,10.);
#3682=VECTOR('',#12553,10.);
#3683=VECTOR('',#12556,10.);
#3684=VECTOR('',#12557,10.);
#3685=VECTOR('',#12558,10.);
#3686=VECTOR('',#12561,10.);
#3687=VECTOR('',#12562,10.);
#3688=VECTOR('',#12565,10.);
#3689=VECTOR('',#12566,10.);
#3690=VECTOR('',#12567,10.);
#3691=VECTOR('',#12568,10.);
#3692=VECTOR('',#12571,10.);
#3693=VECTOR('',#12572,10.);
#3694=VECTOR('',#12573,10.);
#3695=VECTOR('',#12576,10.);
#3696=VECTOR('',#12577,10.);
#3697=VECTOR('',#12578,10.);
#3698=VECTOR('',#12581,10.);
#3699=VECTOR('',#12582,10.);
#3700=VECTOR('',#12593,4.);
#3701=VECTOR('',#12600,5.);
#3702=VECTOR('',#12613,5.);
#3703=VECTOR('',#12620,5.);
#3704=VECTOR('',#12627,5.);
#3705=VECTOR('',#12634,5.);
#3706=VECTOR('',#12641,5.);
#3707=VECTOR('',#12648,5.);
#3708=VECTOR('',#12655,5.);
#3709=VECTOR('',#12662,5.);
#3710=VECTOR('',#12669,5.);
#3711=VECTOR('',#12676,5.);
#3712=VECTOR('',#12683,5.);
#3713=VECTOR('',#12690,5.);
#3714=VECTOR('',#12697,5.);
#3715=VECTOR('',#12704,5.);
#3716=VECTOR('',#12711,5.);
#3717=VECTOR('',#12718,5.);
#3718=VECTOR('',#12725,5.);
#3719=VECTOR('',#12732,5.);
#3720=VECTOR('',#12737,10.);
#3721=VECTOR('',#12738,10.);
#3722=VECTOR('',#12739,10.);
#3723=VECTOR('',#12740,10.);
#3724=VECTOR('',#12743,10.);
#3725=VECTOR('',#12744,10.);
#3726=VECTOR('',#12745,10.);
#3727=VECTOR('',#12748,10.);
#3728=VECTOR('',#12749,10.);
#3729=VECTOR('',#12750,10.);
#3730=VECTOR('',#12753,10.);
#3731=VECTOR('',#12754,10.);
#3732=VECTOR('',#12765,13.);
#3733=VECTOR('',#12772,4.5);
#3734=VECTOR('',#12779,4.5);
#3735=VECTOR('',#12786,3.5);
#3736=VECTOR('',#12793,3.5);
#3737=VECTOR('',#12800,3.5);
#3738=VECTOR('',#12807,3.5);
#3739=VECTOR('',#12812,10.);
#3740=VECTOR('',#12813,10.);
#3741=VECTOR('',#12814,10.);
#3742=VECTOR('',#12815,10.);
#3743=VECTOR('',#12818,10.);
#3744=VECTOR('',#12819,10.);
#3745=VECTOR('',#12820,10.);
#3746=VECTOR('',#12823,10.);
#3747=VECTOR('',#12824,10.);
#3748=VECTOR('',#12825,10.);
#3749=VECTOR('',#12828,10.);
#3750=VECTOR('',#12829,10.);
#3751=VECTOR('',#12838,2.);
#3752=VECTOR('',#12843,2.);
#3753=VECTOR('',#12846,2.);
#3754=VECTOR('',#12849,2.);
#3755=VECTOR('',#12852,2.);
#3756=VECTOR('',#12855,2.);
#3757=VECTOR('',#12858,2.);
#3758=VECTOR('',#12861,2.);
#3759=VECTOR('',#12864,2.);
#3760=VECTOR('',#12867,2.);
#3761=VECTOR('',#12870,2.);
#3762=VECTOR('',#12873,2.);
#3763=VECTOR('',#12876,2.);
#3764=VECTOR('',#12879,2.);
#3765=VECTOR('',#12882,2.);
#3766=VECTOR('',#12885,2.);
#3767=VECTOR('',#12888,1.5555);
#3768=VECTOR('',#12893,1.5555);
#3769=VECTOR('',#12896,1.5555);
#3770=VECTOR('',#12899,1.5555);
#3771=VECTOR('',#12902,1.5555);
#3772=VECTOR('',#12905,1.5555);
#3773=VECTOR('',#12908,1.5555);
#3774=VECTOR('',#12911,1.5555);
#3775=VECTOR('',#12914,1.5555);
#3776=VECTOR('',#12917,1.5555);
#3777=VECTOR('',#12920,1.5555);
#3778=VECTOR('',#12923,1.5555);
#3779=VECTOR('',#12926,1.5555);
#3780=VECTOR('',#12929,1.5555);
#3781=VECTOR('',#12932,1.5555);
#3782=VECTOR('',#12935,1.5555);
#3783=VECTOR('',#12940,1.5);
#3784=VECTOR('',#12951,10.);
#3785=VECTOR('',#12952,10.);
#3786=VECTOR('',#12953,10.);
#3787=VECTOR('',#12954,10.);
#3788=VECTOR('',#12957,10.);
#3789=VECTOR('',#12958,10.);
#3790=VECTOR('',#12959,10.);
#3791=VECTOR('',#12962,10.);
#3792=VECTOR('',#12963,10.);
#3793=VECTOR('',#12964,10.);
#3794=VECTOR('',#12967,10.);
#3795=VECTOR('',#12968,10.);
#3796=VECTOR('',#12969,10.);
#3797=VECTOR('',#12972,10.);
#3798=VECTOR('',#12973,10.);
#3799=VECTOR('',#12974,10.);
#3800=VECTOR('',#12977,10.);
#3801=VECTOR('',#12978,10.);
#3802=VECTOR('',#12987,3.5);
#3803=VECTOR('',#12998,3.);
#3804=VECTOR('',#13003,3.);
#3805=VECTOR('',#13006,3.);
#3806=VECTOR('',#13009,3.);
#3807=VECTOR('',#13012,3.);
#3808=VECTOR('',#13015,3.);
#3809=VECTOR('',#13018,3.);
#3810=VECTOR('',#13021,3.);
#3811=VECTOR('',#13024,3.);
#3812=VECTOR('',#13027,3.);
#3813=VECTOR('',#13030,3.);
#3814=VECTOR('',#13033,2.37175);
#3815=VECTOR('',#13038,2.37175);
#3816=VECTOR('',#13041,2.37175);
#3817=VECTOR('',#13044,2.37175);
#3818=VECTOR('',#13047,2.37175);
#3819=VECTOR('',#13050,2.37175);
#3820=VECTOR('',#13053,2.37175);
#3821=VECTOR('',#13056,2.37175);
#3822=VECTOR('',#13059,2.37175);
#3823=VECTOR('',#13062,2.37175);
#3824=VECTOR('',#13065,2.37175);
#3825=VECTOR('',#13070,2.5);
#3826=VECTOR('',#13081,10.);
#3827=VECTOR('',#13082,10.);
#3828=VECTOR('',#13083,10.);
#3829=VECTOR('',#13084,10.);
#3830=VECTOR('',#13087,10.);
#3831=VECTOR('',#13088,10.);
#3832=VECTOR('',#13089,10.);
#3833=VECTOR('',#13092,10.);
#3834=VECTOR('',#13093,10.);
#3835=VECTOR('',#13094,10.);
#3836=VECTOR('',#13097,10.);
#3837=VECTOR('',#13098,10.);
#3838=VECTOR('',#13099,10.);
#3839=VECTOR('',#13102,10.);
#3840=VECTOR('',#13103,10.);
#3841=VECTOR('',#13104,10.);
#3842=VECTOR('',#13107,10.);
#3843=VECTOR('',#13108,10.);
#3844=VECTOR('',#13117,5.);
#3845=VECTOR('',#13128,8.);
#3846=VECTOR('',#13133,8.);
#3847=VECTOR('',#13136,8.);
#3848=VECTOR('',#13139,8.);
#3849=VECTOR('',#13142,8.);
#3850=VECTOR('',#13145,8.);
#3851=VECTOR('',#13148,8.);
#3852=VECTOR('',#13151,8.);
#3853=VECTOR('',#13154,8.);
#3854=VECTOR('',#13157,8.);
#3855=VECTOR('',#13160,7.0685);
#3856=VECTOR('',#13165,7.0685);
#3857=VECTOR('',#13168,7.0685);
#3858=VECTOR('',#13171,7.0685);
#3859=VECTOR('',#13174,7.0685);
#3860=VECTOR('',#13177,7.0685);
#3861=VECTOR('',#13180,7.0685);
#3862=VECTOR('',#13183,7.0685);
#3863=VECTOR('',#13186,7.0685);
#3864=VECTOR('',#13209,7.);
#3865=VECTOR('',#13212,6.);
#3866=VECTOR('',#13227,7.);
#3867=VECTOR('',#13230,6.);
#3868=VECTOR('',#13245,7.);
#3869=VECTOR('',#13248,6.);
#3870=VECTOR('',#13255,6.);
#3871=VECTOR('',#13266,12.);
#3872=VECTOR('',#13275,4.);
#3873=VECTOR('',#13284,8.5);
#3874=VECTOR('',#13291,12.);
#3875=VERTEX_POINT('',#13451);
#3876=VERTEX_POINT('',#13452);
#3877=VERTEX_POINT('',#13454);
#3878=VERTEX_POINT('',#13474);
#3879=VERTEX_POINT('',#13476);
#3880=VERTEX_POINT('',#13481);
#3881=VERTEX_POINT('',#13507);
#3882=VERTEX_POINT('',#13508);
#3883=VERTEX_POINT('',#13558);
#3884=VERTEX_POINT('',#13559);
#3885=VERTEX_POINT('',#13606);
#3886=VERTEX_POINT('',#13607);
#3887=VERTEX_POINT('',#13657);
#3888=VERTEX_POINT('',#13658);
#3889=VERTEX_POINT('',#13708);
#3890=VERTEX_POINT('',#13709);
#3891=VERTEX_POINT('',#13756);
#3892=VERTEX_POINT('',#13757);
#3893=VERTEX_POINT('',#13804);
#3894=VERTEX_POINT('',#13805);
#3895=VERTEX_POINT('',#13855);
#3896=VERTEX_POINT('',#13856);
#3897=VERTEX_POINT('',#13903);
#3898=VERTEX_POINT('',#13904);
#3899=VERTEX_POINT('',#13951);
#3900=VERTEX_POINT('',#13952);
#3901=VERTEX_POINT('',#14002);
#3902=VERTEX_POINT('',#14003);
#3903=VERTEX_POINT('',#14053);
#3904=VERTEX_POINT('',#14054);
#3905=VERTEX_POINT('',#14101);
#3906=VERTEX_POINT('',#14102);
#3907=VERTEX_POINT('',#14152);
#3908=VERTEX_POINT('',#14153);
#3909=VERTEX_POINT('',#14155);
#3910=VERTEX_POINT('',#14169);
#3911=VERTEX_POINT('',#14191);
#3912=VERTEX_POINT('',#14192);
#3913=VERTEX_POINT('',#14194);
#3914=VERTEX_POINT('',#14201);
#3915=VERTEX_POINT('',#14211);
#3916=VERTEX_POINT('',#14212);
#3917=VERTEX_POINT('',#14235);
#3918=VERTEX_POINT('',#14236);
#3919=VERTEX_POINT('',#14260);
#3920=VERTEX_POINT('',#14261);
#3921=VERTEX_POINT('',#14285);
#3922=VERTEX_POINT('',#14286);
#3923=VERTEX_POINT('',#14309);
#3924=VERTEX_POINT('',#14310);
#3925=VERTEX_POINT('',#14334);
#3926=VERTEX_POINT('',#14335);
#3927=VERTEX_POINT('',#14358);
#3928=VERTEX_POINT('',#14359);
#3929=VERTEX_POINT('',#14383);
#3930=VERTEX_POINT('',#14384);
#3931=VERTEX_POINT('',#14408);
#3932=VERTEX_POINT('',#14409);
#3933=VERTEX_POINT('',#14432);
#3934=VERTEX_POINT('',#14433);
#3935=VERTEX_POINT('',#14457);
#3936=VERTEX_POINT('',#14458);
#3937=VERTEX_POINT('',#14481);
#3938=VERTEX_POINT('',#14482);
#3939=VERTEX_POINT('',#14506);
#3940=VERTEX_POINT('',#14507);
#3941=VERTEX_POINT('',#14531);
#3942=VERTEX_POINT('',#14532);
#3943=VERTEX_POINT('',#14555);
#3944=VERTEX_POINT('',#14556);
#3945=VERTEX_POINT('',#14558);
#3946=VERTEX_POINT('',#14564);
#3947=VERTEX_POINT('',#14572);
#3948=VERTEX_POINT('',#14573);
#3949=VERTEX_POINT('',#14575);
#3950=VERTEX_POINT('',#14595);
#3951=VERTEX_POINT('',#14597);
#3952=VERTEX_POINT('',#14602);
#3953=VERTEX_POINT('',#14628);
#3954=VERTEX_POINT('',#14629);
#3955=VERTEX_POINT('',#14679);
#3956=VERTEX_POINT('',#14680);
#3957=VERTEX_POINT('',#14727);
#3958=VERTEX_POINT('',#14728);
#3959=VERTEX_POINT('',#14778);
#3960=VERTEX_POINT('',#14779);
#3961=VERTEX_POINT('',#14829);
#3962=VERTEX_POINT('',#14830);
#3963=VERTEX_POINT('',#14877);
#3964=VERTEX_POINT('',#14878);
#3965=VERTEX_POINT('',#14925);
#3966=VERTEX_POINT('',#14926);
#3967=VERTEX_POINT('',#14976);
#3968=VERTEX_POINT('',#14977);
#3969=VERTEX_POINT('',#15024);
#3970=VERTEX_POINT('',#15025);
#3971=VERTEX_POINT('',#15072);
#3972=VERTEX_POINT('',#15073);
#3973=VERTEX_POINT('',#15123);
#3974=VERTEX_POINT('',#15124);
#3975=VERTEX_POINT('',#15174);
#3976=VERTEX_POINT('',#15175);
#3977=VERTEX_POINT('',#15222);
#3978=VERTEX_POINT('',#15223);
#3979=VERTEX_POINT('',#15273);
#3980=VERTEX_POINT('',#15274);
#3981=VERTEX_POINT('',#15276);
#3982=VERTEX_POINT('',#15290);
#3983=VERTEX_POINT('',#15312);
#3984=VERTEX_POINT('',#15313);
#3985=VERTEX_POINT('',#15315);
#3986=VERTEX_POINT('',#15322);
#3987=VERTEX_POINT('',#15332);
#3988=VERTEX_POINT('',#15333);
#3989=VERTEX_POINT('',#15356);
#3990=VERTEX_POINT('',#15357);
#3991=VERTEX_POINT('',#15381);
#3992=VERTEX_POINT('',#15382);
#3993=VERTEX_POINT('',#15406);
#3994=VERTEX_POINT('',#15407);
#3995=VERTEX_POINT('',#15430);
#3996=VERTEX_POINT('',#15431);
#3997=VERTEX_POINT('',#15455);
#3998=VERTEX_POINT('',#15456);
#3999=VERTEX_POINT('',#15479);
#4000=VERTEX_POINT('',#15480);
#4001=VERTEX_POINT('',#15504);
#4002=VERTEX_POINT('',#15505);
#4003=VERTEX_POINT('',#15529);
#4004=VERTEX_POINT('',#15530);
#4005=VERTEX_POINT('',#15553);
#4006=VERTEX_POINT('',#15554);
#4007=VERTEX_POINT('',#15578);
#4008=VERTEX_POINT('',#15579);
#4009=VERTEX_POINT('',#15602);
#4010=VERTEX_POINT('',#15603);
#4011=VERTEX_POINT('',#15627);
#4012=VERTEX_POINT('',#15628);
#4013=VERTEX_POINT('',#15652);
#4014=VERTEX_POINT('',#15653);
#4015=VERTEX_POINT('',#15676);
#4016=VERTEX_POINT('',#15677);
#4017=VERTEX_POINT('',#15679);
#4018=VERTEX_POINT('',#15685);
#4019=VERTEX_POINT('',#15693);
#4020=VERTEX_POINT('',#15694);
#4021=VERTEX_POINT('',#15696);
#4022=VERTEX_POINT('',#15716);
#4023=VERTEX_POINT('',#15718);
#4024=VERTEX_POINT('',#15723);
#4025=VERTEX_POINT('',#15749);
#4026=VERTEX_POINT('',#15750);
#4027=VERTEX_POINT('',#15800);
#4028=VERTEX_POINT('',#15801);
#4029=VERTEX_POINT('',#15848);
#4030=VERTEX_POINT('',#15849);
#4031=VERTEX_POINT('',#15899);
#4032=VERTEX_POINT('',#15900);
#4033=VERTEX_POINT('',#15950);
#4034=VERTEX_POINT('',#15951);
#4035=VERTEX_POINT('',#15998);
#4036=VERTEX_POINT('',#15999);
#4037=VERTEX_POINT('',#16046);
#4038=VERTEX_POINT('',#16047);
#4039=VERTEX_POINT('',#16097);
#4040=VERTEX_POINT('',#16098);
#4041=VERTEX_POINT('',#16145);
#4042=VERTEX_POINT('',#16146);
#4043=VERTEX_POINT('',#16193);
#4044=VERTEX_POINT('',#16194);
#4045=VERTEX_POINT('',#16244);
#4046=VERTEX_POINT('',#16245);
#4047=VERTEX_POINT('',#16295);
#4048=VERTEX_POINT('',#16296);
#4049=VERTEX_POINT('',#16343);
#4050=VERTEX_POINT('',#16344);
#4051=VERTEX_POINT('',#16394);
#4052=VERTEX_POINT('',#16395);
#4053=VERTEX_POINT('',#16397);
#4054=VERTEX_POINT('',#16411);
#4055=VERTEX_POINT('',#16433);
#4056=VERTEX_POINT('',#16434);
#4057=VERTEX_POINT('',#16436);
#4058=VERTEX_POINT('',#16443);
#4059=VERTEX_POINT('',#16453);
#4060=VERTEX_POINT('',#16454);
#4061=VERTEX_POINT('',#16477);
#4062=VERTEX_POINT('',#16478);
#4063=VERTEX_POINT('',#16502);
#4064=VERTEX_POINT('',#16503);
#4065=VERTEX_POINT('',#16527);
#4066=VERTEX_POINT('',#16528);
#4067=VERTEX_POINT('',#16551);
#4068=VERTEX_POINT('',#16552);
#4069=VERTEX_POINT('',#16576);
#4070=VERTEX_POINT('',#16577);
#4071=VERTEX_POINT('',#16600);
#4072=VERTEX_POINT('',#16601);
#4073=VERTEX_POINT('',#16625);
#4074=VERTEX_POINT('',#16626);
#4075=VERTEX_POINT('',#16650);
#4076=VERTEX_POINT('',#16651);
#4077=VERTEX_POINT('',#16674);
#4078=VERTEX_POINT('',#16675);
#4079=VERTEX_POINT('',#16699);
#4080=VERTEX_POINT('',#16700);
#4081=VERTEX_POINT('',#16723);
#4082=VERTEX_POINT('',#16724);
#4083=VERTEX_POINT('',#16748);
#4084=VERTEX_POINT('',#16749);
#4085=VERTEX_POINT('',#16773);
#4086=VERTEX_POINT('',#16774);
#4087=VERTEX_POINT('',#16797);
#4088=VERTEX_POINT('',#16798);
#4089=VERTEX_POINT('',#16800);
#4090=VERTEX_POINT('',#16806);
#4091=VERTEX_POINT('',#16814);
#4092=VERTEX_POINT('',#16815);
#4093=VERTEX_POINT('',#16817);
#4094=VERTEX_POINT('',#16837);
#4095=VERTEX_POINT('',#16839);
#4096=VERTEX_POINT('',#16844);
#4097=VERTEX_POINT('',#16870);
#4098=VERTEX_POINT('',#16871);
#4099=VERTEX_POINT('',#16921);
#4100=VERTEX_POINT('',#16922);
#4101=VERTEX_POINT('',#16969);
#4102=VERTEX_POINT('',#16970);
#4103=VERTEX_POINT('',#17020);
#4104=VERTEX_POINT('',#17021);
#4105=VERTEX_POINT('',#17071);
#4106=VERTEX_POINT('',#17072);
#4107=VERTEX_POINT('',#17119);
#4108=VERTEX_POINT('',#17120);
#4109=VERTEX_POINT('',#17167);
#4110=VERTEX_POINT('',#17168);
#4111=VERTEX_POINT('',#17218);
#4112=VERTEX_POINT('',#17219);
#4113=VERTEX_POINT('',#17266);
#4114=VERTEX_POINT('',#17267);
#4115=VERTEX_POINT('',#17314);
#4116=VERTEX_POINT('',#17315);
#4117=VERTEX_POINT('',#17365);
#4118=VERTEX_POINT('',#17366);
#4119=VERTEX_POINT('',#17416);
#4120=VERTEX_POINT('',#17417);
#4121=VERTEX_POINT('',#17464);
#4122=VERTEX_POINT('',#17465);
#4123=VERTEX_POINT('',#17515);
#4124=VERTEX_POINT('',#17516);
#4125=VERTEX_POINT('',#17518);
#4126=VERTEX_POINT('',#17532);
#4127=VERTEX_POINT('',#17554);
#4128=VERTEX_POINT('',#17555);
#4129=VERTEX_POINT('',#17557);
#4130=VERTEX_POINT('',#17564);
#4131=VERTEX_POINT('',#17574);
#4132=VERTEX_POINT('',#17575);
#4133=VERTEX_POINT('',#17598);
#4134=VERTEX_POINT('',#17599);
#4135=VERTEX_POINT('',#17623);
#4136=VERTEX_POINT('',#17624);
#4137=VERTEX_POINT('',#17648);
#4138=VERTEX_POINT('',#17649);
#4139=VERTEX_POINT('',#17672);
#4140=VERTEX_POINT('',#17673);
#4141=VERTEX_POINT('',#17697);
#4142=VERTEX_POINT('',#17698);
#4143=VERTEX_POINT('',#17721);
#4144=VERTEX_POINT('',#17722);
#4145=VERTEX_POINT('',#17746);
#4146=VERTEX_POINT('',#17747);
#4147=VERTEX_POINT('',#17771);
#4148=VERTEX_POINT('',#17772);
#4149=VERTEX_POINT('',#17795);
#4150=VERTEX_POINT('',#17796);
#4151=VERTEX_POINT('',#17820);
#4152=VERTEX_POINT('',#17821);
#4153=VERTEX_POINT('',#17844);
#4154=VERTEX_POINT('',#17845);
#4155=VERTEX_POINT('',#17869);
#4156=VERTEX_POINT('',#17870);
#4157=VERTEX_POINT('',#17894);
#4158=VERTEX_POINT('',#17895);
#4159=VERTEX_POINT('',#17918);
#4160=VERTEX_POINT('',#17919);
#4161=VERTEX_POINT('',#17921);
#4162=VERTEX_POINT('',#17927);
#4163=VERTEX_POINT('',#17935);
#4164=VERTEX_POINT('',#17936);
#4165=VERTEX_POINT('',#17938);
#4166=VERTEX_POINT('',#17943);
#4167=VERTEX_POINT('',#17945);
#4168=VERTEX_POINT('',#17965);
#4169=VERTEX_POINT('',#17978);
#4170=VERTEX_POINT('',#17979);
#4171=VERTEX_POINT('',#18029);
#4172=VERTEX_POINT('',#18030);
#4173=VERTEX_POINT('',#18080);
#4174=VERTEX_POINT('',#18081);
#4175=VERTEX_POINT('',#18128);
#4176=VERTEX_POINT('',#18129);
#4177=VERTEX_POINT('',#18179);
#4178=VERTEX_POINT('',#18180);
#4179=VERTEX_POINT('',#18230);
#4180=VERTEX_POINT('',#18231);
#4181=VERTEX_POINT('',#18278);
#4182=VERTEX_POINT('',#18279);
#4183=VERTEX_POINT('',#18329);
#4184=VERTEX_POINT('',#18330);
#4185=VERTEX_POINT('',#18380);
#4186=VERTEX_POINT('',#18381);
#4187=VERTEX_POINT('',#18428);
#4188=VERTEX_POINT('',#18429);
#4189=VERTEX_POINT('',#18479);
#4190=VERTEX_POINT('',#18480);
#4191=VERTEX_POINT('',#18530);
#4192=VERTEX_POINT('',#18531);
#4193=VERTEX_POINT('',#18578);
#4194=VERTEX_POINT('',#18579);
#4195=VERTEX_POINT('',#18629);
#4196=VERTEX_POINT('',#18630);
#4197=VERTEX_POINT('',#18632);
#4198=VERTEX_POINT('',#18646);
#4199=VERTEX_POINT('',#18668);
#4200=VERTEX_POINT('',#18669);
#4201=VERTEX_POINT('',#18671);
#4202=VERTEX_POINT('',#18676);
#4203=VERTEX_POINT('',#18678);
#4204=VERTEX_POINT('',#18698);
#4205=VERTEX_POINT('',#18711);
#4206=VERTEX_POINT('',#18712);
#4207=VERTEX_POINT('',#18762);
#4208=VERTEX_POINT('',#18763);
#4209=VERTEX_POINT('',#18813);
#4210=VERTEX_POINT('',#18814);
#4211=VERTEX_POINT('',#18861);
#4212=VERTEX_POINT('',#18862);
#4213=VERTEX_POINT('',#18912);
#4214=VERTEX_POINT('',#18913);
#4215=VERTEX_POINT('',#18963);
#4216=VERTEX_POINT('',#18964);
#4217=VERTEX_POINT('',#19011);
#4218=VERTEX_POINT('',#19012);
#4219=VERTEX_POINT('',#19062);
#4220=VERTEX_POINT('',#19063);
#4221=VERTEX_POINT('',#19113);
#4222=VERTEX_POINT('',#19114);
#4223=VERTEX_POINT('',#19161);
#4224=VERTEX_POINT('',#19162);
#4225=VERTEX_POINT('',#19212);
#4226=VERTEX_POINT('',#19213);
#4227=VERTEX_POINT('',#19263);
#4228=VERTEX_POINT('',#19264);
#4229=VERTEX_POINT('',#19311);
#4230=VERTEX_POINT('',#19312);
#4231=VERTEX_POINT('',#19362);
#4232=VERTEX_POINT('',#19363);
#4233=VERTEX_POINT('',#19365);
#4234=VERTEX_POINT('',#19379);
#4235=VERTEX_POINT('',#19401);
#4236=VERTEX_POINT('',#19402);
#4237=VERTEX_POINT('',#19404);
#4238=VERTEX_POINT('',#19413);
#4239=VERTEX_POINT('',#19425);
#4240=VERTEX_POINT('',#19426);
#4241=VERTEX_POINT('',#19449);
#4242=VERTEX_POINT('',#19450);
#4243=VERTEX_POINT('',#19474);
#4244=VERTEX_POINT('',#19475);
#4245=VERTEX_POINT('',#19499);
#4246=VERTEX_POINT('',#19500);
#4247=VERTEX_POINT('',#19523);
#4248=VERTEX_POINT('',#19524);
#4249=VERTEX_POINT('',#19548);
#4250=VERTEX_POINT('',#19549);
#4251=VERTEX_POINT('',#19573);
#4252=VERTEX_POINT('',#19574);
#4253=VERTEX_POINT('',#19597);
#4254=VERTEX_POINT('',#19598);
#4255=VERTEX_POINT('',#19622);
#4256=VERTEX_POINT('',#19623);
#4257=VERTEX_POINT('',#19647);
#4258=VERTEX_POINT('',#19648);
#4259=VERTEX_POINT('',#19671);
#4260=VERTEX_POINT('',#19672);
#4261=VERTEX_POINT('',#19696);
#4262=VERTEX_POINT('',#19697);
#4263=VERTEX_POINT('',#19721);
#4264=VERTEX_POINT('',#19722);
#4265=VERTEX_POINT('',#19745);
#4266=VERTEX_POINT('',#19746);
#4267=VERTEX_POINT('',#19748);
#4268=VERTEX_POINT('',#19754);
#4269=VERTEX_POINT('',#19762);
#4270=VERTEX_POINT('',#19763);
#4271=VERTEX_POINT('',#19765);
#4272=VERTEX_POINT('',#19774);
#4273=VERTEX_POINT('',#19786);
#4274=VERTEX_POINT('',#19787);
#4275=VERTEX_POINT('',#19810);
#4276=VERTEX_POINT('',#19811);
#4277=VERTEX_POINT('',#19835);
#4278=VERTEX_POINT('',#19836);
#4279=VERTEX_POINT('',#19860);
#4280=VERTEX_POINT('',#19861);
#4281=VERTEX_POINT('',#19884);
#4282=VERTEX_POINT('',#19885);
#4283=VERTEX_POINT('',#19909);
#4284=VERTEX_POINT('',#19910);
#4285=VERTEX_POINT('',#19934);
#4286=VERTEX_POINT('',#19935);
#4287=VERTEX_POINT('',#19958);
#4288=VERTEX_POINT('',#19959);
#4289=VERTEX_POINT('',#19983);
#4290=VERTEX_POINT('',#19984);
#4291=VERTEX_POINT('',#20008);
#4292=VERTEX_POINT('',#20009);
#4293=VERTEX_POINT('',#20032);
#4294=VERTEX_POINT('',#20033);
#4295=VERTEX_POINT('',#20057);
#4296=VERTEX_POINT('',#20058);
#4297=VERTEX_POINT('',#20082);
#4298=VERTEX_POINT('',#20083);
#4299=VERTEX_POINT('',#20106);
#4300=VERTEX_POINT('',#20107);
#4301=VERTEX_POINT('',#20109);
#4302=VERTEX_POINT('',#20115);
#4303=VERTEX_POINT('',#20123);
#4304=VERTEX_POINT('',#20124);
#4305=VERTEX_POINT('',#20126);
#4306=VERTEX_POINT('',#20131);
#4307=VERTEX_POINT('',#20133);
#4308=VERTEX_POINT('',#20136);
#4309=VERTEX_POINT('',#20149);
#4310=VERTEX_POINT('',#20150);
#4311=VERTEX_POINT('',#20200);
#4312=VERTEX_POINT('',#20201);
#4313=VERTEX_POINT('',#20251);
#4314=VERTEX_POINT('',#20252);
#4315=VERTEX_POINT('',#20299);
#4316=VERTEX_POINT('',#20300);
#4317=VERTEX_POINT('',#20350);
#4318=VERTEX_POINT('',#20351);
#4319=VERTEX_POINT('',#20401);
#4320=VERTEX_POINT('',#20402);
#4321=VERTEX_POINT('',#20449);
#4322=VERTEX_POINT('',#20450);
#4323=VERTEX_POINT('',#20500);
#4324=VERTEX_POINT('',#20501);
#4325=VERTEX_POINT('',#20551);
#4326=VERTEX_POINT('',#20552);
#4327=VERTEX_POINT('',#20599);
#4328=VERTEX_POINT('',#20600);
#4329=VERTEX_POINT('',#20650);
#4330=VERTEX_POINT('',#20651);
#4331=VERTEX_POINT('',#20701);
#4332=VERTEX_POINT('',#20702);
#4333=VERTEX_POINT('',#20749);
#4334=VERTEX_POINT('',#20750);
#4335=VERTEX_POINT('',#20800);
#4336=VERTEX_POINT('',#20801);
#4337=VERTEX_POINT('',#20803);
#4338=VERTEX_POINT('',#20817);
#4339=VERTEX_POINT('',#20839);
#4340=VERTEX_POINT('',#20840);
#4341=VERTEX_POINT('',#20842);
#4342=VERTEX_POINT('',#20851);
#4343=VERTEX_POINT('',#20863);
#4344=VERTEX_POINT('',#20864);
#4345=VERTEX_POINT('',#20887);
#4346=VERTEX_POINT('',#20888);
#4347=VERTEX_POINT('',#20912);
#4348=VERTEX_POINT('',#20913);
#4349=VERTEX_POINT('',#20937);
#4350=VERTEX_POINT('',#20938);
#4351=VERTEX_POINT('',#20961);
#4352=VERTEX_POINT('',#20962);
#4353=VERTEX_POINT('',#20986);
#4354=VERTEX_POINT('',#20987);
#4355=VERTEX_POINT('',#21011);
#4356=VERTEX_POINT('',#21012);
#4357=VERTEX_POINT('',#21035);
#4358=VERTEX_POINT('',#21036);
#4359=VERTEX_POINT('',#21060);
#4360=VERTEX_POINT('',#21061);
#4361=VERTEX_POINT('',#21085);
#4362=VERTEX_POINT('',#21086);
#4363=VERTEX_POINT('',#21109);
#4364=VERTEX_POINT('',#21110);
#4365=VERTEX_POINT('',#21134);
#4366=VERTEX_POINT('',#21135);
#4367=VERTEX_POINT('',#21159);
#4368=VERTEX_POINT('',#21160);
#4369=VERTEX_POINT('',#21183);
#4370=VERTEX_POINT('',#21184);
#4371=VERTEX_POINT('',#21186);
#4372=VERTEX_POINT('',#21192);
#4373=VERTEX_POINT('',#21200);
#4374=VERTEX_POINT('',#21201);
#4375=VERTEX_POINT('',#21203);
#4376=VERTEX_POINT('',#21208);
#4377=VERTEX_POINT('',#21210);
#4378=VERTEX_POINT('',#21213);
#4379=VERTEX_POINT('',#21226);
#4380=VERTEX_POINT('',#21227);
#4381=VERTEX_POINT('',#21277);
#4382=VERTEX_POINT('',#21278);
#4383=VERTEX_POINT('',#21328);
#4384=VERTEX_POINT('',#21329);
#4385=VERTEX_POINT('',#21376);
#4386=VERTEX_POINT('',#21377);
#4387=VERTEX_POINT('',#21427);
#4388=VERTEX_POINT('',#21428);
#4389=VERTEX_POINT('',#21478);
#4390=VERTEX_POINT('',#21479);
#4391=VERTEX_POINT('',#21526);
#4392=VERTEX_POINT('',#21527);
#4393=VERTEX_POINT('',#21577);
#4394=VERTEX_POINT('',#21578);
#4395=VERTEX_POINT('',#21628);
#4396=VERTEX_POINT('',#21629);
#4397=VERTEX_POINT('',#21676);
#4398=VERTEX_POINT('',#21677);
#4399=VERTEX_POINT('',#21727);
#4400=VERTEX_POINT('',#21728);
#4401=VERTEX_POINT('',#21778);
#4402=VERTEX_POINT('',#21779);
#4403=VERTEX_POINT('',#21826);
#4404=VERTEX_POINT('',#21827);
#4405=VERTEX_POINT('',#21877);
#4406=VERTEX_POINT('',#21878);
#4407=VERTEX_POINT('',#21880);
#4408=VERTEX_POINT('',#21894);
#4409=VERTEX_POINT('',#21916);
#4410=VERTEX_POINT('',#21917);
#4411=VERTEX_POINT('',#21919);
#4412=VERTEX_POINT('',#21928);
#4413=VERTEX_POINT('',#21940);
#4414=VERTEX_POINT('',#21941);
#4415=VERTEX_POINT('',#21964);
#4416=VERTEX_POINT('',#21965);
#4417=VERTEX_POINT('',#21989);
#4418=VERTEX_POINT('',#21990);
#4419=VERTEX_POINT('',#22014);
#4420=VERTEX_POINT('',#22015);
#4421=VERTEX_POINT('',#22038);
#4422=VERTEX_POINT('',#22039);
#4423=VERTEX_POINT('',#22063);
#4424=VERTEX_POINT('',#22064);
#4425=VERTEX_POINT('',#22088);
#4426=VERTEX_POINT('',#22089);
#4427=VERTEX_POINT('',#22112);
#4428=VERTEX_POINT('',#22113);
#4429=VERTEX_POINT('',#22137);
#4430=VERTEX_POINT('',#22138);
#4431=VERTEX_POINT('',#22162);
#4432=VERTEX_POINT('',#22163);
#4433=VERTEX_POINT('',#22186);
#4434=VERTEX_POINT('',#22187);
#4435=VERTEX_POINT('',#22211);
#4436=VERTEX_POINT('',#22212);
#4437=VERTEX_POINT('',#22236);
#4438=VERTEX_POINT('',#22237);
#4439=VERTEX_POINT('',#22260);
#4440=VERTEX_POINT('',#22261);
#4441=VERTEX_POINT('',#22263);
#4442=VERTEX_POINT('',#22269);
#4443=VERTEX_POINT('',#22277);
#4444=VERTEX_POINT('',#22278);
#4445=VERTEX_POINT('',#22280);
#4446=VERTEX_POINT('',#22306);
#4447=VERTEX_POINT('',#22346);
#4448=VERTEX_POINT('',#22347);
#4449=VERTEX_POINT('',#22436);
#4450=VERTEX_POINT('',#22437);
#4451=VERTEX_POINT('',#22523);
#4452=VERTEX_POINT('',#22524);
#4453=VERTEX_POINT('',#22613);
#4454=VERTEX_POINT('',#22614);
#4455=VERTEX_POINT('',#22700);
#4456=VERTEX_POINT('',#22701);
#4457=VERTEX_POINT('',#22790);
#4458=VERTEX_POINT('',#22791);
#4459=VERTEX_POINT('',#22877);
#4460=VERTEX_POINT('',#22878);
#4461=VERTEX_POINT('',#22880);
#4462=VERTEX_POINT('',#22888);
#4463=VERTEX_POINT('',#22910);
#4464=VERTEX_POINT('',#22911);
#4465=VERTEX_POINT('',#22913);
#4466=VERTEX_POINT('',#22927);
#4467=VERTEX_POINT('',#22944);
#4468=VERTEX_POINT('',#22945);
#4469=VERTEX_POINT('',#22980);
#4470=VERTEX_POINT('',#22981);
#4471=VERTEX_POINT('',#23018);
#4472=VERTEX_POINT('',#23019);
#4473=VERTEX_POINT('',#23056);
#4474=VERTEX_POINT('',#23057);
#4475=VERTEX_POINT('',#23093);
#4476=VERTEX_POINT('',#23094);
#4477=VERTEX_POINT('',#23130);
#4478=VERTEX_POINT('',#23131);
#4479=VERTEX_POINT('',#23168);
#4480=VERTEX_POINT('',#23169);
#4481=VERTEX_POINT('',#23171);
#4482=VERTEX_POINT('',#23178);
#4483=VERTEX_POINT('',#24644);
#4484=VERTEX_POINT('',#24648);
#4485=VERTEX_POINT('',#24652);
#4486=VERTEX_POINT('',#24653);
#4487=VERTEX_POINT('',#24655);
#4488=VERTEX_POINT('',#24657);
#4489=VERTEX_POINT('',#27519);
#4490=VERTEX_POINT('',#27553);
#4491=VERTEX_POINT('',#28591);
#4492=VERTEX_POINT('',#28613);
#4493=VERTEX_POINT('',#28647);
#4494=VERTEX_POINT('',#29685);
#4495=VERTEX_POINT('',#34687);
#4496=VERTEX_POINT('',#34689);
#4497=VERTEX_POINT('',#34693);
#4498=VERTEX_POINT('',#34695);
#4499=VERTEX_POINT('',#34699);
#4500=VERTEX_POINT('',#34701);
#4501=VERTEX_POINT('',#34705);
#4502=VERTEX_POINT('',#34707);
#4503=VERTEX_POINT('',#34711);
#4504=VERTEX_POINT('',#34713);
#4505=VERTEX_POINT('',#34717);
#4506=VERTEX_POINT('',#34719);
#4507=VERTEX_POINT('',#34723);
#4508=VERTEX_POINT('',#34725);
#4509=VERTEX_POINT('',#34729);
#4510=VERTEX_POINT('',#34731);
#4511=VERTEX_POINT('',#34735);
#4512=VERTEX_POINT('',#34738);
#4513=VERTEX_POINT('',#34742);
#4514=VERTEX_POINT('',#34744);
#4515=VERTEX_POINT('',#34748);
#4516=VERTEX_POINT('',#34750);
#4517=VERTEX_POINT('',#34754);
#4518=VERTEX_POINT('',#34756);
#4519=VERTEX_POINT('',#34760);
#4520=VERTEX_POINT('',#34762);
#4521=VERTEX_POINT('',#34766);
#4522=VERTEX_POINT('',#34768);
#4523=VERTEX_POINT('',#34772);
#4524=VERTEX_POINT('',#34774);
#4525=VERTEX_POINT('',#34778);
#4526=VERTEX_POINT('',#34780);
#4527=VERTEX_POINT('',#34784);
#4528=VERTEX_POINT('',#34787);
#4529=VERTEX_POINT('',#34791);
#4530=VERTEX_POINT('',#34793);
#4531=VERTEX_POINT('',#34797);
#4532=VERTEX_POINT('',#34798);
#4533=VERTEX_POINT('',#34800);
#4534=VERTEX_POINT('',#34802);
#4535=VERTEX_POINT('',#34806);
#4536=VERTEX_POINT('',#34808);
#4537=VERTEX_POINT('',#34812);
#4538=VERTEX_POINT('',#34814);
#4539=VERTEX_POINT('',#34822);
#4540=VERTEX_POINT('',#34824);
#4541=VERTEX_POINT('',#34828);
#4542=VERTEX_POINT('',#34832);
#4543=VERTEX_POINT('',#34840);
#4544=VERTEX_POINT('',#34842);
#4545=VERTEX_POINT('',#34846);
#4546=VERTEX_POINT('',#34848);
#4547=VERTEX_POINT('',#34852);
#4548=VERTEX_POINT('',#34854);
#4549=VERTEX_POINT('',#34858);
#4550=VERTEX_POINT('',#34860);
#4551=VERTEX_POINT('',#34864);
#4552=VERTEX_POINT('',#34865);
#4553=VERTEX_POINT('',#34867);
#4554=VERTEX_POINT('',#34869);
#4555=VERTEX_POINT('',#34873);
#4556=VERTEX_POINT('',#34875);
#4557=VERTEX_POINT('',#34879);
#4558=VERTEX_POINT('',#34881);
#4559=VERTEX_POINT('',#34891);
#4560=VERTEX_POINT('',#34893);
#4561=VERTEX_POINT('',#34897);
#4562=VERTEX_POINT('',#34899);
#4563=VERTEX_POINT('',#34903);
#4564=VERTEX_POINT('',#34905);
#4565=VERTEX_POINT('',#34909);
#4566=VERTEX_POINT('',#34911);
#4567=VERTEX_POINT('',#34915);
#4568=VERTEX_POINT('',#34916);
#4569=VERTEX_POINT('',#34918);
#4570=VERTEX_POINT('',#34920);
#4571=VERTEX_POINT('',#34924);
#4572=VERTEX_POINT('',#34926);
#4573=VERTEX_POINT('',#34930);
#4574=VERTEX_POINT('',#34932);
#4575=VERTEX_POINT('',#34939);
#4576=VERTEX_POINT('',#34940);
#4577=VERTEX_POINT('',#34942);
#4578=VERTEX_POINT('',#34944);
#4579=VERTEX_POINT('',#34948);
#4580=VERTEX_POINT('',#34950);
#4581=VERTEX_POINT('',#34954);
#4582=VERTEX_POINT('',#34956);
#4583=VERTEX_POINT('',#34966);
#4584=VERTEX_POINT('',#34968);
#4585=VERTEX_POINT('',#34972);
#4586=VERTEX_POINT('',#34974);
#4587=VERTEX_POINT('',#34981);
#4588=VERTEX_POINT('',#34983);
#4589=VERTEX_POINT('',#34987);
#4590=VERTEX_POINT('',#34989);
#4591=VERTEX_POINT('',#34993);
#4592=VERTEX_POINT('',#34995);
#4593=VERTEX_POINT('',#34999);
#4594=VERTEX_POINT('',#35001);
#4595=VERTEX_POINT('',#35005);
#4596=VERTEX_POINT('',#35007);
#4597=VERTEX_POINT('',#35011);
#4598=VERTEX_POINT('',#35013);
#4599=VERTEX_POINT('',#35017);
#4600=VERTEX_POINT('',#35019);
#4601=VERTEX_POINT('',#35023);
#4602=VERTEX_POINT('',#35025);
#4603=VERTEX_POINT('',#35029);
#4604=VERTEX_POINT('',#35031);
#4605=VERTEX_POINT('',#35035);
#4606=VERTEX_POINT('',#35037);
#4607=VERTEX_POINT('',#35041);
#4608=VERTEX_POINT('',#35043);
#4609=VERTEX_POINT('',#35047);
#4610=VERTEX_POINT('',#35049);
#4611=VERTEX_POINT('',#35053);
#4612=VERTEX_POINT('',#35055);
#4613=VERTEX_POINT('',#35059);
#4614=VERTEX_POINT('',#35061);
#4615=VERTEX_POINT('',#35065);
#4616=VERTEX_POINT('',#35067);
#4617=VERTEX_POINT('',#35071);
#4618=VERTEX_POINT('',#35073);
#4619=VERTEX_POINT('',#35077);
#4620=VERTEX_POINT('',#35079);
#4621=VERTEX_POINT('',#35083);
#4622=VERTEX_POINT('',#35085);
#4623=VERTEX_POINT('',#35089);
#4624=VERTEX_POINT('',#35090);
#4625=VERTEX_POINT('',#35092);
#4626=VERTEX_POINT('',#35094);
#4627=VERTEX_POINT('',#35098);
#4628=VERTEX_POINT('',#35100);
#4629=VERTEX_POINT('',#35104);
#4630=VERTEX_POINT('',#35106);
#4631=VERTEX_POINT('',#35116);
#4632=VERTEX_POINT('',#35118);
#4633=VERTEX_POINT('',#35122);
#4634=VERTEX_POINT('',#35124);
#4635=VERTEX_POINT('',#35128);
#4636=VERTEX_POINT('',#35130);
#4637=VERTEX_POINT('',#35134);
#4638=VERTEX_POINT('',#35136);
#4639=VERTEX_POINT('',#35140);
#4640=VERTEX_POINT('',#35142);
#4641=VERTEX_POINT('',#35146);
#4642=VERTEX_POINT('',#35148);
#4643=VERTEX_POINT('',#35152);
#4644=VERTEX_POINT('',#35154);
#4645=VERTEX_POINT('',#35158);
#4646=VERTEX_POINT('',#35159);
#4647=VERTEX_POINT('',#35161);
#4648=VERTEX_POINT('',#35163);
#4649=VERTEX_POINT('',#35167);
#4650=VERTEX_POINT('',#35169);
#4651=VERTEX_POINT('',#35173);
#4652=VERTEX_POINT('',#35175);
#4653=VERTEX_POINT('',#35185);
#4654=VERTEX_POINT('',#35186);
#4655=VERTEX_POINT('',#35188);
#4656=VERTEX_POINT('',#35199);
#4657=VERTEX_POINT('',#35209);
#4658=VERTEX_POINT('',#35210);
#4659=VERTEX_POINT('',#35257);
#4660=VERTEX_POINT('',#35258);
#4661=VERTEX_POINT('',#35305);
#4662=VERTEX_POINT('',#35306);
#4663=VERTEX_POINT('',#35359);
#4664=VERTEX_POINT('',#35360);
#4665=VERTEX_POINT('',#35407);
#4666=VERTEX_POINT('',#35408);
#4667=VERTEX_POINT('',#35455);
#4668=VERTEX_POINT('',#35456);
#4669=VERTEX_POINT('',#35503);
#4670=VERTEX_POINT('',#35504);
#4671=VERTEX_POINT('',#35557);
#4672=VERTEX_POINT('',#35558);
#4673=VERTEX_POINT('',#35605);
#4674=VERTEX_POINT('',#35606);
#4675=VERTEX_POINT('',#35653);
#4676=VERTEX_POINT('',#35654);
#4677=VERTEX_POINT('',#35707);
#4678=VERTEX_POINT('',#35708);
#4679=VERTEX_POINT('',#35755);
#4680=VERTEX_POINT('',#35756);
#4681=VERTEX_POINT('',#35803);
#4682=VERTEX_POINT('',#35804);
#4683=VERTEX_POINT('',#35854);
#4684=VERTEX_POINT('',#35855);
#4685=VERTEX_POINT('',#35905);
#4686=VERTEX_POINT('',#35906);
#4687=VERTEX_POINT('',#35953);
#4688=VERTEX_POINT('',#35954);
#4689=VERTEX_POINT('',#35956);
#4690=VERTEX_POINT('',#35965);
#4691=VERTEX_POINT('',#35975);
#4692=VERTEX_POINT('',#35976);
#4693=VERTEX_POINT('',#35999);
#4694=VERTEX_POINT('',#36000);
#4695=VERTEX_POINT('',#36023);
#4696=VERTEX_POINT('',#36024);
#4697=VERTEX_POINT('',#36049);
#4698=VERTEX_POINT('',#36050);
#4699=VERTEX_POINT('',#36073);
#4700=VERTEX_POINT('',#36074);
#4701=VERTEX_POINT('',#36097);
#4702=VERTEX_POINT('',#36098);
#4703=VERTEX_POINT('',#36122);
#4704=VERTEX_POINT('',#36123);
#4705=VERTEX_POINT('',#36147);
#4706=VERTEX_POINT('',#36148);
#4707=VERTEX_POINT('',#36171);
#4708=VERTEX_POINT('',#36172);
#4709=VERTEX_POINT('',#36196);
#4710=VERTEX_POINT('',#36197);
#4711=VERTEX_POINT('',#36221);
#4712=VERTEX_POINT('',#36222);
#4713=VERTEX_POINT('',#36245);
#4714=VERTEX_POINT('',#36246);
#4715=VERTEX_POINT('',#36269);
#4716=VERTEX_POINT('',#36270);
#4717=VERTEX_POINT('',#36294);
#4718=VERTEX_POINT('',#36295);
#4719=VERTEX_POINT('',#36319);
#4720=VERTEX_POINT('',#36320);
#4721=VERTEX_POINT('',#36343);
#4722=VERTEX_POINT('',#36471);
#4723=VERTEX_POINT('',#36530);
#4724=VERTEX_POINT('',#36635);
#4725=VERTEX_POINT('',#37062);
#4726=VERTEX_POINT('',#37170);
#4727=VERTEX_POINT('',#37716);
#4728=VERTEX_POINT('',#37717);
#4729=VERTEX_POINT('',#37719);
#4730=VERTEX_POINT('',#37721);
#4731=VERTEX_POINT('',#37725);
#4732=VERTEX_POINT('',#37727);
#4733=VERTEX_POINT('',#37731);
#4734=VERTEX_POINT('',#37733);
#4735=VERTEX_POINT('',#37737);
#4736=VERTEX_POINT('',#37739);
#4737=VERTEX_POINT('',#37743);
#4738=VERTEX_POINT('',#37745);
#4739=VERTEX_POINT('',#37753);
#4740=VERTEX_POINT('',#37756);
#4741=VERTEX_POINT('',#37763);
#4742=VERTEX_POINT('',#37764);
#4743=VERTEX_POINT('',#37766);
#4744=VERTEX_POINT('',#37777);
#4745=VERTEX_POINT('',#37787);
#4746=VERTEX_POINT('',#37788);
#4747=VERTEX_POINT('',#37835);
#4748=VERTEX_POINT('',#37836);
#4749=VERTEX_POINT('',#37883);
#4750=VERTEX_POINT('',#37884);
#4751=VERTEX_POINT('',#37937);
#4752=VERTEX_POINT('',#37938);
#4753=VERTEX_POINT('',#37985);
#4754=VERTEX_POINT('',#37986);
#4755=VERTEX_POINT('',#38033);
#4756=VERTEX_POINT('',#38034);
#4757=VERTEX_POINT('',#38087);
#4758=VERTEX_POINT('',#38088);
#4759=VERTEX_POINT('',#38135);
#4760=VERTEX_POINT('',#38136);
#4761=VERTEX_POINT('',#38186);
#4762=VERTEX_POINT('',#38187);
#4763=VERTEX_POINT('',#38237);
#4764=VERTEX_POINT('',#38238);
#4765=VERTEX_POINT('',#38285);
#4766=VERTEX_POINT('',#38286);
#4767=VERTEX_POINT('',#38288);
#4768=VERTEX_POINT('',#38299);
#4769=VERTEX_POINT('',#38310);
#4770=VERTEX_POINT('',#38311);
#4771=VERTEX_POINT('',#38335);
#4772=VERTEX_POINT('',#38336);
#4773=VERTEX_POINT('',#38359);
#4774=VERTEX_POINT('',#38360);
#4775=VERTEX_POINT('',#38385);
#4776=VERTEX_POINT('',#38386);
#4777=VERTEX_POINT('',#38409);
#4778=VERTEX_POINT('',#38410);
#4779=VERTEX_POINT('',#38434);
#4780=VERTEX_POINT('',#38435);
#4781=VERTEX_POINT('',#38459);
#4782=VERTEX_POINT('',#38460);
#4783=VERTEX_POINT('',#38483);
#4784=VERTEX_POINT('',#38484);
#4785=VERTEX_POINT('',#38508);
#4786=VERTEX_POINT('',#38509);
#4787=VERTEX_POINT('',#38533);
#4788=VERTEX_POINT('',#38534);
#4789=VERTEX_POINT('',#38557);
#4790=VERTEX_POINT('',#38775);
#4791=VERTEX_POINT('',#38837);
#4792=VERTEX_POINT('',#38870);
#4793=VERTEX_POINT('',#39181);
#4794=VERTEX_POINT('',#39298);
#4795=VERTEX_POINT('',#39737);
#4796=VERTEX_POINT('',#39738);
#4797=VERTEX_POINT('',#39740);
#4798=VERTEX_POINT('',#39742);
#4799=VERTEX_POINT('',#39746);
#4800=VERTEX_POINT('',#39748);
#4801=VERTEX_POINT('',#39752);
#4802=VERTEX_POINT('',#39754);
#4803=VERTEX_POINT('',#39758);
#4804=VERTEX_POINT('',#39760);
#4805=VERTEX_POINT('',#39764);
#4806=VERTEX_POINT('',#39766);
#4807=VERTEX_POINT('',#39774);
#4808=VERTEX_POINT('',#39777);
#4809=VERTEX_POINT('',#39784);
#4810=VERTEX_POINT('',#39785);
#4811=VERTEX_POINT('',#39787);
#4812=VERTEX_POINT('',#39804);
#4813=VERTEX_POINT('',#39817);
#4814=VERTEX_POINT('',#39818);
#4815=VERTEX_POINT('',#39901);
#4816=VERTEX_POINT('',#39902);
#4817=VERTEX_POINT('',#39991);
#4818=VERTEX_POINT('',#39992);
#4819=VERTEX_POINT('',#40081);
#4820=VERTEX_POINT('',#40082);
#4821=VERTEX_POINT('',#40165);
#4822=VERTEX_POINT('',#40166);
#4823=VERTEX_POINT('',#40255);
#4824=VERTEX_POINT('',#40256);
#4825=VERTEX_POINT('',#40342);
#4826=VERTEX_POINT('',#40343);
#4827=VERTEX_POINT('',#40429);
#4828=VERTEX_POINT('',#40430);
#4829=VERTEX_POINT('',#40519);
#4830=VERTEX_POINT('',#40520);
#4831=VERTEX_POINT('',#40603);
#4832=VERTEX_POINT('',#40604);
#4833=VERTEX_POINT('',#40606);
#4834=VERTEX_POINT('',#40619);
#4835=VERTEX_POINT('',#40632);
#4836=VERTEX_POINT('',#40633);
#4837=VERTEX_POINT('',#40669);
#4838=VERTEX_POINT('',#40670);
#4839=VERTEX_POINT('',#40707);
#4840=VERTEX_POINT('',#40708);
#4841=VERTEX_POINT('',#40743);
#4842=VERTEX_POINT('',#40744);
#4843=VERTEX_POINT('',#40781);
#4844=VERTEX_POINT('',#40782);
#4845=VERTEX_POINT('',#40818);
#4846=VERTEX_POINT('',#40819);
#4847=VERTEX_POINT('',#40855);
#4848=VERTEX_POINT('',#40856);
#4849=VERTEX_POINT('',#40893);
#4850=VERTEX_POINT('',#40894);
#4851=VERTEX_POINT('',#41429);
#4852=VERTEX_POINT('',#41558);
#4853=VERTEX_POINT('',#41689);
#4854=VERTEX_POINT('',#42203);
#4855=VERTEX_POINT('',#42444);
#4856=VERTEX_POINT('',#42446);
#4857=VERTEX_POINT('',#42449);
#4858=VERTEX_POINT('',#42451);
#4859=VERTEX_POINT('',#42456);
#4860=VERTEX_POINT('',#42460);
#4861=VERTEX_POINT('',#42463);
#4862=VERTEX_POINT('',#42465);
#4863=VERTEX_POINT('',#42470);
#4864=VERTEX_POINT('',#42474);
#4865=VERTEX_POINT('',#42477);
#4866=VERTEX_POINT('',#42479);
#4867=VERTEX_POINT('',#42484);
#4868=VERTEX_POINT('',#42488);
#4869=VERTEX_POINT('',#42492);
#4870=VERTEX_POINT('',#42495);
#4871=VERTEX_POINT('',#42498);
#4872=VERTEX_POINT('',#42503);
#4873=VERTEX_POINT('',#42509);
#4874=VERTEX_POINT('',#42511);
#4875=VERTEX_POINT('',#42515);
#4876=VERTEX_POINT('',#42517);
#4877=EDGE_CURVE('',#3875,#3876,#2799,.T.);
#4878=EDGE_CURVE('',#3876,#3877,#2021,.T.);
#4879=EDGE_CURVE('',#3877,#3878,#1825,.T.);
#4880=EDGE_CURVE('',#3878,#3879,#2022,.T.);
#4881=EDGE_CURVE('',#3879,#3880,#2800,.T.);
#4882=EDGE_CURVE('',#3880,#3880,#1826,.F.);
#4883=EDGE_CURVE('',#3879,#3875,#2023,.T.);
#4884=EDGE_CURVE('',#3881,#3882,#2801,.T.);
#4885=EDGE_CURVE('',#3882,#3876,#2024,.T.);
#4886=EDGE_CURVE('',#3875,#3881,#2025,.T.);
#4887=EDGE_CURVE('',#3883,#3884,#2802,.T.);
#4888=EDGE_CURVE('',#3884,#3882,#2026,.T.);
#4889=EDGE_CURVE('',#3881,#3883,#2027,.T.);
#4890=EDGE_CURVE('',#3885,#3886,#2803,.T.);
#4891=EDGE_CURVE('',#3886,#3884,#2028,.T.);
#4892=EDGE_CURVE('',#3883,#3885,#2029,.T.);
#4893=EDGE_CURVE('',#3887,#3888,#2804,.T.);
#4894=EDGE_CURVE('',#3888,#3886,#2030,.T.);
#4895=EDGE_CURVE('',#3885,#3887,#2031,.T.);
#4896=EDGE_CURVE('',#3889,#3890,#2805,.T.);
#4897=EDGE_CURVE('',#3890,#3888,#2032,.T.);
#4898=EDGE_CURVE('',#3887,#3889,#2033,.T.);
#4899=EDGE_CURVE('',#3891,#3892,#2806,.T.);
#4900=EDGE_CURVE('',#3892,#3890,#2034,.T.);
#4901=EDGE_CURVE('',#3889,#3891,#2035,.T.);
#4902=EDGE_CURVE('',#3893,#3894,#2807,.T.);
#4903=EDGE_CURVE('',#3894,#3892,#2036,.T.);
#4904=EDGE_CURVE('',#3891,#3893,#2037,.T.);
#4905=EDGE_CURVE('',#3895,#3896,#2808,.T.);
#4906=EDGE_CURVE('',#3896,#3894,#2038,.T.);
#4907=EDGE_CURVE('',#3893,#3895,#2039,.T.);
#4908=EDGE_CURVE('',#3897,#3898,#2809,.T.);
#4909=EDGE_CURVE('',#3898,#3896,#2040,.T.);
#4910=EDGE_CURVE('',#3895,#3897,#2041,.T.);
#4911=EDGE_CURVE('',#3899,#3900,#2810,.T.);
#4912=EDGE_CURVE('',#3900,#3898,#2042,.T.);
#4913=EDGE_CURVE('',#3897,#3899,#2043,.T.);
#4914=EDGE_CURVE('',#3901,#3902,#2811,.T.);
#4915=EDGE_CURVE('',#3902,#3900,#2044,.T.);
#4916=EDGE_CURVE('',#3899,#3901,#2045,.T.);
#4917=EDGE_CURVE('',#3903,#3904,#2812,.T.);
#4918=EDGE_CURVE('',#3904,#3902,#2046,.T.);
#4919=EDGE_CURVE('',#3901,#3903,#2047,.T.);
#4920=EDGE_CURVE('',#3905,#3906,#2813,.T.);
#4921=EDGE_CURVE('',#3906,#3904,#2048,.T.);
#4922=EDGE_CURVE('',#3903,#3905,#2049,.T.);
#4923=EDGE_CURVE('',#3907,#3908,#2814,.T.);
#4924=EDGE_CURVE('',#3907,#3909,#2050,.T.);
#4925=EDGE_CURVE('',#3910,#3909,#1827,.T.);
#4926=EDGE_CURVE('',#3910,#3908,#2051,.T.);
#4927=EDGE_CURVE('',#3911,#3912,#2815,.T.);
#4928=EDGE_CURVE('',#3912,#3913,#2052,.T.);
#4929=EDGE_CURVE('',#3914,#3913,#1828,.T.);
#4930=EDGE_CURVE('',#3911,#3914,#2053,.T.);
#4931=EDGE_CURVE('',#3915,#3916,#2816,.T.);
#4932=EDGE_CURVE('',#3916,#3912,#2054,.T.);
#4933=EDGE_CURVE('',#3915,#3911,#2055,.T.);
#4934=EDGE_CURVE('',#3917,#3918,#2817,.T.);
#4935=EDGE_CURVE('',#3918,#3916,#2056,.T.);
#4936=EDGE_CURVE('',#3917,#3915,#2057,.T.);
#4937=EDGE_CURVE('',#3919,#3920,#2818,.T.);
#4938=EDGE_CURVE('',#3920,#3918,#2058,.T.);
#4939=EDGE_CURVE('',#3919,#3917,#2059,.T.);
#4940=EDGE_CURVE('',#3921,#3922,#2819,.T.);
#4941=EDGE_CURVE('',#3922,#3920,#2060,.T.);
#4942=EDGE_CURVE('',#3921,#3919,#2061,.T.);
#4943=EDGE_CURVE('',#3923,#3924,#2820,.T.);
#4944=EDGE_CURVE('',#3924,#3922,#2062,.T.);
#4945=EDGE_CURVE('',#3923,#3921,#2063,.T.);
#4946=EDGE_CURVE('',#3925,#3926,#2821,.T.);
#4947=EDGE_CURVE('',#3926,#3924,#2064,.T.);
#4948=EDGE_CURVE('',#3925,#3923,#2065,.T.);
#4949=EDGE_CURVE('',#3927,#3928,#2822,.T.);
#4950=EDGE_CURVE('',#3928,#3926,#2066,.T.);
#4951=EDGE_CURVE('',#3927,#3925,#2067,.T.);
#4952=EDGE_CURVE('',#3929,#3930,#2823,.T.);
#4953=EDGE_CURVE('',#3930,#3928,#2068,.T.);
#4954=EDGE_CURVE('',#3929,#3927,#2069,.T.);
#4955=EDGE_CURVE('',#3931,#3932,#2824,.T.);
#4956=EDGE_CURVE('',#3932,#3930,#2070,.T.);
#4957=EDGE_CURVE('',#3931,#3929,#2071,.T.);
#4958=EDGE_CURVE('',#3933,#3934,#2825,.T.);
#4959=EDGE_CURVE('',#3934,#3932,#2072,.T.);
#4960=EDGE_CURVE('',#3933,#3931,#2073,.T.);
#4961=EDGE_CURVE('',#3935,#3936,#2826,.T.);
#4962=EDGE_CURVE('',#3936,#3934,#2074,.T.);
#4963=EDGE_CURVE('',#3935,#3933,#2075,.T.);
#4964=EDGE_CURVE('',#3937,#3938,#2827,.T.);
#4965=EDGE_CURVE('',#3938,#3936,#2076,.T.);
#4966=EDGE_CURVE('',#3937,#3935,#2077,.T.);
#4967=EDGE_CURVE('',#3939,#3940,#2828,.T.);
#4968=EDGE_CURVE('',#3940,#3938,#2078,.T.);
#4969=EDGE_CURVE('',#3939,#3937,#2079,.T.);
#4970=EDGE_CURVE('',#3941,#3942,#2829,.T.);
#4971=EDGE_CURVE('',#3942,#3940,#2080,.T.);
#4972=EDGE_CURVE('',#3941,#3939,#2081,.T.);
#4973=EDGE_CURVE('',#3943,#3944,#2830,.T.);
#4974=EDGE_CURVE('',#3945,#3943,#2082,.T.);
#4975=EDGE_CURVE('',#3946,#3945,#1829,.T.);
#4976=EDGE_CURVE('',#3946,#3944,#2083,.T.);
#4977=EDGE_CURVE('',#3947,#3948,#2831,.T.);
#4978=EDGE_CURVE('',#3948,#3949,#2084,.T.);
#4979=EDGE_CURVE('',#3949,#3950,#1830,.T.);
#4980=EDGE_CURVE('',#3950,#3951,#2085,.T.);
#4981=EDGE_CURVE('',#3951,#3952,#2832,.T.);
#4982=EDGE_CURVE('',#3952,#3952,#1831,.F.);
#4983=EDGE_CURVE('',#3951,#3947,#2086,.T.);
#4984=EDGE_CURVE('',#3953,#3954,#2833,.T.);
#4985=EDGE_CURVE('',#3954,#3948,#2087,.T.);
#4986=EDGE_CURVE('',#3947,#3953,#2088,.T.);
#4987=EDGE_CURVE('',#3955,#3956,#2834,.T.);
#4988=EDGE_CURVE('',#3956,#3954,#2089,.T.);
#4989=EDGE_CURVE('',#3953,#3955,#2090,.T.);
#4990=EDGE_CURVE('',#3957,#3958,#2835,.T.);
#4991=EDGE_CURVE('',#3958,#3956,#2091,.T.);
#4992=EDGE_CURVE('',#3955,#3957,#2092,.T.);
#4993=EDGE_CURVE('',#3959,#3960,#2836,.T.);
#4994=EDGE_CURVE('',#3960,#3958,#2093,.T.);
#4995=EDGE_CURVE('',#3957,#3959,#2094,.T.);
#4996=EDGE_CURVE('',#3961,#3962,#2837,.T.);
#4997=EDGE_CURVE('',#3962,#3960,#2095,.T.);
#4998=EDGE_CURVE('',#3959,#3961,#2096,.T.);
#4999=EDGE_CURVE('',#3963,#3964,#2838,.T.);
#5000=EDGE_CURVE('',#3964,#3962,#2097,.T.);
#5001=EDGE_CURVE('',#3961,#3963,#2098,.T.);
#5002=EDGE_CURVE('',#3965,#3966,#2839,.T.);
#5003=EDGE_CURVE('',#3966,#3964,#2099,.T.);
#5004=EDGE_CURVE('',#3963,#3965,#2100,.T.);
#5005=EDGE_CURVE('',#3967,#3968,#2840,.T.);
#5006=EDGE_CURVE('',#3968,#3966,#2101,.T.);
#5007=EDGE_CURVE('',#3965,#3967,#2102,.T.);
#5008=EDGE_CURVE('',#3969,#3970,#2841,.T.);
#5009=EDGE_CURVE('',#3970,#3968,#2103,.T.);
#5010=EDGE_CURVE('',#3967,#3969,#2104,.T.);
#5011=EDGE_CURVE('',#3971,#3972,#2842,.T.);
#5012=EDGE_CURVE('',#3972,#3970,#2105,.T.);
#5013=EDGE_CURVE('',#3969,#3971,#2106,.T.);
#5014=EDGE_CURVE('',#3973,#3974,#2843,.T.);
#5015=EDGE_CURVE('',#3974,#3972,#2107,.T.);
#5016=EDGE_CURVE('',#3971,#3973,#2108,.T.);
#5017=EDGE_CURVE('',#3975,#3976,#2844,.T.);
#5018=EDGE_CURVE('',#3976,#3974,#2109,.T.);
#5019=EDGE_CURVE('',#3973,#3975,#2110,.T.);
#5020=EDGE_CURVE('',#3977,#3978,#2845,.T.);
#5021=EDGE_CURVE('',#3978,#3976,#2111,.T.);
#5022=EDGE_CURVE('',#3975,#3977,#2112,.T.);
#5023=EDGE_CURVE('',#3979,#3980,#2846,.T.);
#5024=EDGE_CURVE('',#3979,#3981,#2113,.T.);
#5025=EDGE_CURVE('',#3982,#3981,#1832,.T.);
#5026=EDGE_CURVE('',#3982,#3980,#2114,.T.);
#5027=EDGE_CURVE('',#3983,#3984,#2847,.T.);
#5028=EDGE_CURVE('',#3984,#3985,#2115,.T.);
#5029=EDGE_CURVE('',#3986,#3985,#1833,.T.);
#5030=EDGE_CURVE('',#3983,#3986,#2116,.T.);
#5031=EDGE_CURVE('',#3987,#3988,#2848,.T.);
#5032=EDGE_CURVE('',#3988,#3984,#2117,.T.);
#5033=EDGE_CURVE('',#3987,#3983,#2118,.T.);
#5034=EDGE_CURVE('',#3989,#3990,#2849,.T.);
#5035=EDGE_CURVE('',#3990,#3988,#2119,.T.);
#5036=EDGE_CURVE('',#3989,#3987,#2120,.T.);
#5037=EDGE_CURVE('',#3991,#3992,#2850,.T.);
#5038=EDGE_CURVE('',#3992,#3990,#2121,.T.);
#5039=EDGE_CURVE('',#3991,#3989,#2122,.T.);
#5040=EDGE_CURVE('',#3993,#3994,#2851,.T.);
#5041=EDGE_CURVE('',#3994,#3992,#2123,.T.);
#5042=EDGE_CURVE('',#3993,#3991,#2124,.T.);
#5043=EDGE_CURVE('',#3995,#3996,#2852,.T.);
#5044=EDGE_CURVE('',#3996,#3994,#2125,.T.);
#5045=EDGE_CURVE('',#3995,#3993,#2126,.T.);
#5046=EDGE_CURVE('',#3997,#3998,#2853,.T.);
#5047=EDGE_CURVE('',#3998,#3996,#2127,.T.);
#5048=EDGE_CURVE('',#3997,#3995,#2128,.T.);
#5049=EDGE_CURVE('',#3999,#4000,#2854,.T.);
#5050=EDGE_CURVE('',#4000,#3998,#2129,.T.);
#5051=EDGE_CURVE('',#3999,#3997,#2130,.T.);
#5052=EDGE_CURVE('',#4001,#4002,#2855,.T.);
#5053=EDGE_CURVE('',#4002,#4000,#2131,.T.);
#5054=EDGE_CURVE('',#4001,#3999,#2132,.T.);
#5055=EDGE_CURVE('',#4003,#4004,#2856,.T.);
#5056=EDGE_CURVE('',#4004,#4002,#2133,.T.);
#5057=EDGE_CURVE('',#4003,#4001,#2134,.T.);
#5058=EDGE_CURVE('',#4005,#4006,#2857,.T.);
#5059=EDGE_CURVE('',#4006,#4004,#2135,.T.);
#5060=EDGE_CURVE('',#4005,#4003,#2136,.T.);
#5061=EDGE_CURVE('',#4007,#4008,#2858,.T.);
#5062=EDGE_CURVE('',#4008,#4006,#2137,.T.);
#5063=EDGE_CURVE('',#4007,#4005,#2138,.T.);
#5064=EDGE_CURVE('',#4009,#4010,#2859,.T.);
#5065=EDGE_CURVE('',#4010,#4008,#2139,.T.);
#5066=EDGE_CURVE('',#4009,#4007,#2140,.T.);
#5067=EDGE_CURVE('',#4011,#4012,#2860,.T.);
#5068=EDGE_CURVE('',#4012,#4010,#2141,.T.);
#5069=EDGE_CURVE('',#4011,#4009,#2142,.T.);
#5070=EDGE_CURVE('',#4013,#4014,#2861,.T.);
#5071=EDGE_CURVE('',#4014,#4012,#2143,.T.);
#5072=EDGE_CURVE('',#4013,#4011,#2144,.T.);
#5073=EDGE_CURVE('',#4015,#4016,#2862,.T.);
#5074=EDGE_CURVE('',#4017,#4015,#2145,.T.);
#5075=EDGE_CURVE('',#4018,#4017,#1834,.T.);
#5076=EDGE_CURVE('',#4018,#4016,#2146,.T.);
#5077=EDGE_CURVE('',#4019,#4020,#2863,.T.);
#5078=EDGE_CURVE('',#4020,#4021,#2147,.T.);
#5079=EDGE_CURVE('',#4021,#4022,#1835,.T.);
#5080=EDGE_CURVE('',#4022,#4023,#2148,.T.);
#5081=EDGE_CURVE('',#4023,#4024,#2864,.T.);
#5082=EDGE_CURVE('',#4024,#4024,#1836,.F.);
#5083=EDGE_CURVE('',#4023,#4019,#2149,.T.);
#5084=EDGE_CURVE('',#4025,#4026,#2865,.T.);
#5085=EDGE_CURVE('',#4026,#4020,#2150,.T.);
#5086=EDGE_CURVE('',#4019,#4025,#2151,.T.);
#5087=EDGE_CURVE('',#4027,#4028,#2866,.T.);
#5088=EDGE_CURVE('',#4028,#4026,#2152,.T.);
#5089=EDGE_CURVE('',#4025,#4027,#2153,.T.);
#5090=EDGE_CURVE('',#4029,#4030,#2867,.T.);
#5091=EDGE_CURVE('',#4030,#4028,#2154,.T.);
#5092=EDGE_CURVE('',#4027,#4029,#2155,.T.);
#5093=EDGE_CURVE('',#4031,#4032,#2868,.T.);
#5094=EDGE_CURVE('',#4032,#4030,#2156,.T.);
#5095=EDGE_CURVE('',#4029,#4031,#2157,.T.);
#5096=EDGE_CURVE('',#4033,#4034,#2869,.T.);
#5097=EDGE_CURVE('',#4034,#4032,#2158,.T.);
#5098=EDGE_CURVE('',#4031,#4033,#2159,.T.);
#5099=EDGE_CURVE('',#4035,#4036,#2870,.T.);
#5100=EDGE_CURVE('',#4036,#4034,#2160,.T.);
#5101=EDGE_CURVE('',#4033,#4035,#2161,.T.);
#5102=EDGE_CURVE('',#4037,#4038,#2871,.T.);
#5103=EDGE_CURVE('',#4038,#4036,#2162,.T.);
#5104=EDGE_CURVE('',#4035,#4037,#2163,.T.);
#5105=EDGE_CURVE('',#4039,#4040,#2872,.T.);
#5106=EDGE_CURVE('',#4040,#4038,#2164,.T.);
#5107=EDGE_CURVE('',#4037,#4039,#2165,.T.);
#5108=EDGE_CURVE('',#4041,#4042,#2873,.T.);
#5109=EDGE_CURVE('',#4042,#4040,#2166,.T.);
#5110=EDGE_CURVE('',#4039,#4041,#2167,.T.);
#5111=EDGE_CURVE('',#4043,#4044,#2874,.T.);
#5112=EDGE_CURVE('',#4044,#4042,#2168,.T.);
#5113=EDGE_CURVE('',#4041,#4043,#2169,.T.);
#5114=EDGE_CURVE('',#4045,#4046,#2875,.T.);
#5115=EDGE_CURVE('',#4046,#4044,#2170,.T.);
#5116=EDGE_CURVE('',#4043,#4045,#2171,.T.);
#5117=EDGE_CURVE('',#4047,#4048,#2876,.T.);
#5118=EDGE_CURVE('',#4048,#4046,#2172,.T.);
#5119=EDGE_CURVE('',#4045,#4047,#2173,.T.);
#5120=EDGE_CURVE('',#4049,#4050,#2877,.T.);
#5121=EDGE_CURVE('',#4050,#4048,#2174,.T.);
#5122=EDGE_CURVE('',#4047,#4049,#2175,.T.);
#5123=EDGE_CURVE('',#4051,#4052,#2878,.T.);
#5124=EDGE_CURVE('',#4051,#4053,#2176,.T.);
#5125=EDGE_CURVE('',#4054,#4053,#1837,.T.);
#5126=EDGE_CURVE('',#4054,#4052,#2177,.T.);
#5127=EDGE_CURVE('',#4055,#4056,#2879,.T.);
#5128=EDGE_CURVE('',#4056,#4057,#2178,.T.);
#5129=EDGE_CURVE('',#4058,#4057,#1838,.T.);
#5130=EDGE_CURVE('',#4055,#4058,#2179,.T.);
#5131=EDGE_CURVE('',#4059,#4060,#2880,.T.);
#5132=EDGE_CURVE('',#4060,#4056,#2180,.T.);
#5133=EDGE_CURVE('',#4059,#4055,#2181,.T.);
#5134=EDGE_CURVE('',#4061,#4062,#2881,.T.);
#5135=EDGE_CURVE('',#4062,#4060,#2182,.T.);
#5136=EDGE_CURVE('',#4061,#4059,#2183,.T.);
#5137=EDGE_CURVE('',#4063,#4064,#2882,.T.);
#5138=EDGE_CURVE('',#4064,#4062,#2184,.T.);
#5139=EDGE_CURVE('',#4063,#4061,#2185,.T.);
#5140=EDGE_CURVE('',#4065,#4066,#2883,.T.);
#5141=EDGE_CURVE('',#4066,#4064,#2186,.T.);
#5142=EDGE_CURVE('',#4065,#4063,#2187,.T.);
#5143=EDGE_CURVE('',#4067,#4068,#2884,.T.);
#5144=EDGE_CURVE('',#4068,#4066,#2188,.T.);
#5145=EDGE_CURVE('',#4067,#4065,#2189,.T.);
#5146=EDGE_CURVE('',#4069,#4070,#2885,.T.);
#5147=EDGE_CURVE('',#4070,#4068,#2190,.T.);
#5148=EDGE_CURVE('',#4069,#4067,#2191,.T.);
#5149=EDGE_CURVE('',#4071,#4072,#2886,.T.);
#5150=EDGE_CURVE('',#4072,#4070,#2192,.T.);
#5151=EDGE_CURVE('',#4071,#4069,#2193,.T.);
#5152=EDGE_CURVE('',#4073,#4074,#2887,.T.);
#5153=EDGE_CURVE('',#4074,#4072,#2194,.T.);
#5154=EDGE_CURVE('',#4073,#4071,#2195,.T.);
#5155=EDGE_CURVE('',#4075,#4076,#2888,.T.);
#5156=EDGE_CURVE('',#4076,#4074,#2196,.T.);
#5157=EDGE_CURVE('',#4075,#4073,#2197,.T.);
#5158=EDGE_CURVE('',#4077,#4078,#2889,.T.);
#5159=EDGE_CURVE('',#4078,#4076,#2198,.T.);
#5160=EDGE_CURVE('',#4077,#4075,#2199,.T.);
#5161=EDGE_CURVE('',#4079,#4080,#2890,.T.);
#5162=EDGE_CURVE('',#4080,#4078,#2200,.T.);
#5163=EDGE_CURVE('',#4079,#4077,#2201,.T.);
#5164=EDGE_CURVE('',#4081,#4082,#2891,.T.);
#5165=EDGE_CURVE('',#4082,#4080,#2202,.T.);
#5166=EDGE_CURVE('',#4081,#4079,#2203,.T.);
#5167=EDGE_CURVE('',#4083,#4084,#2892,.T.);
#5168=EDGE_CURVE('',#4084,#4082,#2204,.T.);
#5169=EDGE_CURVE('',#4083,#4081,#2205,.T.);
#5170=EDGE_CURVE('',#4085,#4086,#2893,.T.);
#5171=EDGE_CURVE('',#4086,#4084,#2206,.T.);
#5172=EDGE_CURVE('',#4085,#4083,#2207,.T.);
#5173=EDGE_CURVE('',#4087,#4088,#2894,.T.);
#5174=EDGE_CURVE('',#4089,#4087,#2208,.T.);
#5175=EDGE_CURVE('',#4090,#4089,#1839,.T.);
#5176=EDGE_CURVE('',#4090,#4088,#2209,.T.);
#5177=EDGE_CURVE('',#4091,#4092,#2895,.T.);
#5178=EDGE_CURVE('',#4092,#4093,#2210,.T.);
#5179=EDGE_CURVE('',#4093,#4094,#1840,.T.);
#5180=EDGE_CURVE('',#4094,#4095,#2211,.T.);
#5181=EDGE_CURVE('',#4095,#4096,#2896,.T.);
#5182=EDGE_CURVE('',#4096,#4096,#1841,.F.);
#5183=EDGE_CURVE('',#4095,#4091,#2212,.T.);
#5184=EDGE_CURVE('',#4097,#4098,#2897,.T.);
#5185=EDGE_CURVE('',#4098,#4092,#2213,.T.);
#5186=EDGE_CURVE('',#4091,#4097,#2214,.T.);
#5187=EDGE_CURVE('',#4099,#4100,#2898,.T.);
#5188=EDGE_CURVE('',#4100,#4098,#2215,.T.);
#5189=EDGE_CURVE('',#4097,#4099,#2216,.T.);
#5190=EDGE_CURVE('',#4101,#4102,#2899,.T.);
#5191=EDGE_CURVE('',#4102,#4100,#2217,.T.);
#5192=EDGE_CURVE('',#4099,#4101,#2218,.T.);
#5193=EDGE_CURVE('',#4103,#4104,#2900,.T.);
#5194=EDGE_CURVE('',#4104,#4102,#2219,.T.);
#5195=EDGE_CURVE('',#4101,#4103,#2220,.T.);
#5196=EDGE_CURVE('',#4105,#4106,#2901,.T.);
#5197=EDGE_CURVE('',#4106,#4104,#2221,.T.);
#5198=EDGE_CURVE('',#4103,#4105,#2222,.T.);
#5199=EDGE_CURVE('',#4107,#4108,#2902,.T.);
#5200=EDGE_CURVE('',#4108,#4106,#2223,.T.);
#5201=EDGE_CURVE('',#4105,#4107,#2224,.T.);
#5202=EDGE_CURVE('',#4109,#4110,#2903,.T.);
#5203=EDGE_CURVE('',#4110,#4108,#2225,.T.);
#5204=EDGE_CURVE('',#4107,#4109,#2226,.T.);
#5205=EDGE_CURVE('',#4111,#4112,#2904,.T.);
#5206=EDGE_CURVE('',#4112,#4110,#2227,.T.);
#5207=EDGE_CURVE('',#4109,#4111,#2228,.T.);
#5208=EDGE_CURVE('',#4113,#4114,#2905,.T.);
#5209=EDGE_CURVE('',#4114,#4112,#2229,.T.);
#5210=EDGE_CURVE('',#4111,#4113,#2230,.T.);
#5211=EDGE_CURVE('',#4115,#4116,#2906,.T.);
#5212=EDGE_CURVE('',#4116,#4114,#2231,.T.);
#5213=EDGE_CURVE('',#4113,#4115,#2232,.T.);
#5214=EDGE_CURVE('',#4117,#4118,#2907,.T.);
#5215=EDGE_CURVE('',#4118,#4116,#2233,.T.);
#5216=EDGE_CURVE('',#4115,#4117,#2234,.T.);
#5217=EDGE_CURVE('',#4119,#4120,#2908,.T.);
#5218=EDGE_CURVE('',#4120,#4118,#2235,.T.);
#5219=EDGE_CURVE('',#4117,#4119,#2236,.T.);
#5220=EDGE_CURVE('',#4121,#4122,#2909,.T.);
#5221=EDGE_CURVE('',#4122,#4120,#2237,.T.);
#5222=EDGE_CURVE('',#4119,#4121,#2238,.T.);
#5223=EDGE_CURVE('',#4123,#4124,#2910,.T.);
#5224=EDGE_CURVE('',#4123,#4125,#2239,.T.);
#5225=EDGE_CURVE('',#4126,#4125,#1842,.T.);
#5226=EDGE_CURVE('',#4126,#4124,#2240,.T.);
#5227=EDGE_CURVE('',#4127,#4128,#2911,.T.);
#5228=EDGE_CURVE('',#4128,#4129,#2241,.T.);
#5229=EDGE_CURVE('',#4130,#4129,#1843,.T.);
#5230=EDGE_CURVE('',#4127,#4130,#2242,.T.);
#5231=EDGE_CURVE('',#4131,#4132,#2912,.T.);
#5232=EDGE_CURVE('',#4132,#4128,#2243,.T.);
#5233=EDGE_CURVE('',#4131,#4127,#2244,.T.);
#5234=EDGE_CURVE('',#4133,#4134,#2913,.T.);
#5235=EDGE_CURVE('',#4134,#4132,#2245,.T.);
#5236=EDGE_CURVE('',#4133,#4131,#2246,.T.);
#5237=EDGE_CURVE('',#4135,#4136,#2914,.T.);
#5238=EDGE_CURVE('',#4136,#4134,#2247,.T.);
#5239=EDGE_CURVE('',#4135,#4133,#2248,.T.);
#5240=EDGE_CURVE('',#4137,#4138,#2915,.T.);
#5241=EDGE_CURVE('',#4138,#4136,#2249,.T.);
#5242=EDGE_CURVE('',#4137,#4135,#2250,.T.);
#5243=EDGE_CURVE('',#4139,#4140,#2916,.T.);
#5244=EDGE_CURVE('',#4140,#4138,#2251,.T.);
#5245=EDGE_CURVE('',#4139,#4137,#2252,.T.);
#5246=EDGE_CURVE('',#4141,#4142,#2917,.T.);
#5247=EDGE_CURVE('',#4142,#4140,#2253,.T.);
#5248=EDGE_CURVE('',#4141,#4139,#2254,.T.);
#5249=EDGE_CURVE('',#4143,#4144,#2918,.T.);
#5250=EDGE_CURVE('',#4144,#4142,#2255,.T.);
#5251=EDGE_CURVE('',#4143,#4141,#2256,.T.);
#5252=EDGE_CURVE('',#4145,#4146,#2919,.T.);
#5253=EDGE_CURVE('',#4146,#4144,#2257,.T.);
#5254=EDGE_CURVE('',#4145,#4143,#2258,.T.);
#5255=EDGE_CURVE('',#4147,#4148,#2920,.T.);
#5256=EDGE_CURVE('',#4148,#4146,#2259,.T.);
#5257=EDGE_CURVE('',#4147,#4145,#2260,.T.);
#5258=EDGE_CURVE('',#4149,#4150,#2921,.T.);
#5259=EDGE_CURVE('',#4150,#4148,#2261,.T.);
#5260=EDGE_CURVE('',#4149,#4147,#2262,.T.);
#5261=EDGE_CURVE('',#4151,#4152,#2922,.T.);
#5262=EDGE_CURVE('',#4152,#4150,#2263,.T.);
#5263=EDGE_CURVE('',#4151,#4149,#2264,.T.);
#5264=EDGE_CURVE('',#4153,#4154,#2923,.T.);
#5265=EDGE_CURVE('',#4154,#4152,#2265,.T.);
#5266=EDGE_CURVE('',#4153,#4151,#2266,.T.);
#5267=EDGE_CURVE('',#4155,#4156,#2924,.T.);
#5268=EDGE_CURVE('',#4156,#4154,#2267,.T.);
#5269=EDGE_CURVE('',#4155,#4153,#2268,.T.);
#5270=EDGE_CURVE('',#4157,#4158,#2925,.T.);
#5271=EDGE_CURVE('',#4158,#4156,#2269,.T.);
#5272=EDGE_CURVE('',#4157,#4155,#2270,.T.);
#5273=EDGE_CURVE('',#4159,#4160,#2926,.T.);
#5274=EDGE_CURVE('',#4161,#4159,#2271,.T.);
#5275=EDGE_CURVE('',#4162,#4161,#1844,.T.);
#5276=EDGE_CURVE('',#4162,#4160,#2272,.T.);
#5277=EDGE_CURVE('',#4163,#4164,#2927,.T.);
#5278=EDGE_CURVE('',#4164,#4165,#2273,.T.);
#5279=EDGE_CURVE('',#4165,#4166,#1845,.T.);
#5280=EDGE_CURVE('',#4167,#4166,#2274,.F.);
#5281=EDGE_CURVE('',#4167,#4168,#1846,.T.);
#5282=EDGE_CURVE('',#4168,#4163,#2275,.T.);
#5283=EDGE_CURVE('',#4169,#4170,#2928,.T.);
#5284=EDGE_CURVE('',#4170,#4164,#2276,.T.);
#5285=EDGE_CURVE('',#4163,#4169,#2277,.T.);
#5286=EDGE_CURVE('',#4171,#4172,#2929,.T.);
#5287=EDGE_CURVE('',#4172,#4170,#2278,.T.);
#5288=EDGE_CURVE('',#4169,#4171,#2279,.T.);
#5289=EDGE_CURVE('',#4173,#4174,#2930,.T.);
#5290=EDGE_CURVE('',#4174,#4172,#2280,.T.);
#5291=EDGE_CURVE('',#4171,#4173,#2281,.T.);
#5292=EDGE_CURVE('',#4175,#4176,#2931,.T.);
#5293=EDGE_CURVE('',#4176,#4174,#2282,.T.);
#5294=EDGE_CURVE('',#4173,#4175,#2283,.T.);
#5295=EDGE_CURVE('',#4177,#4178,#2932,.T.);
#5296=EDGE_CURVE('',#4178,#4176,#2284,.T.);
#5297=EDGE_CURVE('',#4175,#4177,#2285,.T.);
#5298=EDGE_CURVE('',#4179,#4180,#2933,.T.);
#5299=EDGE_CURVE('',#4180,#4178,#2286,.T.);
#5300=EDGE_CURVE('',#4177,#4179,#2287,.T.);
#5301=EDGE_CURVE('',#4181,#4182,#2934,.T.);
#5302=EDGE_CURVE('',#4182,#4180,#2288,.T.);
#5303=EDGE_CURVE('',#4179,#4181,#2289,.T.);
#5304=EDGE_CURVE('',#4183,#4184,#2935,.T.);
#5305=EDGE_CURVE('',#4184,#4182,#2290,.T.);
#5306=EDGE_CURVE('',#4181,#4183,#2291,.T.);
#5307=EDGE_CURVE('',#4185,#4186,#2936,.T.);
#5308=EDGE_CURVE('',#4186,#4184,#2292,.T.);
#5309=EDGE_CURVE('',#4183,#4185,#2293,.T.);
#5310=EDGE_CURVE('',#4187,#4188,#2937,.T.);
#5311=EDGE_CURVE('',#4188,#4186,#2294,.T.);
#5312=EDGE_CURVE('',#4185,#4187,#2295,.T.);
#5313=EDGE_CURVE('',#4189,#4190,#2938,.T.);
#5314=EDGE_CURVE('',#4190,#4188,#2296,.T.);
#5315=EDGE_CURVE('',#4187,#4189,#2297,.T.);
#5316=EDGE_CURVE('',#4191,#4192,#2939,.T.);
#5317=EDGE_CURVE('',#4192,#4190,#2298,.T.);
#5318=EDGE_CURVE('',#4189,#4191,#2299,.T.);
#5319=EDGE_CURVE('',#4193,#4194,#2940,.T.);
#5320=EDGE_CURVE('',#4194,#4192,#2300,.T.);
#5321=EDGE_CURVE('',#4191,#4193,#2301,.T.);
#5322=EDGE_CURVE('',#4195,#4196,#2941,.T.);
#5323=EDGE_CURVE('',#4195,#4197,#2302,.T.);
#5324=EDGE_CURVE('',#4198,#4197,#1847,.F.);
#5325=EDGE_CURVE('',#4198,#4196,#2303,.T.);
#5326=EDGE_CURVE('',#4199,#4200,#2942,.T.);
#5327=EDGE_CURVE('',#4200,#4201,#2304,.T.);
#5328=EDGE_CURVE('',#4201,#4202,#1848,.T.);
#5329=EDGE_CURVE('',#4203,#4202,#2305,.F.);
#5330=EDGE_CURVE('',#4203,#4204,#1849,.T.);
#5331=EDGE_CURVE('',#4204,#4199,#2306,.T.);
#5332=EDGE_CURVE('',#4205,#4206,#2943,.T.);
#5333=EDGE_CURVE('',#4206,#4200,#2307,.T.);
#5334=EDGE_CURVE('',#4199,#4205,#2308,.T.);
#5335=EDGE_CURVE('',#4207,#4208,#2944,.T.);
#5336=EDGE_CURVE('',#4208,#4206,#2309,.T.);
#5337=EDGE_CURVE('',#4205,#4207,#2310,.T.);
#5338=EDGE_CURVE('',#4209,#4210,#2945,.T.);
#5339=EDGE_CURVE('',#4210,#4208,#2311,.T.);
#5340=EDGE_CURVE('',#4207,#4209,#2312,.T.);
#5341=EDGE_CURVE('',#4211,#4212,#2946,.T.);
#5342=EDGE_CURVE('',#4212,#4210,#2313,.T.);
#5343=EDGE_CURVE('',#4209,#4211,#2314,.T.);
#5344=EDGE_CURVE('',#4213,#4214,#2947,.T.);
#5345=EDGE_CURVE('',#4214,#4212,#2315,.T.);
#5346=EDGE_CURVE('',#4211,#4213,#2316,.T.);
#5347=EDGE_CURVE('',#4215,#4216,#2948,.T.);
#5348=EDGE_CURVE('',#4216,#4214,#2317,.T.);
#5349=EDGE_CURVE('',#4213,#4215,#2318,.T.);
#5350=EDGE_CURVE('',#4217,#4218,#2949,.T.);
#5351=EDGE_CURVE('',#4218,#4216,#2319,.T.);
#5352=EDGE_CURVE('',#4215,#4217,#2320,.T.);
#5353=EDGE_CURVE('',#4219,#4220,#2950,.T.);
#5354=EDGE_CURVE('',#4220,#4218,#2321,.T.);
#5355=EDGE_CURVE('',#4217,#4219,#2322,.T.);
#5356=EDGE_CURVE('',#4221,#4222,#2951,.T.);
#5357=EDGE_CURVE('',#4222,#4220,#2323,.T.);
#5358=EDGE_CURVE('',#4219,#4221,#2324,.T.);
#5359=EDGE_CURVE('',#4223,#4224,#2952,.T.);
#5360=EDGE_CURVE('',#4224,#4222,#2325,.T.);
#5361=EDGE_CURVE('',#4221,#4223,#2326,.T.);
#5362=EDGE_CURVE('',#4225,#4226,#2953,.T.);
#5363=EDGE_CURVE('',#4226,#4224,#2327,.T.);
#5364=EDGE_CURVE('',#4223,#4225,#2328,.T.);
#5365=EDGE_CURVE('',#4227,#4228,#2954,.T.);
#5366=EDGE_CURVE('',#4228,#4226,#2329,.T.);
#5367=EDGE_CURVE('',#4225,#4227,#2330,.T.);
#5368=EDGE_CURVE('',#4229,#4230,#2955,.T.);
#5369=EDGE_CURVE('',#4230,#4228,#2331,.T.);
#5370=EDGE_CURVE('',#4227,#4229,#2332,.T.);
#5371=EDGE_CURVE('',#4231,#4232,#2956,.T.);
#5372=EDGE_CURVE('',#4231,#4233,#2333,.T.);
#5373=EDGE_CURVE('',#4234,#4233,#1850,.F.);
#5374=EDGE_CURVE('',#4234,#4232,#2334,.T.);
#5375=EDGE_CURVE('',#4235,#4236,#2957,.T.);
#5376=EDGE_CURVE('',#4236,#4237,#2335,.T.);
#5377=EDGE_CURVE('',#4238,#4237,#1851,.T.);
#5378=EDGE_CURVE('',#4235,#4238,#2336,.T.);
#5379=EDGE_CURVE('',#4239,#4240,#2958,.T.);
#5380=EDGE_CURVE('',#4240,#4236,#2337,.T.);
#5381=EDGE_CURVE('',#4239,#4235,#2338,.T.);
#5382=EDGE_CURVE('',#4241,#4242,#2959,.T.);
#5383=EDGE_CURVE('',#4242,#4240,#2339,.T.);
#5384=EDGE_CURVE('',#4241,#4239,#2340,.T.);
#5385=EDGE_CURVE('',#4243,#4244,#2960,.T.);
#5386=EDGE_CURVE('',#4244,#4242,#2341,.T.);
#5387=EDGE_CURVE('',#4243,#4241,#2342,.T.);
#5388=EDGE_CURVE('',#4245,#4246,#2961,.T.);
#5389=EDGE_CURVE('',#4246,#4244,#2343,.T.);
#5390=EDGE_CURVE('',#4245,#4243,#2344,.T.);
#5391=EDGE_CURVE('',#4247,#4248,#2962,.T.);
#5392=EDGE_CURVE('',#4248,#4246,#2345,.T.);
#5393=EDGE_CURVE('',#4247,#4245,#2346,.T.);
#5394=EDGE_CURVE('',#4249,#4250,#2963,.T.);
#5395=EDGE_CURVE('',#4250,#4248,#2347,.T.);
#5396=EDGE_CURVE('',#4249,#4247,#2348,.T.);
#5397=EDGE_CURVE('',#4251,#4252,#2964,.T.);
#5398=EDGE_CURVE('',#4252,#4250,#2349,.T.);
#5399=EDGE_CURVE('',#4251,#4249,#2350,.T.);
#5400=EDGE_CURVE('',#4253,#4254,#2965,.T.);
#5401=EDGE_CURVE('',#4254,#4252,#2351,.T.);
#5402=EDGE_CURVE('',#4253,#4251,#2352,.T.);
#5403=EDGE_CURVE('',#4255,#4256,#2966,.T.);
#5404=EDGE_CURVE('',#4256,#4254,#2353,.T.);
#5405=EDGE_CURVE('',#4255,#4253,#2354,.T.);
#5406=EDGE_CURVE('',#4257,#4258,#2967,.T.);
#5407=EDGE_CURVE('',#4258,#4256,#2355,.T.);
#5408=EDGE_CURVE('',#4257,#4255,#2356,.T.);
#5409=EDGE_CURVE('',#4259,#4260,#2968,.T.);
#5410=EDGE_CURVE('',#4260,#4258,#2357,.T.);
#5411=EDGE_CURVE('',#4259,#4257,#2358,.T.);
#5412=EDGE_CURVE('',#4261,#4262,#2969,.T.);
#5413=EDGE_CURVE('',#4262,#4260,#2359,.T.);
#5414=EDGE_CURVE('',#4261,#4259,#2360,.T.);
#5415=EDGE_CURVE('',#4263,#4264,#2970,.T.);
#5416=EDGE_CURVE('',#4264,#4262,#2361,.T.);
#5417=EDGE_CURVE('',#4263,#4261,#2362,.T.);
#5418=EDGE_CURVE('',#4265,#4266,#2971,.T.);
#5419=EDGE_CURVE('',#4267,#4265,#2363,.T.);
#5420=EDGE_CURVE('',#4268,#4267,#1852,.T.);
#5421=EDGE_CURVE('',#4268,#4266,#2364,.T.);
#5422=EDGE_CURVE('',#4269,#4270,#2972,.T.);
#5423=EDGE_CURVE('',#4270,#4271,#2365,.T.);
#5424=EDGE_CURVE('',#4272,#4271,#1853,.T.);
#5425=EDGE_CURVE('',#4269,#4272,#2366,.T.);
#5426=EDGE_CURVE('',#4273,#4274,#2973,.T.);
#5427=EDGE_CURVE('',#4274,#4270,#2367,.T.);
#5428=EDGE_CURVE('',#4273,#4269,#2368,.T.);
#5429=EDGE_CURVE('',#4275,#4276,#2974,.T.);
#5430=EDGE_CURVE('',#4276,#4274,#2369,.T.);
#5431=EDGE_CURVE('',#4275,#4273,#2370,.T.);
#5432=EDGE_CURVE('',#4277,#4278,#2975,.T.);
#5433=EDGE_CURVE('',#4278,#4276,#2371,.T.);
#5434=EDGE_CURVE('',#4277,#4275,#2372,.T.);
#5435=EDGE_CURVE('',#4279,#4280,#2976,.T.);
#5436=EDGE_CURVE('',#4280,#4278,#2373,.T.);
#5437=EDGE_CURVE('',#4279,#4277,#2374,.T.);
#5438=EDGE_CURVE('',#4281,#4282,#2977,.T.);
#5439=EDGE_CURVE('',#4282,#4280,#2375,.T.);
#5440=EDGE_CURVE('',#4281,#4279,#2376,.T.);
#5441=EDGE_CURVE('',#4283,#4284,#2978,.T.);
#5442=EDGE_CURVE('',#4284,#4282,#2377,.T.);
#5443=EDGE_CURVE('',#4283,#4281,#2378,.T.);
#5444=EDGE_CURVE('',#4285,#4286,#2979,.T.);
#5445=EDGE_CURVE('',#4286,#4284,#2379,.T.);
#5446=EDGE_CURVE('',#4285,#4283,#2380,.T.);
#5447=EDGE_CURVE('',#4287,#4288,#2980,.T.);
#5448=EDGE_CURVE('',#4288,#4286,#2381,.T.);
#5449=EDGE_CURVE('',#4287,#4285,#2382,.T.);
#5450=EDGE_CURVE('',#4289,#4290,#2981,.T.);
#5451=EDGE_CURVE('',#4290,#4288,#2383,.T.);
#5452=EDGE_CURVE('',#4289,#4287,#2384,.T.);
#5453=EDGE_CURVE('',#4291,#4292,#2982,.T.);
#5454=EDGE_CURVE('',#4292,#4290,#2385,.T.);
#5455=EDGE_CURVE('',#4291,#4289,#2386,.T.);
#5456=EDGE_CURVE('',#4293,#4294,#2983,.T.);
#5457=EDGE_CURVE('',#4294,#4292,#2387,.T.);
#5458=EDGE_CURVE('',#4293,#4291,#2388,.T.);
#5459=EDGE_CURVE('',#4295,#4296,#2984,.T.);
#5460=EDGE_CURVE('',#4296,#4294,#2389,.T.);
#5461=EDGE_CURVE('',#4295,#4293,#2390,.T.);
#5462=EDGE_CURVE('',#4297,#4298,#2985,.T.);
#5463=EDGE_CURVE('',#4298,#4296,#2391,.T.);
#5464=EDGE_CURVE('',#4297,#4295,#2392,.T.);
#5465=EDGE_CURVE('',#4299,#4300,#2986,.T.);
#5466=EDGE_CURVE('',#4301,#4299,#2393,.T.);
#5467=EDGE_CURVE('',#4302,#4301,#1854,.T.);
#5468=EDGE_CURVE('',#4302,#4300,#2394,.T.);
#5469=EDGE_CURVE('',#4303,#4304,#2987,.T.);
#5470=EDGE_CURVE('',#4304,#4305,#2395,.T.);
#5471=EDGE_CURVE('',#4305,#4306,#1855,.T.);
#5472=EDGE_CURVE('',#4306,#4307,#2988,.T.);
#5473=EDGE_CURVE('',#4307,#4307,#1856,.F.);
#5474=EDGE_CURVE('',#4306,#4308,#1857,.T.);
#5475=EDGE_CURVE('',#4308,#4303,#2396,.T.);
#5476=EDGE_CURVE('',#4309,#4310,#2989,.T.);
#5477=EDGE_CURVE('',#4310,#4304,#2397,.T.);
#5478=EDGE_CURVE('',#4303,#4309,#2398,.T.);
#5479=EDGE_CURVE('',#4311,#4312,#2990,.T.);
#5480=EDGE_CURVE('',#4312,#4310,#2399,.T.);
#5481=EDGE_CURVE('',#4309,#4311,#2400,.T.);
#5482=EDGE_CURVE('',#4313,#4314,#2991,.T.);
#5483=EDGE_CURVE('',#4314,#4312,#2401,.T.);
#5484=EDGE_CURVE('',#4311,#4313,#2402,.T.);
#5485=EDGE_CURVE('',#4315,#4316,#2992,.T.);
#5486=EDGE_CURVE('',#4316,#4314,#2403,.T.);
#5487=EDGE_CURVE('',#4313,#4315,#2404,.T.);
#5488=EDGE_CURVE('',#4317,#4318,#2993,.T.);
#5489=EDGE_CURVE('',#4318,#4316,#2405,.T.);
#5490=EDGE_CURVE('',#4315,#4317,#2406,.T.);
#5491=EDGE_CURVE('',#4319,#4320,#2994,.T.);
#5492=EDGE_CURVE('',#4320,#4318,#2407,.T.);
#5493=EDGE_CURVE('',#4317,#4319,#2408,.T.);
#5494=EDGE_CURVE('',#4321,#4322,#2995,.T.);
#5495=EDGE_CURVE('',#4322,#4320,#2409,.T.);
#5496=EDGE_CURVE('',#4319,#4321,#2410,.T.);
#5497=EDGE_CURVE('',#4323,#4324,#2996,.T.);
#5498=EDGE_CURVE('',#4324,#4322,#2411,.T.);
#5499=EDGE_CURVE('',#4321,#4323,#2412,.T.);
#5500=EDGE_CURVE('',#4325,#4326,#2997,.T.);
#5501=EDGE_CURVE('',#4326,#4324,#2413,.T.);
#5502=EDGE_CURVE('',#4323,#4325,#2414,.T.);
#5503=EDGE_CURVE('',#4327,#4328,#2998,.T.);
#5504=EDGE_CURVE('',#4328,#4326,#2415,.T.);
#5505=EDGE_CURVE('',#4325,#4327,#2416,.T.);
#5506=EDGE_CURVE('',#4329,#4330,#2999,.T.);
#5507=EDGE_CURVE('',#4330,#4328,#2417,.T.);
#5508=EDGE_CURVE('',#4327,#4329,#2418,.T.);
#5509=EDGE_CURVE('',#4331,#4332,#3000,.T.);
#5510=EDGE_CURVE('',#4332,#4330,#2419,.T.);
#5511=EDGE_CURVE('',#4329,#4331,#2420,.T.);
#5512=EDGE_CURVE('',#4333,#4334,#3001,.T.);
#5513=EDGE_CURVE('',#4334,#4332,#2421,.T.);
#5514=EDGE_CURVE('',#4331,#4333,#2422,.T.);
#5515=EDGE_CURVE('',#4335,#4336,#3002,.T.);
#5516=EDGE_CURVE('',#4335,#4337,#2423,.T.);
#5517=EDGE_CURVE('',#4338,#4337,#1858,.F.);
#5518=EDGE_CURVE('',#4338,#4336,#2424,.T.);
#5519=EDGE_CURVE('',#4339,#4340,#3003,.T.);
#5520=EDGE_CURVE('',#4340,#4341,#2425,.T.);
#5521=EDGE_CURVE('',#4342,#4341,#1859,.T.);
#5522=EDGE_CURVE('',#4339,#4342,#2426,.T.);
#5523=EDGE_CURVE('',#4343,#4344,#3004,.T.);
#5524=EDGE_CURVE('',#4344,#4340,#2427,.T.);
#5525=EDGE_CURVE('',#4343,#4339,#2428,.T.);
#5526=EDGE_CURVE('',#4345,#4346,#3005,.T.);
#5527=EDGE_CURVE('',#4346,#4344,#2429,.T.);
#5528=EDGE_CURVE('',#4345,#4343,#2430,.T.);
#5529=EDGE_CURVE('',#4347,#4348,#3006,.T.);
#5530=EDGE_CURVE('',#4348,#4346,#2431,.T.);
#5531=EDGE_CURVE('',#4347,#4345,#2432,.T.);
#5532=EDGE_CURVE('',#4349,#4350,#3007,.T.);
#5533=EDGE_CURVE('',#4350,#4348,#2433,.T.);
#5534=EDGE_CURVE('',#4349,#4347,#2434,.T.);
#5535=EDGE_CURVE('',#4351,#4352,#3008,.T.);
#5536=EDGE_CURVE('',#4352,#4350,#2435,.T.);
#5537=EDGE_CURVE('',#4351,#4349,#2436,.T.);
#5538=EDGE_CURVE('',#4353,#4354,#3009,.T.);
#5539=EDGE_CURVE('',#4354,#4352,#2437,.T.);
#5540=EDGE_CURVE('',#4353,#4351,#2438,.T.);
#5541=EDGE_CURVE('',#4355,#4356,#3010,.T.);
#5542=EDGE_CURVE('',#4356,#4354,#2439,.T.);
#5543=EDGE_CURVE('',#4355,#4353,#2440,.T.);
#5544=EDGE_CURVE('',#4357,#4358,#3011,.T.);
#5545=EDGE_CURVE('',#4358,#4356,#2441,.T.);
#5546=EDGE_CURVE('',#4357,#4355,#2442,.T.);
#5547=EDGE_CURVE('',#4359,#4360,#3012,.T.);
#5548=EDGE_CURVE('',#4360,#4358,#2443,.T.);
#5549=EDGE_CURVE('',#4359,#4357,#2444,.T.);
#5550=EDGE_CURVE('',#4361,#4362,#3013,.T.);
#5551=EDGE_CURVE('',#4362,#4360,#2445,.T.);
#5552=EDGE_CURVE('',#4361,#4359,#2446,.T.);
#5553=EDGE_CURVE('',#4363,#4364,#3014,.T.);
#5554=EDGE_CURVE('',#4364,#4362,#2447,.T.);
#5555=EDGE_CURVE('',#4363,#4361,#2448,.T.);
#5556=EDGE_CURVE('',#4365,#4366,#3015,.T.);
#5557=EDGE_CURVE('',#4366,#4364,#2449,.T.);
#5558=EDGE_CURVE('',#4365,#4363,#2450,.T.);
#5559=EDGE_CURVE('',#4367,#4368,#3016,.T.);
#5560=EDGE_CURVE('',#4368,#4366,#2451,.T.);
#5561=EDGE_CURVE('',#4367,#4365,#2452,.T.);
#5562=EDGE_CURVE('',#4369,#4370,#3017,.T.);
#5563=EDGE_CURVE('',#4371,#4369,#2453,.T.);
#5564=EDGE_CURVE('',#4372,#4371,#1860,.T.);
#5565=EDGE_CURVE('',#4372,#4370,#2454,.T.);
#5566=EDGE_CURVE('',#4373,#4374,#3018,.T.);
#5567=EDGE_CURVE('',#4374,#4375,#2455,.T.);
#5568=EDGE_CURVE('',#4375,#4376,#1861,.T.);
#5569=EDGE_CURVE('',#4376,#4377,#3019,.T.);
#5570=EDGE_CURVE('',#4377,#4377,#1862,.F.);
#5571=EDGE_CURVE('',#4376,#4378,#1863,.T.);
#5572=EDGE_CURVE('',#4378,#4373,#2456,.T.);
#5573=EDGE_CURVE('',#4379,#4380,#3020,.T.);
#5574=EDGE_CURVE('',#4380,#4374,#2457,.T.);
#5575=EDGE_CURVE('',#4373,#4379,#2458,.T.);
#5576=EDGE_CURVE('',#4381,#4382,#3021,.T.);
#5577=EDGE_CURVE('',#4382,#4380,#2459,.T.);
#5578=EDGE_CURVE('',#4379,#4381,#2460,.T.);
#5579=EDGE_CURVE('',#4383,#4384,#3022,.T.);
#5580=EDGE_CURVE('',#4384,#4382,#2461,.T.);
#5581=EDGE_CURVE('',#4381,#4383,#2462,.T.);
#5582=EDGE_CURVE('',#4385,#4386,#3023,.T.);
#5583=EDGE_CURVE('',#4386,#4384,#2463,.T.);
#5584=EDGE_CURVE('',#4383,#4385,#2464,.T.);
#5585=EDGE_CURVE('',#4387,#4388,#3024,.T.);
#5586=EDGE_CURVE('',#4388,#4386,#2465,.T.);
#5587=EDGE_CURVE('',#4385,#4387,#2466,.T.);
#5588=EDGE_CURVE('',#4389,#4390,#3025,.T.);
#5589=EDGE_CURVE('',#4390,#4388,#2467,.T.);
#5590=EDGE_CURVE('',#4387,#4389,#2468,.T.);
#5591=EDGE_CURVE('',#4391,#4392,#3026,.T.);
#5592=EDGE_CURVE('',#4392,#4390,#2469,.T.);
#5593=EDGE_CURVE('',#4389,#4391,#2470,.T.);
#5594=EDGE_CURVE('',#4393,#4394,#3027,.T.);
#5595=EDGE_CURVE('',#4394,#4392,#2471,.T.);
#5596=EDGE_CURVE('',#4391,#4393,#2472,.T.);
#5597=EDGE_CURVE('',#4395,#4396,#3028,.T.);
#5598=EDGE_CURVE('',#4396,#4394,#2473,.T.);
#5599=EDGE_CURVE('',#4393,#4395,#2474,.T.);
#5600=EDGE_CURVE('',#4397,#4398,#3029,.T.);
#5601=EDGE_CURVE('',#4398,#4396,#2475,.T.);
#5602=EDGE_CURVE('',#4395,#4397,#2476,.T.);
#5603=EDGE_CURVE('',#4399,#4400,#3030,.T.);
#5604=EDGE_CURVE('',#4400,#4398,#2477,.T.);
#5605=EDGE_CURVE('',#4397,#4399,#2478,.T.);
#5606=EDGE_CURVE('',#4401,#4402,#3031,.T.);
#5607=EDGE_CURVE('',#4402,#4400,#2479,.T.);
#5608=EDGE_CURVE('',#4399,#4401,#2480,.T.);
#5609=EDGE_CURVE('',#4403,#4404,#3032,.T.);
#5610=EDGE_CURVE('',#4404,#4402,#2481,.T.);
#5611=EDGE_CURVE('',#4401,#4403,#2482,.T.);
#5612=EDGE_CURVE('',#4405,#4406,#3033,.T.);
#5613=EDGE_CURVE('',#4405,#4407,#2483,.T.);
#5614=EDGE_CURVE('',#4408,#4407,#1864,.F.);
#5615=EDGE_CURVE('',#4408,#4406,#2484,.T.);
#5616=EDGE_CURVE('',#4409,#4410,#3034,.T.);
#5617=EDGE_CURVE('',#4410,#4411,#2485,.T.);
#5618=EDGE_CURVE('',#4412,#4411,#1865,.T.);
#5619=EDGE_CURVE('',#4409,#4412,#2486,.T.);
#5620=EDGE_CURVE('',#4413,#4414,#3035,.T.);
#5621=EDGE_CURVE('',#4414,#4410,#2487,.T.);
#5622=EDGE_CURVE('',#4413,#4409,#2488,.T.);
#5623=EDGE_CURVE('',#4415,#4416,#3036,.T.);
#5624=EDGE_CURVE('',#4416,#4414,#2489,.T.);
#5625=EDGE_CURVE('',#4415,#4413,#2490,.T.);
#5626=EDGE_CURVE('',#4417,#4418,#3037,.T.);
#5627=EDGE_CURVE('',#4418,#4416,#2491,.T.);
#5628=EDGE_CURVE('',#4417,#4415,#2492,.T.);
#5629=EDGE_CURVE('',#4419,#4420,#3038,.T.);
#5630=EDGE_CURVE('',#4420,#4418,#2493,.T.);
#5631=EDGE_CURVE('',#4419,#4417,#2494,.T.);
#5632=EDGE_CURVE('',#4421,#4422,#3039,.T.);
#5633=EDGE_CURVE('',#4422,#4420,#2495,.T.);
#5634=EDGE_CURVE('',#4421,#4419,#2496,.T.);
#5635=EDGE_CURVE('',#4423,#4424,#3040,.T.);
#5636=EDGE_CURVE('',#4424,#4422,#2497,.T.);
#5637=EDGE_CURVE('',#4423,#4421,#2498,.T.);
#5638=EDGE_CURVE('',#4425,#4426,#3041,.T.);
#5639=EDGE_CURVE('',#4426,#4424,#2499,.T.);
#5640=EDGE_CURVE('',#4425,#4423,#2500,.T.);
#5641=EDGE_CURVE('',#4427,#4428,#3042,.T.);
#5642=EDGE_CURVE('',#4428,#4426,#2501,.T.);
#5643=EDGE_CURVE('',#4427,#4425,#2502,.T.);
#5644=EDGE_CURVE('',#4429,#4430,#3043,.T.);
#5645=EDGE_CURVE('',#4430,#4428,#2503,.T.);
#5646=EDGE_CURVE('',#4429,#4427,#2504,.T.);
#5647=EDGE_CURVE('',#4431,#4432,#3044,.T.);
#5648=EDGE_CURVE('',#4432,#4430,#2505,.T.);
#5649=EDGE_CURVE('',#4431,#4429,#2506,.T.);
#5650=EDGE_CURVE('',#4433,#4434,#3045,.T.);
#5651=EDGE_CURVE('',#4434,#4432,#2507,.T.);
#5652=EDGE_CURVE('',#4433,#4431,#2508,.T.);
#5653=EDGE_CURVE('',#4435,#4436,#3046,.T.);
#5654=EDGE_CURVE('',#4436,#4434,#2509,.T.);
#5655=EDGE_CURVE('',#4435,#4433,#2510,.T.);
#5656=EDGE_CURVE('',#4437,#4438,#3047,.T.);
#5657=EDGE_CURVE('',#4438,#4436,#2511,.T.);
#5658=EDGE_CURVE('',#4437,#4435,#2512,.T.);
#5659=EDGE_CURVE('',#4439,#4440,#3048,.T.);
#5660=EDGE_CURVE('',#4441,#4439,#2513,.T.);
#5661=EDGE_CURVE('',#4442,#4441,#1866,.T.);
#5662=EDGE_CURVE('',#4442,#4440,#2514,.T.);
#5663=EDGE_CURVE('',#4443,#4444,#3049,.T.);
#5664=EDGE_CURVE('',#4444,#4445,#2515,.T.);
#5665=EDGE_CURVE('',#4445,#4446,#1867,.F.);
#5666=EDGE_CURVE('',#4446,#4443,#2516,.T.);
#5667=EDGE_CURVE('',#4447,#4448,#3050,.T.);
#5668=EDGE_CURVE('',#4448,#4444,#2517,.T.);
#5669=EDGE_CURVE('',#4443,#4447,#2518,.T.);
#5670=EDGE_CURVE('',#4449,#4450,#3051,.T.);
#5671=EDGE_CURVE('',#4450,#4448,#2519,.T.);
#5672=EDGE_CURVE('',#4447,#4449,#2520,.T.);
#5673=EDGE_CURVE('',#4451,#4452,#3052,.T.);
#5674=EDGE_CURVE('',#4452,#4450,#2521,.T.);
#5675=EDGE_CURVE('',#4449,#4451,#2522,.T.);
#5676=EDGE_CURVE('',#4453,#4454,#3053,.T.);
#5677=EDGE_CURVE('',#4454,#4452,#2523,.T.);
#5678=EDGE_CURVE('',#4451,#4453,#2524,.T.);
#5679=EDGE_CURVE('',#4455,#4456,#3054,.T.);
#5680=EDGE_CURVE('',#4456,#4454,#2525,.T.);
#5681=EDGE_CURVE('',#4453,#4455,#2526,.T.);
#5682=EDGE_CURVE('',#4457,#4458,#3055,.T.);
#5683=EDGE_CURVE('',#4458,#4456,#2527,.T.);
#5684=EDGE_CURVE('',#4455,#4457,#2528,.T.);
#5685=EDGE_CURVE('',#4459,#4460,#3056,.T.);
#5686=EDGE_CURVE('',#4459,#4461,#2529,.T.);
#5687=EDGE_CURVE('',#4462,#4461,#1868,.T.);
#5688=EDGE_CURVE('',#4462,#4460,#2530,.T.);
#5689=EDGE_CURVE('',#4463,#4464,#3057,.T.);
#5690=EDGE_CURVE('',#4464,#4465,#2531,.T.);
#5691=EDGE_CURVE('',#4466,#4465,#1869,.T.);
#5692=EDGE_CURVE('',#4463,#4466,#2532,.T.);
#5693=EDGE_CURVE('',#4467,#4468,#3058,.T.);
#5694=EDGE_CURVE('',#4468,#4464,#2533,.T.);
#5695=EDGE_CURVE('',#4467,#4463,#2534,.T.);
#5696=EDGE_CURVE('',#4469,#4470,#3059,.T.);
#5697=EDGE_CURVE('',#4470,#4468,#2535,.T.);
#5698=EDGE_CURVE('',#4469,#4467,#2536,.T.);
#5699=EDGE_CURVE('',#4471,#4472,#3060,.T.);
#5700=EDGE_CURVE('',#4472,#4470,#2537,.T.);
#5701=EDGE_CURVE('',#4471,#4469,#2538,.T.);
#5702=EDGE_CURVE('',#4473,#4474,#3061,.T.);
#5703=EDGE_CURVE('',#4474,#4472,#2539,.T.);
#5704=EDGE_CURVE('',#4473,#4471,#2540,.T.);
#5705=EDGE_CURVE('',#4475,#4476,#3062,.T.);
#5706=EDGE_CURVE('',#4476,#4474,#2541,.T.);
#5707=EDGE_CURVE('',#4475,#4473,#2542,.T.);
#5708=EDGE_CURVE('',#4477,#4478,#3063,.T.);
#5709=EDGE_CURVE('',#4478,#4476,#2543,.T.);
#5710=EDGE_CURVE('',#4477,#4475,#2544,.T.);
#5711=EDGE_CURVE('',#4479,#4480,#3064,.T.);
#5712=EDGE_CURVE('',#4481,#4479,#2545,.T.);
#5713=EDGE_CURVE('',#4482,#4481,#1870,.T.);
#5714=EDGE_CURVE('',#4482,#4480,#2546,.T.);
#5715=EDGE_CURVE('',#4480,#4478,#2547,.T.);
#5716=EDGE_CURVE('',#4479,#4477,#2548,.T.);
#5717=EDGE_CURVE('',#4465,#4462,#2549,.T.);
#5718=EDGE_CURVE('',#4445,#4482,#2550,.T.);
#5719=EDGE_CURVE('',#4460,#4458,#2551,.T.);
#5720=EDGE_CURVE('',#4461,#4466,#2552,.T.);
#5721=EDGE_CURVE('',#4457,#4459,#2553,.T.);
#5722=EDGE_CURVE('',#4481,#4446,#2554,.T.);
#5723=EDGE_CURVE('',#4483,#4483,#1871,.T.);
#5724=EDGE_CURVE('',#4484,#4484,#1872,.T.);
#5725=EDGE_CURVE('',#4484,#4483,#3065,.T.);
#5726=EDGE_CURVE('',#4485,#4486,#3066,.F.);
#5727=EDGE_CURVE('',#4487,#4485,#3067,.F.);
#5728=EDGE_CURVE('',#4488,#4487,#3068,.T.);
#5729=EDGE_CURVE('',#4486,#4488,#3069,.F.);
#5730=EDGE_CURVE('',#4267,#4234,#2555,.T.);
#5731=EDGE_CURVE('',#4233,#4268,#2556,.T.);
#5732=EDGE_CURVE('',#4301,#4198,#2557,.T.);
#5733=EDGE_CURVE('',#4197,#4302,#2558,.T.);
#5734=EDGE_CURVE('',#4371,#4338,#2559,.T.);
#5735=EDGE_CURVE('',#4337,#4372,#2560,.T.);
#5736=EDGE_CURVE('',#4441,#4408,#2561,.T.);
#5737=EDGE_CURVE('',#4407,#4442,#2562,.T.);
#5738=EDGE_CURVE('',#4375,#4412,#2563,.T.);
#5739=EDGE_CURVE('',#4411,#4378,#2564,.T.);
#5740=EDGE_CURVE('',#4440,#4438,#2565,.T.);
#5741=EDGE_CURVE('',#4439,#4437,#2566,.T.);
#5742=EDGE_CURVE('',#4403,#4405,#2567,.T.);
#5743=EDGE_CURVE('',#4406,#4404,#2568,.T.);
#5744=EDGE_CURVE('',#4305,#4342,#2569,.T.);
#5745=EDGE_CURVE('',#4341,#4308,#2570,.T.);
#5746=EDGE_CURVE('',#4370,#4368,#2571,.T.);
#5747=EDGE_CURVE('',#4369,#4367,#2572,.T.);
#5748=EDGE_CURVE('',#4333,#4335,#2573,.T.);
#5749=EDGE_CURVE('',#4336,#4334,#2574,.T.);
#5750=EDGE_CURVE('',#4489,#4167,#3070,.T.);
#5751=EDGE_CURVE('',#4489,#4168,#2575,.T.);
#5752=EDGE_CURVE('',#4166,#4490,#3071,.T.);
#5753=EDGE_CURVE('',#4490,#4272,#2576,.T.);
#5754=EDGE_CURVE('',#4271,#4489,#2577,.T.);
#5755=EDGE_CURVE('',#4489,#4167,#3072,.T.);
#5756=EDGE_CURVE('',#4166,#4167,#1873,.T.);
#5757=EDGE_CURVE('',#4166,#4490,#3073,.T.);
#5758=EDGE_CURVE('',#4165,#4490,#2578,.T.);
#5759=EDGE_CURVE('',#4300,#4298,#2579,.T.);
#5760=EDGE_CURVE('',#4299,#4297,#2580,.T.);
#5761=EDGE_CURVE('',#4193,#4195,#2581,.T.);
#5762=EDGE_CURVE('',#4196,#4194,#2582,.T.);
#5763=EDGE_CURVE('',#4491,#4167,#2583,.F.);
#5764=EDGE_CURVE('',#4166,#4491,#2584,.F.);
#5765=EDGE_CURVE('',#4492,#4203,#3074,.T.);
#5766=EDGE_CURVE('',#4492,#4204,#2585,.T.);
#5767=EDGE_CURVE('',#4202,#4493,#3075,.T.);
#5768=EDGE_CURVE('',#4493,#4238,#2586,.T.);
#5769=EDGE_CURVE('',#4237,#4492,#2587,.T.);
#5770=EDGE_CURVE('',#4492,#4203,#3076,.T.);
#5771=EDGE_CURVE('',#4202,#4203,#1874,.T.);
#5772=EDGE_CURVE('',#4202,#4493,#3077,.T.);
#5773=EDGE_CURVE('',#4201,#4493,#2588,.T.);
#5774=EDGE_CURVE('',#4266,#4264,#2589,.T.);
#5775=EDGE_CURVE('',#4265,#4263,#2590,.T.);
#5776=EDGE_CURVE('',#4229,#4231,#2591,.T.);
#5777=EDGE_CURVE('',#4232,#4230,#2592,.T.);
#5778=EDGE_CURVE('',#4494,#4203,#2593,.F.);
#5779=EDGE_CURVE('',#4202,#4494,#2594,.F.);
#5780=EDGE_CURVE('',#4093,#4130,#2595,.T.);
#5781=EDGE_CURVE('',#4129,#4094,#2596,.T.);
#5782=EDGE_CURVE('',#4160,#4158,#2597,.T.);
#5783=EDGE_CURVE('',#4159,#4157,#2598,.T.);
#5784=EDGE_CURVE('',#4125,#4162,#2599,.T.);
#5785=EDGE_CURVE('',#4121,#4123,#2600,.T.);
#5786=EDGE_CURVE('',#4124,#4122,#2601,.T.);
#5787=EDGE_CURVE('',#4161,#4126,#2602,.T.);
#5788=EDGE_CURVE('',#4021,#4058,#2603,.T.);
#5789=EDGE_CURVE('',#4057,#4022,#2604,.T.);
#5790=EDGE_CURVE('',#4088,#4086,#2605,.T.);
#5791=EDGE_CURVE('',#4087,#4085,#2606,.T.);
#5792=EDGE_CURVE('',#4053,#4090,#2607,.T.);
#5793=EDGE_CURVE('',#4049,#4051,#2608,.T.);
#5794=EDGE_CURVE('',#4052,#4050,#2609,.T.);
#5795=EDGE_CURVE('',#4089,#4054,#2610,.T.);
#5796=EDGE_CURVE('',#3949,#3986,#2611,.T.);
#5797=EDGE_CURVE('',#3985,#3950,#2612,.T.);
#5798=EDGE_CURVE('',#4016,#4014,#2613,.T.);
#5799=EDGE_CURVE('',#4015,#4013,#2614,.T.);
#5800=EDGE_CURVE('',#3981,#4018,#2615,.T.);
#5801=EDGE_CURVE('',#3977,#3979,#2616,.T.);
#5802=EDGE_CURVE('',#3980,#3978,#2617,.T.);
#5803=EDGE_CURVE('',#4017,#3982,#2618,.T.);
#5804=EDGE_CURVE('',#3877,#3914,#2619,.T.);
#5805=EDGE_CURVE('',#3913,#3878,#2620,.T.);
#5806=EDGE_CURVE('',#3944,#3942,#2621,.T.);
#5807=EDGE_CURVE('',#3943,#3941,#2622,.T.);
#5808=EDGE_CURVE('',#3909,#3946,#2623,.T.);
#5809=EDGE_CURVE('',#3905,#3907,#2624,.T.);
#5810=EDGE_CURVE('',#3908,#3906,#2625,.T.);
#5811=EDGE_CURVE('',#3945,#3910,#2626,.T.);
#5812=EDGE_CURVE('',#4495,#4495,#1875,.T.);
#5813=EDGE_CURVE('',#4495,#4496,#3078,.T.);
#5814=EDGE_CURVE('',#4496,#4496,#1876,.T.);
#5815=EDGE_CURVE('',#4497,#4497,#1877,.T.);
#5816=EDGE_CURVE('',#4497,#4498,#3079,.T.);
#5817=EDGE_CURVE('',#4498,#4498,#1878,.T.);
#5818=EDGE_CURVE('',#4499,#4499,#1879,.T.);
#5819=EDGE_CURVE('',#4499,#4500,#3080,.T.);
#5820=EDGE_CURVE('',#4500,#4500,#1880,.T.);
#5821=EDGE_CURVE('',#4501,#4501,#1881,.T.);
#5822=EDGE_CURVE('',#4501,#4502,#3081,.T.);
#5823=EDGE_CURVE('',#4502,#4502,#1882,.T.);
#5824=EDGE_CURVE('',#4503,#4503,#1883,.T.);
#5825=EDGE_CURVE('',#4503,#4504,#3082,.T.);
#5826=EDGE_CURVE('',#4504,#4504,#1884,.T.);
#5827=EDGE_CURVE('',#4505,#4505,#1885,.T.);
#5828=EDGE_CURVE('',#4505,#4506,#3083,.T.);
#5829=EDGE_CURVE('',#4506,#4506,#1886,.T.);
#5830=EDGE_CURVE('',#4507,#4507,#1887,.T.);
#5831=EDGE_CURVE('',#4507,#4508,#3084,.T.);
#5832=EDGE_CURVE('',#4508,#4508,#1888,.T.);
#5833=EDGE_CURVE('',#4509,#4509,#1889,.T.);
#5834=EDGE_CURVE('',#4509,#4510,#3085,.T.);
#5835=EDGE_CURVE('',#4510,#4510,#1890,.T.);
#5836=EDGE_CURVE('',#4511,#4511,#1891,.T.);
#5837=EDGE_CURVE('',#4511,#4493,#3086,.T.);
#5838=EDGE_CURVE('',#4492,#4512,#3087,.T.);
#5839=EDGE_CURVE('',#4512,#4512,#1892,.T.);
#5840=EDGE_CURVE('',#4513,#4513,#1893,.T.);
#5841=EDGE_CURVE('',#4513,#4514,#3088,.T.);
#5842=EDGE_CURVE('',#4514,#4514,#1894,.T.);
#5843=EDGE_CURVE('',#4515,#4515,#1895,.T.);
#5844=EDGE_CURVE('',#4515,#4516,#3089,.T.);
#5845=EDGE_CURVE('',#4516,#4516,#1896,.T.);
#5846=EDGE_CURVE('',#4517,#4517,#1897,.T.);
#5847=EDGE_CURVE('',#4517,#4518,#3090,.T.);
#5848=EDGE_CURVE('',#4518,#4518,#1898,.T.);
#5849=EDGE_CURVE('',#4519,#4519,#1899,.T.);
#5850=EDGE_CURVE('',#4519,#4520,#3091,.T.);
#5851=EDGE_CURVE('',#4520,#4520,#1900,.T.);
#5852=EDGE_CURVE('',#4521,#4521,#1901,.T.);
#5853=EDGE_CURVE('',#4521,#4522,#3092,.T.);
#5854=EDGE_CURVE('',#4522,#4522,#1902,.T.);
#5855=EDGE_CURVE('',#4523,#4523,#1903,.T.);
#5856=EDGE_CURVE('',#4523,#4524,#3093,.T.);
#5857=EDGE_CURVE('',#4524,#4524,#1904,.T.);
#5858=EDGE_CURVE('',#4525,#4525,#1905,.T.);
#5859=EDGE_CURVE('',#4525,#4526,#3094,.T.);
#5860=EDGE_CURVE('',#4526,#4526,#1906,.T.);
#5861=EDGE_CURVE('',#4527,#4527,#1907,.T.);
#5862=EDGE_CURVE('',#4527,#4490,#3095,.T.);
#5863=EDGE_CURVE('',#4489,#4528,#3096,.T.);
#5864=EDGE_CURVE('',#4528,#4528,#1908,.T.);
#5865=EDGE_CURVE('',#4529,#4529,#1909,.T.);
#5866=EDGE_CURVE('',#4529,#4530,#3097,.T.);
#5867=EDGE_CURVE('',#4530,#4530,#1910,.T.);
#5868=EDGE_CURVE('',#4531,#4532,#3098,.T.);
#5869=EDGE_CURVE('',#4531,#4533,#3099,.T.);
#5870=EDGE_CURVE('',#4533,#4534,#3100,.T.);
#5871=EDGE_CURVE('',#4532,#4534,#3101,.T.);
#5872=EDGE_CURVE('',#4535,#4531,#3102,.T.);
#5873=EDGE_CURVE('',#4535,#4536,#3103,.T.);
#5874=EDGE_CURVE('',#4536,#4533,#3104,.T.);
#5875=EDGE_CURVE('',#4537,#4535,#3105,.T.);
#5876=EDGE_CURVE('',#4537,#4538,#3106,.T.);
#5877=EDGE_CURVE('',#4538,#4536,#3107,.T.);
#5878=EDGE_CURVE('',#4532,#4537,#3108,.T.);
#5879=EDGE_CURVE('',#4534,#4538,#3109,.T.);
#5880=EDGE_CURVE('',#4485,#4539,#3110,.T.);
#5881=EDGE_CURVE('',#4540,#4539,#3111,.F.);
#5882=EDGE_CURVE('',#4487,#4540,#3112,.F.);
#5883=EDGE_CURVE('',#4541,#4540,#3113,.T.);
#5884=EDGE_CURVE('',#4488,#4541,#3114,.T.);
#5885=EDGE_CURVE('',#4542,#4541,#3115,.F.);
#5886=EDGE_CURVE('',#4486,#4542,#3116,.F.);
#5887=EDGE_CURVE('',#4539,#4542,#3117,.F.);
#5888=EDGE_CURVE('',#4543,#4543,#1911,.T.);
#5889=EDGE_CURVE('',#4543,#4544,#3118,.T.);
#5890=EDGE_CURVE('',#4544,#4544,#1912,.T.);
#5891=EDGE_CURVE('',#4545,#4545,#1913,.T.);
#5892=EDGE_CURVE('',#4545,#4546,#3119,.T.);
#5893=EDGE_CURVE('',#4546,#4546,#1914,.T.);
#5894=EDGE_CURVE('',#4547,#4547,#1915,.T.);
#5895=EDGE_CURVE('',#4547,#4548,#3120,.T.);
#5896=EDGE_CURVE('',#4548,#4548,#1916,.T.);
#5897=EDGE_CURVE('',#4549,#4549,#1917,.T.);
#5898=EDGE_CURVE('',#4549,#4550,#3121,.T.);
#5899=EDGE_CURVE('',#4550,#4550,#1918,.T.);
#5900=EDGE_CURVE('',#4551,#4552,#3122,.T.);
#5901=EDGE_CURVE('',#4552,#4553,#3123,.T.);
#5902=EDGE_CURVE('',#4554,#4553,#3124,.T.);
#5903=EDGE_CURVE('',#4551,#4554,#3125,.T.);
#5904=EDGE_CURVE('',#4555,#4551,#3126,.T.);
#5905=EDGE_CURVE('',#4556,#4554,#3127,.T.);
#5906=EDGE_CURVE('',#4555,#4556,#3128,.T.);
#5907=EDGE_CURVE('',#4557,#4555,#3129,.T.);
#5908=EDGE_CURVE('',#4558,#4556,#3130,.T.);
#5909=EDGE_CURVE('',#4557,#4558,#3131,.T.);
#5910=EDGE_CURVE('',#4552,#4557,#3132,.T.);
#5911=EDGE_CURVE('',#4553,#4558,#3133,.T.);
#5912=EDGE_CURVE('',#4559,#4559,#1919,.T.);
#5913=EDGE_CURVE('',#4559,#4560,#3134,.T.);
#5914=EDGE_CURVE('',#4560,#4560,#1920,.T.);
#5915=EDGE_CURVE('',#4561,#4561,#1921,.T.);
#5916=EDGE_CURVE('',#4561,#4562,#3135,.T.);
#5917=EDGE_CURVE('',#4562,#4562,#1922,.T.);
#5918=EDGE_CURVE('',#4563,#4563,#1923,.T.);
#5919=EDGE_CURVE('',#4563,#4564,#3136,.T.);
#5920=EDGE_CURVE('',#4564,#4564,#1924,.T.);
#5921=EDGE_CURVE('',#4565,#4565,#1925,.T.);
#5922=EDGE_CURVE('',#4565,#4566,#3137,.T.);
#5923=EDGE_CURVE('',#4566,#4566,#1926,.T.);
#5924=EDGE_CURVE('',#4567,#4568,#3138,.T.);
#5925=EDGE_CURVE('',#4567,#4569,#3139,.T.);
#5926=EDGE_CURVE('',#4570,#4569,#3140,.T.);
#5927=EDGE_CURVE('',#4568,#4570,#3141,.T.);
#5928=EDGE_CURVE('',#4571,#4567,#3142,.T.);
#5929=EDGE_CURVE('',#4571,#4572,#3143,.T.);
#5930=EDGE_CURVE('',#4569,#4572,#3144,.T.);
#5931=EDGE_CURVE('',#4573,#4571,#3145,.T.);
#5932=EDGE_CURVE('',#4573,#4574,#3146,.T.);
#5933=EDGE_CURVE('',#4572,#4574,#3147,.T.);
#5934=EDGE_CURVE('',#4568,#4573,#3148,.T.);
#5935=EDGE_CURVE('',#4574,#4570,#3149,.T.);
#5936=EDGE_CURVE('',#4575,#4576,#3150,.T.);
#5937=EDGE_CURVE('',#4576,#4577,#3151,.T.);
#5938=EDGE_CURVE('',#4578,#4577,#3152,.T.);
#5939=EDGE_CURVE('',#4575,#4578,#3153,.T.);
#5940=EDGE_CURVE('',#4579,#4575,#3154,.T.);
#5941=EDGE_CURVE('',#4580,#4578,#3155,.T.);
#5942=EDGE_CURVE('',#4579,#4580,#3156,.T.);
#5943=EDGE_CURVE('',#4581,#4579,#3157,.T.);
#5944=EDGE_CURVE('',#4582,#4580,#3158,.T.);
#5945=EDGE_CURVE('',#4581,#4582,#3159,.T.);
#5946=EDGE_CURVE('',#4576,#4581,#3160,.T.);
#5947=EDGE_CURVE('',#4577,#4582,#3161,.T.);
#5948=EDGE_CURVE('',#4583,#4583,#1927,.T.);
#5949=EDGE_CURVE('',#4583,#4584,#3162,.T.);
#5950=EDGE_CURVE('',#4584,#4584,#1928,.T.);
#5951=EDGE_CURVE('',#4585,#4585,#1929,.T.);
#5952=EDGE_CURVE('',#4585,#4586,#3163,.T.);
#5953=EDGE_CURVE('',#4586,#4586,#1930,.T.);
#5954=EDGE_CURVE('',#4587,#4587,#1931,.T.);
#5955=EDGE_CURVE('',#4587,#4588,#3164,.T.);
#5956=EDGE_CURVE('',#4588,#4588,#1932,.T.);
#5957=EDGE_CURVE('',#4589,#4589,#1933,.T.);
#5958=EDGE_CURVE('',#4589,#4590,#3165,.T.);
#5959=EDGE_CURVE('',#4590,#4590,#1934,.T.);
#5960=EDGE_CURVE('',#4591,#4591,#1935,.T.);
#5961=EDGE_CURVE('',#4591,#4592,#3166,.T.);
#5962=EDGE_CURVE('',#4592,#4592,#1936,.T.);
#5963=EDGE_CURVE('',#4593,#4593,#1937,.T.);
#5964=EDGE_CURVE('',#4593,#4594,#3167,.T.);
#5965=EDGE_CURVE('',#4594,#4594,#1938,.T.);
#5966=EDGE_CURVE('',#4595,#4595,#1939,.T.);
#5967=EDGE_CURVE('',#4595,#4596,#3168,.T.);
#5968=EDGE_CURVE('',#4596,#4596,#1940,.T.);
#5969=EDGE_CURVE('',#4597,#4597,#1941,.T.);
#5970=EDGE_CURVE('',#4597,#4598,#3169,.T.);
#5971=EDGE_CURVE('',#4598,#4598,#1942,.T.);
#5972=EDGE_CURVE('',#4599,#4599,#1943,.T.);
#5973=EDGE_CURVE('',#4599,#4600,#3170,.T.);
#5974=EDGE_CURVE('',#4600,#4600,#1944,.T.);
#5975=EDGE_CURVE('',#4601,#4601,#1945,.T.);
#5976=EDGE_CURVE('',#4601,#4602,#3171,.T.);
#5977=EDGE_CURVE('',#4602,#4602,#1946,.T.);
#5978=EDGE_CURVE('',#4603,#4603,#1947,.T.);
#5979=EDGE_CURVE('',#4603,#4604,#3172,.T.);
#5980=EDGE_CURVE('',#4604,#4604,#1948,.T.);
#5981=EDGE_CURVE('',#4605,#4605,#1949,.T.);
#5982=EDGE_CURVE('',#4605,#4606,#3173,.T.);
#5983=EDGE_CURVE('',#4606,#4606,#1950,.T.);
#5984=EDGE_CURVE('',#4607,#4607,#1951,.T.);
#5985=EDGE_CURVE('',#4607,#4608,#3174,.T.);
#5986=EDGE_CURVE('',#4608,#4608,#1952,.T.);
#5987=EDGE_CURVE('',#4609,#4609,#1953,.T.);
#5988=EDGE_CURVE('',#4609,#4610,#3175,.T.);
#5989=EDGE_CURVE('',#4610,#4610,#1954,.T.);
#5990=EDGE_CURVE('',#4611,#4611,#1955,.T.);
#5991=EDGE_CURVE('',#4611,#4612,#3176,.T.);
#5992=EDGE_CURVE('',#4612,#4612,#1956,.T.);
#5993=EDGE_CURVE('',#4613,#4613,#1957,.T.);
#5994=EDGE_CURVE('',#4613,#4614,#3177,.T.);
#5995=EDGE_CURVE('',#4614,#4614,#1958,.T.);
#5996=EDGE_CURVE('',#4615,#4615,#1959,.T.);
#5997=EDGE_CURVE('',#4615,#4616,#3178,.T.);
#5998=EDGE_CURVE('',#4616,#4616,#1960,.T.);
#5999=EDGE_CURVE('',#4617,#4617,#1961,.T.);
#6000=EDGE_CURVE('',#4617,#4618,#3179,.T.);
#6001=EDGE_CURVE('',#4618,#4618,#1962,.T.);
#6002=EDGE_CURVE('',#4619,#4619,#1963,.T.);
#6003=EDGE_CURVE('',#4619,#4620,#3180,.T.);
#6004=EDGE_CURVE('',#4620,#4620,#1964,.T.);
#6005=EDGE_CURVE('',#4621,#4621,#1965,.T.);
#6006=EDGE_CURVE('',#4621,#4622,#3181,.T.);
#6007=EDGE_CURVE('',#4622,#4622,#1966,.T.);
#6008=EDGE_CURVE('',#4623,#4624,#3182,.T.);
#6009=EDGE_CURVE('',#4624,#4625,#3183,.F.);
#6010=EDGE_CURVE('',#4626,#4625,#3184,.T.);
#6011=EDGE_CURVE('',#4623,#4626,#3185,.T.);
#6012=EDGE_CURVE('',#4627,#4623,#3186,.F.);
#6013=EDGE_CURVE('',#4628,#4626,#3187,.F.);
#6014=EDGE_CURVE('',#4627,#4628,#3188,.T.);
#6015=EDGE_CURVE('',#4629,#4627,#3189,.F.);
#6016=EDGE_CURVE('',#4630,#4628,#3190,.F.);
#6017=EDGE_CURVE('',#4629,#4630,#3191,.F.);
#6018=EDGE_CURVE('',#4624,#4629,#3192,.F.);
#6019=EDGE_CURVE('',#4625,#4630,#3193,.F.);
#6020=EDGE_CURVE('',#4631,#4631,#1967,.T.);
#6021=EDGE_CURVE('',#4631,#4632,#3194,.T.);
#6022=EDGE_CURVE('',#4632,#4632,#1968,.T.);
#6023=EDGE_CURVE('',#4633,#4633,#1969,.T.);
#6024=EDGE_CURVE('',#4633,#4634,#3195,.T.);
#6025=EDGE_CURVE('',#4634,#4634,#1970,.T.);
#6026=EDGE_CURVE('',#4635,#4635,#1971,.T.);
#6027=EDGE_CURVE('',#4635,#4636,#3196,.T.);
#6028=EDGE_CURVE('',#4636,#4636,#1972,.T.);
#6029=EDGE_CURVE('',#4637,#4637,#1973,.T.);
#6030=EDGE_CURVE('',#4637,#4638,#3197,.T.);
#6031=EDGE_CURVE('',#4638,#4638,#1974,.T.);
#6032=EDGE_CURVE('',#4639,#4639,#1975,.T.);
#6033=EDGE_CURVE('',#4639,#4640,#3198,.T.);
#6034=EDGE_CURVE('',#4640,#4640,#1976,.T.);
#6035=EDGE_CURVE('',#4641,#4641,#1977,.T.);
#6036=EDGE_CURVE('',#4641,#4642,#3199,.T.);
#6037=EDGE_CURVE('',#4642,#4642,#1978,.T.);
#6038=EDGE_CURVE('',#4643,#4643,#1979,.T.);
#6039=EDGE_CURVE('',#4643,#4644,#3200,.T.);
#6040=EDGE_CURVE('',#4644,#4644,#1980,.T.);
#6041=EDGE_CURVE('',#4645,#4646,#3201,.T.);
#6042=EDGE_CURVE('',#4646,#4647,#3202,.T.);
#6043=EDGE_CURVE('',#4648,#4647,#3203,.T.);
#6044=EDGE_CURVE('',#4645,#4648,#3204,.T.);
#6045=EDGE_CURVE('',#4649,#4645,#3205,.T.);
#6046=EDGE_CURVE('',#4650,#4648,#3206,.T.);
#6047=EDGE_CURVE('',#4649,#4650,#3207,.T.);
#6048=EDGE_CURVE('',#4651,#4649,#3208,.T.);
#6049=EDGE_CURVE('',#4652,#4650,#3209,.T.);
#6050=EDGE_CURVE('',#4651,#4652,#3210,.T.);
#6051=EDGE_CURVE('',#4646,#4651,#3211,.T.);
#6052=EDGE_CURVE('',#4647,#4652,#3212,.T.);
#6053=EDGE_CURVE('',#4653,#4654,#3213,.T.);
#6054=EDGE_CURVE('',#4653,#4655,#2627,.T.);
#6055=EDGE_CURVE('',#4655,#4656,#1981,.F.);
#6056=EDGE_CURVE('',#4656,#4654,#2628,.T.);
#6057=EDGE_CURVE('',#4657,#4658,#3214,.T.);
#6058=EDGE_CURVE('',#4657,#4653,#2629,.T.);
#6059=EDGE_CURVE('',#4654,#4658,#2630,.T.);
#6060=EDGE_CURVE('',#4659,#4660,#3215,.T.);
#6061=EDGE_CURVE('',#4659,#4657,#2631,.T.);
#6062=EDGE_CURVE('',#4658,#4660,#2632,.T.);
#6063=EDGE_CURVE('',#4661,#4662,#3216,.T.);
#6064=EDGE_CURVE('',#4661,#4659,#2633,.T.);
#6065=EDGE_CURVE('',#4660,#4662,#2634,.T.);
#6066=EDGE_CURVE('',#4663,#4664,#3217,.T.);
#6067=EDGE_CURVE('',#4663,#4661,#2635,.T.);
#6068=EDGE_CURVE('',#4662,#4664,#2636,.T.);
#6069=EDGE_CURVE('',#4665,#4666,#3218,.T.);
#6070=EDGE_CURVE('',#4665,#4663,#2637,.T.);
#6071=EDGE_CURVE('',#4664,#4666,#2638,.T.);
#6072=EDGE_CURVE('',#4667,#4668,#3219,.T.);
#6073=EDGE_CURVE('',#4667,#4665,#2639,.T.);
#6074=EDGE_CURVE('',#4666,#4668,#2640,.T.);
#6075=EDGE_CURVE('',#4669,#4670,#3220,.T.);
#6076=EDGE_CURVE('',#4669,#4667,#2641,.T.);
#6077=EDGE_CURVE('',#4668,#4670,#2642,.T.);
#6078=EDGE_CURVE('',#4671,#4672,#3221,.T.);
#6079=EDGE_CURVE('',#4671,#4669,#2643,.T.);
#6080=EDGE_CURVE('',#4670,#4672,#2644,.T.);
#6081=EDGE_CURVE('',#4673,#4674,#3222,.T.);
#6082=EDGE_CURVE('',#4673,#4671,#2645,.T.);
#6083=EDGE_CURVE('',#4672,#4674,#2646,.T.);
#6084=EDGE_CURVE('',#4675,#4676,#3223,.T.);
#6085=EDGE_CURVE('',#4675,#4673,#2647,.T.);
#6086=EDGE_CURVE('',#4674,#4676,#2648,.T.);
#6087=EDGE_CURVE('',#4677,#4678,#3224,.T.);
#6088=EDGE_CURVE('',#4677,#4675,#2649,.T.);
#6089=EDGE_CURVE('',#4676,#4678,#2650,.T.);
#6090=EDGE_CURVE('',#4679,#4680,#3225,.T.);
#6091=EDGE_CURVE('',#4679,#4677,#2651,.T.);
#6092=EDGE_CURVE('',#4678,#4680,#2652,.T.);
#6093=EDGE_CURVE('',#4681,#4682,#3226,.T.);
#6094=EDGE_CURVE('',#4681,#4679,#2653,.T.);
#6095=EDGE_CURVE('',#4680,#4682,#2654,.T.);
#6096=EDGE_CURVE('',#4683,#4684,#3227,.T.);
#6097=EDGE_CURVE('',#4683,#4681,#2655,.T.);
#6098=EDGE_CURVE('',#4682,#4684,#2656,.T.);
#6099=EDGE_CURVE('',#4685,#4686,#3228,.T.);
#6100=EDGE_CURVE('',#4685,#4683,#2657,.T.);
#6101=EDGE_CURVE('',#4684,#4686,#2658,.T.);
#6102=EDGE_CURVE('',#4687,#4688,#3229,.T.);
#6103=EDGE_CURVE('',#4687,#4689,#2659,.T.);
#6104=EDGE_CURVE('',#4689,#4690,#1982,.T.);
#6105=EDGE_CURVE('',#4688,#4690,#2660,.T.);
#6106=EDGE_CURVE('',#4691,#4692,#3230,.T.);
#6107=EDGE_CURVE('',#4691,#4687,#2661,.T.);
#6108=EDGE_CURVE('',#4692,#4688,#2662,.T.);
#6109=EDGE_CURVE('',#4693,#4694,#3231,.T.);
#6110=EDGE_CURVE('',#4693,#4691,#2663,.T.);
#6111=EDGE_CURVE('',#4694,#4692,#2664,.T.);
#6112=EDGE_CURVE('',#4695,#4696,#3232,.T.);
#6113=EDGE_CURVE('',#4695,#4693,#2665,.T.);
#6114=EDGE_CURVE('',#4696,#4694,#2666,.T.);
#6115=EDGE_CURVE('',#4697,#4698,#3233,.T.);
#6116=EDGE_CURVE('',#4697,#4695,#2667,.T.);
#6117=EDGE_CURVE('',#4698,#4696,#2668,.T.);
#6118=EDGE_CURVE('',#4699,#4700,#3234,.T.);
#6119=EDGE_CURVE('',#4699,#4697,#2669,.T.);
#6120=EDGE_CURVE('',#4700,#4698,#2670,.T.);
#6121=EDGE_CURVE('',#4701,#4702,#3235,.T.);
#6122=EDGE_CURVE('',#4701,#4699,#2671,.T.);
#6123=EDGE_CURVE('',#4702,#4700,#2672,.T.);
#6124=EDGE_CURVE('',#4703,#4704,#3236,.T.);
#6125=EDGE_CURVE('',#4703,#4701,#2673,.T.);
#6126=EDGE_CURVE('',#4704,#4702,#2674,.T.);
#6127=EDGE_CURVE('',#4705,#4706,#3237,.T.);
#6128=EDGE_CURVE('',#4705,#4703,#2675,.T.);
#6129=EDGE_CURVE('',#4706,#4704,#2676,.T.);
#6130=EDGE_CURVE('',#4707,#4708,#3238,.T.);
#6131=EDGE_CURVE('',#4707,#4705,#2677,.T.);
#6132=EDGE_CURVE('',#4708,#4706,#2678,.T.);
#6133=EDGE_CURVE('',#4709,#4710,#3239,.T.);
#6134=EDGE_CURVE('',#4709,#4707,#2679,.T.);
#6135=EDGE_CURVE('',#4710,#4708,#2680,.T.);
#6136=EDGE_CURVE('',#4711,#4712,#3240,.T.);
#6137=EDGE_CURVE('',#4711,#4709,#2681,.T.);
#6138=EDGE_CURVE('',#4712,#4710,#2682,.T.);
#6139=EDGE_CURVE('',#4713,#4714,#3241,.T.);
#6140=EDGE_CURVE('',#4713,#4711,#2683,.T.);
#6141=EDGE_CURVE('',#4714,#4712,#2684,.T.);
#6142=EDGE_CURVE('',#4715,#4716,#3242,.T.);
#6143=EDGE_CURVE('',#4715,#4713,#2685,.T.);
#6144=EDGE_CURVE('',#4716,#4714,#2686,.T.);
#6145=EDGE_CURVE('',#4717,#4718,#3243,.T.);
#6146=EDGE_CURVE('',#4717,#4715,#2687,.T.);
#6147=EDGE_CURVE('',#4718,#4716,#2688,.T.);
#6148=EDGE_CURVE('',#4719,#4720,#3244,.T.);
#6149=EDGE_CURVE('',#4719,#4717,#2689,.T.);
#6150=EDGE_CURVE('',#4720,#4718,#2690,.T.);
#6151=EDGE_CURVE('',#4690,#4721,#2691,.T.);
#6152=EDGE_CURVE('',#4722,#4689,#2692,.T.);
#6153=EDGE_CURVE('',#4723,#4722,#1983,.T.);
#6154=EDGE_CURVE('',#4721,#4723,#2693,.T.);
#6155=EDGE_CURVE('',#4721,#4724,#3245,.T.);
#6156=EDGE_CURVE('',#4724,#4724,#1984,.T.);
#6157=EDGE_CURVE('',#4725,#4719,#2694,.T.);
#6158=EDGE_CURVE('',#4655,#4725,#2695,.T.);
#6159=EDGE_CURVE('',#4722,#4685,#2696,.T.);
#6160=EDGE_CURVE('',#4726,#4720,#2697,.T.);
#6161=EDGE_CURVE('',#4725,#4726,#1985,.T.);
#6162=EDGE_CURVE('',#4686,#4723,#2698,.T.);
#6163=EDGE_CURVE('',#4726,#4656,#2699,.T.);
#6164=EDGE_CURVE('',#4727,#4728,#3246,.T.);
#6165=EDGE_CURVE('',#4727,#4729,#3247,.T.);
#6166=EDGE_CURVE('',#4729,#4730,#3248,.T.);
#6167=EDGE_CURVE('',#4728,#4730,#3249,.T.);
#6168=EDGE_CURVE('',#4731,#4727,#3250,.T.);
#6169=EDGE_CURVE('',#4731,#4732,#3251,.T.);
#6170=EDGE_CURVE('',#4732,#4729,#3252,.T.);
#6171=EDGE_CURVE('',#4733,#4731,#3253,.T.);
#6172=EDGE_CURVE('',#4733,#4734,#3254,.T.);
#6173=EDGE_CURVE('',#4734,#4732,#3255,.T.);
#6174=EDGE_CURVE('',#4735,#4733,#3256,.T.);
#6175=EDGE_CURVE('',#4735,#4736,#3257,.T.);
#6176=EDGE_CURVE('',#4736,#4734,#3258,.T.);
#6177=EDGE_CURVE('',#4737,#4735,#3259,.T.);
#6178=EDGE_CURVE('',#4737,#4738,#3260,.T.);
#6179=EDGE_CURVE('',#4738,#4736,#3261,.T.);
#6180=EDGE_CURVE('',#4728,#4737,#3262,.T.);
#6181=EDGE_CURVE('',#4730,#4738,#3263,.T.);
#6182=EDGE_CURVE('',#4739,#4739,#1986,.T.);
#6183=EDGE_CURVE('',#4739,#4740,#3264,.T.);
#6184=EDGE_CURVE('',#4740,#4740,#1987,.T.);
#6185=EDGE_CURVE('',#4741,#4742,#3265,.T.);
#6186=EDGE_CURVE('',#4741,#4743,#2700,.T.);
#6187=EDGE_CURVE('',#4743,#4744,#1988,.F.);
#6188=EDGE_CURVE('',#4744,#4742,#2701,.T.);
#6189=EDGE_CURVE('',#4745,#4746,#3266,.T.);
#6190=EDGE_CURVE('',#4745,#4741,#2702,.T.);
#6191=EDGE_CURVE('',#4742,#4746,#2703,.T.);
#6192=EDGE_CURVE('',#4747,#4748,#3267,.T.);
#6193=EDGE_CURVE('',#4747,#4745,#2704,.T.);
#6194=EDGE_CURVE('',#4746,#4748,#2705,.T.);
#6195=EDGE_CURVE('',#4749,#4750,#3268,.T.);
#6196=EDGE_CURVE('',#4749,#4747,#2706,.T.);
#6197=EDGE_CURVE('',#4748,#4750,#2707,.T.);
#6198=EDGE_CURVE('',#4751,#4752,#3269,.T.);
#6199=EDGE_CURVE('',#4751,#4749,#2708,.T.);
#6200=EDGE_CURVE('',#4750,#4752,#2709,.T.);
#6201=EDGE_CURVE('',#4753,#4754,#3270,.T.);
#6202=EDGE_CURVE('',#4753,#4751,#2710,.T.);
#6203=EDGE_CURVE('',#4752,#4754,#2711,.T.);
#6204=EDGE_CURVE('',#4755,#4756,#3271,.T.);
#6205=EDGE_CURVE('',#4755,#4753,#2712,.T.);
#6206=EDGE_CURVE('',#4754,#4756,#2713,.T.);
#6207=EDGE_CURVE('',#4757,#4758,#3272,.T.);
#6208=EDGE_CURVE('',#4757,#4755,#2714,.T.);
#6209=EDGE_CURVE('',#4756,#4758,#2715,.T.);
#6210=EDGE_CURVE('',#4759,#4760,#3273,.T.);
#6211=EDGE_CURVE('',#4759,#4757,#2716,.T.);
#6212=EDGE_CURVE('',#4758,#4760,#2717,.T.);
#6213=EDGE_CURVE('',#4761,#4762,#3274,.T.);
#6214=EDGE_CURVE('',#4761,#4759,#2718,.T.);
#6215=EDGE_CURVE('',#4760,#4762,#2719,.T.);
#6216=EDGE_CURVE('',#4763,#4764,#3275,.T.);
#6217=EDGE_CURVE('',#4763,#4761,#2720,.T.);
#6218=EDGE_CURVE('',#4762,#4764,#2721,.T.);
#6219=EDGE_CURVE('',#4765,#4766,#3276,.T.);
#6220=EDGE_CURVE('',#4765,#4767,#2722,.T.);
#6221=EDGE_CURVE('',#4767,#4768,#1989,.T.);
#6222=EDGE_CURVE('',#4766,#4768,#2723,.T.);
#6223=EDGE_CURVE('',#4769,#4770,#3277,.T.);
#6224=EDGE_CURVE('',#4769,#4765,#2724,.T.);
#6225=EDGE_CURVE('',#4770,#4766,#2725,.T.);
#6226=EDGE_CURVE('',#4771,#4772,#3278,.T.);
#6227=EDGE_CURVE('',#4771,#4769,#2726,.T.);
#6228=EDGE_CURVE('',#4772,#4770,#2727,.T.);
#6229=EDGE_CURVE('',#4773,#4774,#3279,.T.);
#6230=EDGE_CURVE('',#4773,#4771,#2728,.T.);
#6231=EDGE_CURVE('',#4774,#4772,#2729,.T.);
#6232=EDGE_CURVE('',#4775,#4776,#3280,.T.);
#6233=EDGE_CURVE('',#4775,#4773,#2730,.T.);
#6234=EDGE_CURVE('',#4776,#4774,#2731,.T.);
#6235=EDGE_CURVE('',#4777,#4778,#3281,.T.);
#6236=EDGE_CURVE('',#4777,#4775,#2732,.T.);
#6237=EDGE_CURVE('',#4778,#4776,#2733,.T.);
#6238=EDGE_CURVE('',#4779,#4780,#3282,.T.);
#6239=EDGE_CURVE('',#4779,#4777,#2734,.T.);
#6240=EDGE_CURVE('',#4780,#4778,#2735,.T.);
#6241=EDGE_CURVE('',#4781,#4782,#3283,.T.);
#6242=EDGE_CURVE('',#4781,#4779,#2736,.T.);
#6243=EDGE_CURVE('',#4782,#4780,#2737,.T.);
#6244=EDGE_CURVE('',#4783,#4784,#3284,.T.);
#6245=EDGE_CURVE('',#4783,#4781,#2738,.T.);
#6246=EDGE_CURVE('',#4784,#4782,#2739,.T.);
#6247=EDGE_CURVE('',#4785,#4786,#3285,.T.);
#6248=EDGE_CURVE('',#4785,#4783,#2740,.T.);
#6249=EDGE_CURVE('',#4786,#4784,#2741,.T.);
#6250=EDGE_CURVE('',#4787,#4788,#3286,.T.);
#6251=EDGE_CURVE('',#4787,#4785,#2742,.T.);
#6252=EDGE_CURVE('',#4788,#4786,#2743,.T.);
#6253=EDGE_CURVE('',#4768,#4789,#2744,.T.);
#6254=EDGE_CURVE('',#4790,#4767,#2745,.T.);
#6255=EDGE_CURVE('',#4791,#4790,#1990,.T.);
#6256=EDGE_CURVE('',#4789,#4791,#2746,.T.);
#6257=EDGE_CURVE('',#4789,#4792,#3287,.T.);
#6258=EDGE_CURVE('',#4792,#4792,#1991,.T.);
#6259=EDGE_CURVE('',#4793,#4787,#2747,.T.);
#6260=EDGE_CURVE('',#4743,#4793,#2748,.T.);
#6261=EDGE_CURVE('',#4790,#4763,#2749,.T.);
#6262=EDGE_CURVE('',#4794,#4788,#2750,.T.);
#6263=EDGE_CURVE('',#4793,#4794,#1992,.T.);
#6264=EDGE_CURVE('',#4764,#4791,#2751,.T.);
#6265=EDGE_CURVE('',#4794,#4744,#2752,.T.);
#6266=EDGE_CURVE('',#4795,#4796,#3288,.T.);
#6267=EDGE_CURVE('',#4795,#4797,#3289,.T.);
#6268=EDGE_CURVE('',#4797,#4798,#3290,.T.);
#6269=EDGE_CURVE('',#4796,#4798,#3291,.T.);
#6270=EDGE_CURVE('',#4799,#4795,#3292,.T.);
#6271=EDGE_CURVE('',#4799,#4800,#3293,.T.);
#6272=EDGE_CURVE('',#4800,#4797,#3294,.T.);
#6273=EDGE_CURVE('',#4801,#4799,#3295,.T.);
#6274=EDGE_CURVE('',#4801,#4802,#3296,.T.);
#6275=EDGE_CURVE('',#4802,#4800,#3297,.T.);
#6276=EDGE_CURVE('',#4803,#4801,#3298,.T.);
#6277=EDGE_CURVE('',#4803,#4804,#3299,.T.);
#6278=EDGE_CURVE('',#4804,#4802,#3300,.T.);
#6279=EDGE_CURVE('',#4805,#4803,#3301,.T.);
#6280=EDGE_CURVE('',#4805,#4806,#3302,.T.);
#6281=EDGE_CURVE('',#4806,#4804,#3303,.T.);
#6282=EDGE_CURVE('',#4796,#4805,#3304,.T.);
#6283=EDGE_CURVE('',#4798,#4806,#3305,.T.);
#6284=EDGE_CURVE('',#4807,#4807,#1993,.T.);
#6285=EDGE_CURVE('',#4807,#4808,#3306,.T.);
#6286=EDGE_CURVE('',#4808,#4808,#1994,.T.);
#6287=EDGE_CURVE('',#4809,#4810,#3307,.T.);
#6288=EDGE_CURVE('',#4809,#4811,#2753,.T.);
#6289=EDGE_CURVE('',#4811,#4812,#1995,.F.);
#6290=EDGE_CURVE('',#4812,#4810,#2754,.T.);
#6291=EDGE_CURVE('',#4813,#4814,#3308,.T.);
#6292=EDGE_CURVE('',#4813,#4809,#2755,.T.);
#6293=EDGE_CURVE('',#4810,#4814,#2756,.T.);
#6294=EDGE_CURVE('',#4815,#4816,#3309,.T.);
#6295=EDGE_CURVE('',#4815,#4813,#2757,.T.);
#6296=EDGE_CURVE('',#4814,#4816,#2758,.T.);
#6297=EDGE_CURVE('',#4817,#4818,#3310,.T.);
#6298=EDGE_CURVE('',#4817,#4815,#2759,.T.);
#6299=EDGE_CURVE('',#4816,#4818,#2760,.T.);
#6300=EDGE_CURVE('',#4819,#4820,#3311,.T.);
#6301=EDGE_CURVE('',#4819,#4817,#2761,.T.);
#6302=EDGE_CURVE('',#4818,#4820,#2762,.T.);
#6303=EDGE_CURVE('',#4821,#4822,#3312,.T.);
#6304=EDGE_CURVE('',#4821,#4819,#2763,.T.);
#6305=EDGE_CURVE('',#4820,#4822,#2764,.T.);
#6306=EDGE_CURVE('',#4823,#4824,#3313,.T.);
#6307=EDGE_CURVE('',#4823,#4821,#2765,.T.);
#6308=EDGE_CURVE('',#4822,#4824,#2766,.T.);
#6309=EDGE_CURVE('',#4825,#4826,#3314,.T.);
#6310=EDGE_CURVE('',#4825,#4823,#2767,.T.);
#6311=EDGE_CURVE('',#4824,#4826,#2768,.T.);
#6312=EDGE_CURVE('',#4827,#4828,#3315,.T.);
#6313=EDGE_CURVE('',#4827,#4825,#2769,.T.);
#6314=EDGE_CURVE('',#4826,#4828,#2770,.T.);
#6315=EDGE_CURVE('',#4829,#4830,#3316,.T.);
#6316=EDGE_CURVE('',#4829,#4827,#2771,.T.);
#6317=EDGE_CURVE('',#4828,#4830,#2772,.T.);
#6318=EDGE_CURVE('',#4831,#4832,#3317,.T.);
#6319=EDGE_CURVE('',#4831,#4833,#2773,.T.);
#6320=EDGE_CURVE('',#4834,#4833,#1996,.T.);
#6321=EDGE_CURVE('',#4832,#4834,#2774,.T.);
#6322=EDGE_CURVE('',#4835,#4836,#3318,.T.);
#6323=EDGE_CURVE('',#4835,#4831,#2775,.T.);
#6324=EDGE_CURVE('',#4836,#4832,#2776,.T.);
#6325=EDGE_CURVE('',#4837,#4838,#3319,.T.);
#6326=EDGE_CURVE('',#4837,#4835,#2777,.T.);
#6327=EDGE_CURVE('',#4838,#4836,#2778,.T.);
#6328=EDGE_CURVE('',#4839,#4840,#3320,.T.);
#6329=EDGE_CURVE('',#4839,#4837,#2779,.T.);
#6330=EDGE_CURVE('',#4840,#4838,#2780,.T.);
#6331=EDGE_CURVE('',#4841,#4842,#3321,.T.);
#6332=EDGE_CURVE('',#4841,#4839,#2781,.T.);
#6333=EDGE_CURVE('',#4842,#4840,#2782,.T.);
#6334=EDGE_CURVE('',#4843,#4844,#3322,.T.);
#6335=EDGE_CURVE('',#4843,#4841,#2783,.T.);
#6336=EDGE_CURVE('',#4844,#4842,#2784,.T.);
#6337=EDGE_CURVE('',#4845,#4846,#3323,.T.);
#6338=EDGE_CURVE('',#4845,#4843,#2785,.T.);
#6339=EDGE_CURVE('',#4846,#4844,#2786,.T.);
#6340=EDGE_CURVE('',#4847,#4848,#3324,.T.);
#6341=EDGE_CURVE('',#4847,#4845,#2787,.T.);
#6342=EDGE_CURVE('',#4848,#4846,#2788,.T.);
#6343=EDGE_CURVE('',#4849,#4850,#3325,.T.);
#6344=EDGE_CURVE('',#4849,#4847,#2789,.T.);
#6345=EDGE_CURVE('',#4850,#4848,#2790,.T.);
#6346=EDGE_CURVE('',#4851,#4834,#2791,.T.);
#6347=EDGE_CURVE('',#4830,#4851,#2792,.T.);
#6348=EDGE_CURVE('',#4852,#4812,#2793,.T.);
#6349=EDGE_CURVE('',#4852,#4850,#2794,.T.);
#6350=EDGE_CURVE('',#4853,#4852,#1997,.T.);
#6351=EDGE_CURVE('',#4853,#4849,#2795,.T.);
#6352=EDGE_CURVE('',#4833,#4854,#2796,.T.);
#6353=EDGE_CURVE('',#4811,#4853,#2797,.T.);
#6354=EDGE_CURVE('',#4854,#4829,#2798,.T.);
#6355=EDGE_CURVE('',#4854,#4851,#1998,.F.);
#6356=EDGE_CURVE('',#4855,#4855,#1999,.T.);
#6357=EDGE_CURVE('',#4856,#4856,#2000,.T.);
#6358=EDGE_CURVE('',#4857,#4857,#2001,.T.);
#6359=EDGE_CURVE('',#4858,#4858,#2002,.T.);
#6360=EDGE_CURVE('',#4855,#4857,#3326,.T.);
#6361=EDGE_CURVE('',#4858,#4859,#3327,.T.);
#6362=EDGE_CURVE('',#4859,#4859,#2003,.T.);
#6363=EDGE_CURVE('',#4860,#4860,#2004,.T.);
#6364=EDGE_CURVE('',#4861,#4861,#2005,.T.);
#6365=EDGE_CURVE('',#4862,#4862,#2006,.T.);
#6366=EDGE_CURVE('',#4860,#4861,#3328,.T.);
#6367=EDGE_CURVE('',#4862,#4863,#3329,.T.);
#6368=EDGE_CURVE('',#4863,#4863,#2007,.T.);
#6369=EDGE_CURVE('',#4864,#4864,#2008,.T.);
#6370=EDGE_CURVE('',#4865,#4865,#2009,.T.);
#6371=EDGE_CURVE('',#4866,#4866,#2010,.T.);
#6372=EDGE_CURVE('',#4864,#4865,#3330,.T.);
#6373=EDGE_CURVE('',#4866,#4867,#3331,.T.);
#6374=EDGE_CURVE('',#4867,#4867,#2011,.T.);
#6375=EDGE_CURVE('',#4868,#4868,#2012,.T.);
#6376=EDGE_CURVE('',#4868,#4856,#3332,.T.);
#6377=EDGE_CURVE('',#4869,#4869,#2013,.T.);
#6378=EDGE_CURVE('',#4870,#4870,#2014,.T.);
#6379=EDGE_CURVE('',#4870,#4871,#3333,.T.);
#6380=EDGE_CURVE('',#4871,#4871,#2015,.T.);
#6381=EDGE_CURVE('',#4872,#4872,#2016,.T.);
#6382=EDGE_CURVE('',#4872,#4869,#3334,.T.);
#6383=EDGE_CURVE('',#4873,#4873,#2017,.T.);
#6384=EDGE_CURVE('',#4873,#4874,#3335,.T.);
#6385=EDGE_CURVE('',#4874,#4874,#2018,.T.);
#6386=EDGE_CURVE('',#4875,#4875,#2019,.T.);
#6387=EDGE_CURVE('',#4875,#4876,#3336,.T.);
#6388=EDGE_CURVE('',#4876,#4876,#2020,.T.);
#6389=ORIENTED_EDGE('',*,*,#4877,.T.);
#6390=ORIENTED_EDGE('',*,*,#4878,.T.);
#6391=ORIENTED_EDGE('',*,*,#4879,.T.);
#6392=ORIENTED_EDGE('',*,*,#4880,.T.);
#6393=ORIENTED_EDGE('',*,*,#4881,.T.);
#6394=ORIENTED_EDGE('',*,*,#4882,.T.);
#6395=ORIENTED_EDGE('',*,*,#4881,.F.);
#6396=ORIENTED_EDGE('',*,*,#4883,.T.);
#6397=ORIENTED_EDGE('',*,*,#4884,.T.);
#6398=ORIENTED_EDGE('',*,*,#4885,.T.);
#6399=ORIENTED_EDGE('',*,*,#4877,.F.);
#6400=ORIENTED_EDGE('',*,*,#4886,.T.);
#6401=ORIENTED_EDGE('',*,*,#4887,.T.);
#6402=ORIENTED_EDGE('',*,*,#4888,.T.);
#6403=ORIENTED_EDGE('',*,*,#4884,.F.);
#6404=ORIENTED_EDGE('',*,*,#4889,.T.);
#6405=ORIENTED_EDGE('',*,*,#4890,.T.);
#6406=ORIENTED_EDGE('',*,*,#4891,.T.);
#6407=ORIENTED_EDGE('',*,*,#4887,.F.);
#6408=ORIENTED_EDGE('',*,*,#4892,.T.);
#6409=ORIENTED_EDGE('',*,*,#4893,.T.);
#6410=ORIENTED_EDGE('',*,*,#4894,.T.);
#6411=ORIENTED_EDGE('',*,*,#4890,.F.);
#6412=ORIENTED_EDGE('',*,*,#4895,.T.);
#6413=ORIENTED_EDGE('',*,*,#4896,.T.);
#6414=ORIENTED_EDGE('',*,*,#4897,.T.);
#6415=ORIENTED_EDGE('',*,*,#4893,.F.);
#6416=ORIENTED_EDGE('',*,*,#4898,.T.);
#6417=ORIENTED_EDGE('',*,*,#4899,.T.);
#6418=ORIENTED_EDGE('',*,*,#4900,.T.);
#6419=ORIENTED_EDGE('',*,*,#4896,.F.);
#6420=ORIENTED_EDGE('',*,*,#4901,.T.);
#6421=ORIENTED_EDGE('',*,*,#4902,.T.);
#6422=ORIENTED_EDGE('',*,*,#4903,.T.);
#6423=ORIENTED_EDGE('',*,*,#4899,.F.);
#6424=ORIENTED_EDGE('',*,*,#4904,.T.);
#6425=ORIENTED_EDGE('',*,*,#4905,.T.);
#6426=ORIENTED_EDGE('',*,*,#4906,.T.);
#6427=ORIENTED_EDGE('',*,*,#4902,.F.);
#6428=ORIENTED_EDGE('',*,*,#4907,.T.);
#6429=ORIENTED_EDGE('',*,*,#4908,.T.);
#6430=ORIENTED_EDGE('',*,*,#4909,.T.);
#6431=ORIENTED_EDGE('',*,*,#4905,.F.);
#6432=ORIENTED_EDGE('',*,*,#4910,.T.);
#6433=ORIENTED_EDGE('',*,*,#4911,.T.);
#6434=ORIENTED_EDGE('',*,*,#4912,.T.);
#6435=ORIENTED_EDGE('',*,*,#4908,.F.);
#6436=ORIENTED_EDGE('',*,*,#4913,.T.);
#6437=ORIENTED_EDGE('',*,*,#4914,.T.);
#6438=ORIENTED_EDGE('',*,*,#4915,.T.);
#6439=ORIENTED_EDGE('',*,*,#4911,.F.);
#6440=ORIENTED_EDGE('',*,*,#4916,.T.);
#6441=ORIENTED_EDGE('',*,*,#4917,.T.);
#6442=ORIENTED_EDGE('',*,*,#4918,.T.);
#6443=ORIENTED_EDGE('',*,*,#4914,.F.);
#6444=ORIENTED_EDGE('',*,*,#4919,.T.);
#6445=ORIENTED_EDGE('',*,*,#4920,.T.);
#6446=ORIENTED_EDGE('',*,*,#4921,.T.);
#6447=ORIENTED_EDGE('',*,*,#4917,.F.);
#6448=ORIENTED_EDGE('',*,*,#4922,.T.);
#6449=ORIENTED_EDGE('',*,*,#4923,.F.);
#6450=ORIENTED_EDGE('',*,*,#4924,.T.);
#6451=ORIENTED_EDGE('',*,*,#4925,.F.);
#6452=ORIENTED_EDGE('',*,*,#4926,.T.);
#6453=ORIENTED_EDGE('',*,*,#4927,.T.);
#6454=ORIENTED_EDGE('',*,*,#4928,.T.);
#6455=ORIENTED_EDGE('',*,*,#4929,.F.);
#6456=ORIENTED_EDGE('',*,*,#4930,.F.);
#6457=ORIENTED_EDGE('',*,*,#4931,.T.);
#6458=ORIENTED_EDGE('',*,*,#4932,.T.);
#6459=ORIENTED_EDGE('',*,*,#4927,.F.);
#6460=ORIENTED_EDGE('',*,*,#4933,.F.);
#6461=ORIENTED_EDGE('',*,*,#4934,.T.);
#6462=ORIENTED_EDGE('',*,*,#4935,.T.);
#6463=ORIENTED_EDGE('',*,*,#4931,.F.);
#6464=ORIENTED_EDGE('',*,*,#4936,.F.);
#6465=ORIENTED_EDGE('',*,*,#4937,.T.);
#6466=ORIENTED_EDGE('',*,*,#4938,.T.);
#6467=ORIENTED_EDGE('',*,*,#4934,.F.);
#6468=ORIENTED_EDGE('',*,*,#4939,.F.);
#6469=ORIENTED_EDGE('',*,*,#4940,.T.);
#6470=ORIENTED_EDGE('',*,*,#4941,.T.);
#6471=ORIENTED_EDGE('',*,*,#4937,.F.);
#6472=ORIENTED_EDGE('',*,*,#4942,.F.);
#6473=ORIENTED_EDGE('',*,*,#4943,.T.);
#6474=ORIENTED_EDGE('',*,*,#4944,.T.);
#6475=ORIENTED_EDGE('',*,*,#4940,.F.);
#6476=ORIENTED_EDGE('',*,*,#4945,.F.);
#6477=ORIENTED_EDGE('',*,*,#4946,.T.);
#6478=ORIENTED_EDGE('',*,*,#4947,.T.);
#6479=ORIENTED_EDGE('',*,*,#4943,.F.);
#6480=ORIENTED_EDGE('',*,*,#4948,.F.);
#6481=ORIENTED_EDGE('',*,*,#4949,.T.);
#6482=ORIENTED_EDGE('',*,*,#4950,.T.);
#6483=ORIENTED_EDGE('',*,*,#4946,.F.);
#6484=ORIENTED_EDGE('',*,*,#4951,.F.);
#6485=ORIENTED_EDGE('',*,*,#4952,.T.);
#6486=ORIENTED_EDGE('',*,*,#4953,.T.);
#6487=ORIENTED_EDGE('',*,*,#4949,.F.);
#6488=ORIENTED_EDGE('',*,*,#4954,.F.);
#6489=ORIENTED_EDGE('',*,*,#4955,.T.);
#6490=ORIENTED_EDGE('',*,*,#4956,.T.);
#6491=ORIENTED_EDGE('',*,*,#4952,.F.);
#6492=ORIENTED_EDGE('',*,*,#4957,.F.);
#6493=ORIENTED_EDGE('',*,*,#4958,.T.);
#6494=ORIENTED_EDGE('',*,*,#4959,.T.);
#6495=ORIENTED_EDGE('',*,*,#4955,.F.);
#6496=ORIENTED_EDGE('',*,*,#4960,.F.);
#6497=ORIENTED_EDGE('',*,*,#4961,.T.);
#6498=ORIENTED_EDGE('',*,*,#4962,.T.);
#6499=ORIENTED_EDGE('',*,*,#4958,.F.);
#6500=ORIENTED_EDGE('',*,*,#4963,.F.);
#6501=ORIENTED_EDGE('',*,*,#4964,.T.);
#6502=ORIENTED_EDGE('',*,*,#4965,.T.);
#6503=ORIENTED_EDGE('',*,*,#4961,.F.);
#6504=ORIENTED_EDGE('',*,*,#4966,.F.);
#6505=ORIENTED_EDGE('',*,*,#4967,.T.);
#6506=ORIENTED_EDGE('',*,*,#4968,.T.);
#6507=ORIENTED_EDGE('',*,*,#4964,.F.);
#6508=ORIENTED_EDGE('',*,*,#4969,.F.);
#6509=ORIENTED_EDGE('',*,*,#4970,.T.);
#6510=ORIENTED_EDGE('',*,*,#4971,.T.);
#6511=ORIENTED_EDGE('',*,*,#4967,.F.);
#6512=ORIENTED_EDGE('',*,*,#4972,.F.);
#6513=ORIENTED_EDGE('',*,*,#4973,.F.);
#6514=ORIENTED_EDGE('',*,*,#4974,.F.);
#6515=ORIENTED_EDGE('',*,*,#4975,.F.);
#6516=ORIENTED_EDGE('',*,*,#4976,.T.);
#6517=ORIENTED_EDGE('',*,*,#4977,.T.);
#6518=ORIENTED_EDGE('',*,*,#4978,.T.);
#6519=ORIENTED_EDGE('',*,*,#4979,.T.);
#6520=ORIENTED_EDGE('',*,*,#4980,.T.);
#6521=ORIENTED_EDGE('',*,*,#4981,.T.);
#6522=ORIENTED_EDGE('',*,*,#4982,.T.);
#6523=ORIENTED_EDGE('',*,*,#4981,.F.);
#6524=ORIENTED_EDGE('',*,*,#4983,.T.);
#6525=ORIENTED_EDGE('',*,*,#4984,.T.);
#6526=ORIENTED_EDGE('',*,*,#4985,.T.);
#6527=ORIENTED_EDGE('',*,*,#4977,.F.);
#6528=ORIENTED_EDGE('',*,*,#4986,.T.);
#6529=ORIENTED_EDGE('',*,*,#4987,.T.);
#6530=ORIENTED_EDGE('',*,*,#4988,.T.);
#6531=ORIENTED_EDGE('',*,*,#4984,.F.);
#6532=ORIENTED_EDGE('',*,*,#4989,.T.);
#6533=ORIENTED_EDGE('',*,*,#4990,.T.);
#6534=ORIENTED_EDGE('',*,*,#4991,.T.);
#6535=ORIENTED_EDGE('',*,*,#4987,.F.);
#6536=ORIENTED_EDGE('',*,*,#4992,.T.);
#6537=ORIENTED_EDGE('',*,*,#4993,.T.);
#6538=ORIENTED_EDGE('',*,*,#4994,.T.);
#6539=ORIENTED_EDGE('',*,*,#4990,.F.);
#6540=ORIENTED_EDGE('',*,*,#4995,.T.);
#6541=ORIENTED_EDGE('',*,*,#4996,.T.);
#6542=ORIENTED_EDGE('',*,*,#4997,.T.);
#6543=ORIENTED_EDGE('',*,*,#4993,.F.);
#6544=ORIENTED_EDGE('',*,*,#4998,.T.);
#6545=ORIENTED_EDGE('',*,*,#4999,.T.);
#6546=ORIENTED_EDGE('',*,*,#5000,.T.);
#6547=ORIENTED_EDGE('',*,*,#4996,.F.);
#6548=ORIENTED_EDGE('',*,*,#5001,.T.);
#6549=ORIENTED_EDGE('',*,*,#5002,.T.);
#6550=ORIENTED_EDGE('',*,*,#5003,.T.);
#6551=ORIENTED_EDGE('',*,*,#4999,.F.);
#6552=ORIENTED_EDGE('',*,*,#5004,.T.);
#6553=ORIENTED_EDGE('',*,*,#5005,.T.);
#6554=ORIENTED_EDGE('',*,*,#5006,.T.);
#6555=ORIENTED_EDGE('',*,*,#5002,.F.);
#6556=ORIENTED_EDGE('',*,*,#5007,.T.);
#6557=ORIENTED_EDGE('',*,*,#5008,.T.);
#6558=ORIENTED_EDGE('',*,*,#5009,.T.);
#6559=ORIENTED_EDGE('',*,*,#5005,.F.);
#6560=ORIENTED_EDGE('',*,*,#5010,.T.);
#6561=ORIENTED_EDGE('',*,*,#5011,.T.);
#6562=ORIENTED_EDGE('',*,*,#5012,.T.);
#6563=ORIENTED_EDGE('',*,*,#5008,.F.);
#6564=ORIENTED_EDGE('',*,*,#5013,.T.);
#6565=ORIENTED_EDGE('',*,*,#5014,.T.);
#6566=ORIENTED_EDGE('',*,*,#5015,.T.);
#6567=ORIENTED_EDGE('',*,*,#5011,.F.);
#6568=ORIENTED_EDGE('',*,*,#5016,.T.);
#6569=ORIENTED_EDGE('',*,*,#5017,.T.);
#6570=ORIENTED_EDGE('',*,*,#5018,.T.);
#6571=ORIENTED_EDGE('',*,*,#5014,.F.);
#6572=ORIENTED_EDGE('',*,*,#5019,.T.);
#6573=ORIENTED_EDGE('',*,*,#5020,.T.);
#6574=ORIENTED_EDGE('',*,*,#5021,.T.);
#6575=ORIENTED_EDGE('',*,*,#5017,.F.);
#6576=ORIENTED_EDGE('',*,*,#5022,.T.);
#6577=ORIENTED_EDGE('',*,*,#5023,.F.);
#6578=ORIENTED_EDGE('',*,*,#5024,.T.);
#6579=ORIENTED_EDGE('',*,*,#5025,.F.);
#6580=ORIENTED_EDGE('',*,*,#5026,.T.);
#6581=ORIENTED_EDGE('',*,*,#5027,.T.);
#6582=ORIENTED_EDGE('',*,*,#5028,.T.);
#6583=ORIENTED_EDGE('',*,*,#5029,.F.);
#6584=ORIENTED_EDGE('',*,*,#5030,.F.);
#6585=ORIENTED_EDGE('',*,*,#5031,.T.);
#6586=ORIENTED_EDGE('',*,*,#5032,.T.);
#6587=ORIENTED_EDGE('',*,*,#5027,.F.);
#6588=ORIENTED_EDGE('',*,*,#5033,.F.);
#6589=ORIENTED_EDGE('',*,*,#5034,.T.);
#6590=ORIENTED_EDGE('',*,*,#5035,.T.);
#6591=ORIENTED_EDGE('',*,*,#5031,.F.);
#6592=ORIENTED_EDGE('',*,*,#5036,.F.);
#6593=ORIENTED_EDGE('',*,*,#5037,.T.);
#6594=ORIENTED_EDGE('',*,*,#5038,.T.);
#6595=ORIENTED_EDGE('',*,*,#5034,.F.);
#6596=ORIENTED_EDGE('',*,*,#5039,.F.);
#6597=ORIENTED_EDGE('',*,*,#5040,.T.);
#6598=ORIENTED_EDGE('',*,*,#5041,.T.);
#6599=ORIENTED_EDGE('',*,*,#5037,.F.);
#6600=ORIENTED_EDGE('',*,*,#5042,.F.);
#6601=ORIENTED_EDGE('',*,*,#5043,.T.);
#6602=ORIENTED_EDGE('',*,*,#5044,.T.);
#6603=ORIENTED_EDGE('',*,*,#5040,.F.);
#6604=ORIENTED_EDGE('',*,*,#5045,.F.);
#6605=ORIENTED_EDGE('',*,*,#5046,.T.);
#6606=ORIENTED_EDGE('',*,*,#5047,.T.);
#6607=ORIENTED_EDGE('',*,*,#5043,.F.);
#6608=ORIENTED_EDGE('',*,*,#5048,.F.);
#6609=ORIENTED_EDGE('',*,*,#5049,.T.);
#6610=ORIENTED_EDGE('',*,*,#5050,.T.);
#6611=ORIENTED_EDGE('',*,*,#5046,.F.);
#6612=ORIENTED_EDGE('',*,*,#5051,.F.);
#6613=ORIENTED_EDGE('',*,*,#5052,.T.);
#6614=ORIENTED_EDGE('',*,*,#5053,.T.);
#6615=ORIENTED_EDGE('',*,*,#5049,.F.);
#6616=ORIENTED_EDGE('',*,*,#5054,.F.);
#6617=ORIENTED_EDGE('',*,*,#5055,.T.);
#6618=ORIENTED_EDGE('',*,*,#5056,.T.);
#6619=ORIENTED_EDGE('',*,*,#5052,.F.);
#6620=ORIENTED_EDGE('',*,*,#5057,.F.);
#6621=ORIENTED_EDGE('',*,*,#5058,.T.);
#6622=ORIENTED_EDGE('',*,*,#5059,.T.);
#6623=ORIENTED_EDGE('',*,*,#5055,.F.);
#6624=ORIENTED_EDGE('',*,*,#5060,.F.);
#6625=ORIENTED_EDGE('',*,*,#5061,.T.);
#6626=ORIENTED_EDGE('',*,*,#5062,.T.);
#6627=ORIENTED_EDGE('',*,*,#5058,.F.);
#6628=ORIENTED_EDGE('',*,*,#5063,.F.);
#6629=ORIENTED_EDGE('',*,*,#5064,.T.);
#6630=ORIENTED_EDGE('',*,*,#5065,.T.);
#6631=ORIENTED_EDGE('',*,*,#5061,.F.);
#6632=ORIENTED_EDGE('',*,*,#5066,.F.);
#6633=ORIENTED_EDGE('',*,*,#5067,.T.);
#6634=ORIENTED_EDGE('',*,*,#5068,.T.);
#6635=ORIENTED_EDGE('',*,*,#5064,.F.);
#6636=ORIENTED_EDGE('',*,*,#5069,.F.);
#6637=ORIENTED_EDGE('',*,*,#5070,.T.);
#6638=ORIENTED_EDGE('',*,*,#5071,.T.);
#6639=ORIENTED_EDGE('',*,*,#5067,.F.);
#6640=ORIENTED_EDGE('',*,*,#5072,.F.);
#6641=ORIENTED_EDGE('',*,*,#5073,.F.);
#6642=ORIENTED_EDGE('',*,*,#5074,.F.);
#6643=ORIENTED_EDGE('',*,*,#5075,.F.);
#6644=ORIENTED_EDGE('',*,*,#5076,.T.);
#6645=ORIENTED_EDGE('',*,*,#5077,.T.);
#6646=ORIENTED_EDGE('',*,*,#5078,.T.);
#6647=ORIENTED_EDGE('',*,*,#5079,.T.);
#6648=ORIENTED_EDGE('',*,*,#5080,.T.);
#6649=ORIENTED_EDGE('',*,*,#5081,.T.);
#6650=ORIENTED_EDGE('',*,*,#5082,.T.);
#6651=ORIENTED_EDGE('',*,*,#5081,.F.);
#6652=ORIENTED_EDGE('',*,*,#5083,.T.);
#6653=ORIENTED_EDGE('',*,*,#5084,.T.);
#6654=ORIENTED_EDGE('',*,*,#5085,.T.);
#6655=ORIENTED_EDGE('',*,*,#5077,.F.);
#6656=ORIENTED_EDGE('',*,*,#5086,.T.);
#6657=ORIENTED_EDGE('',*,*,#5087,.T.);
#6658=ORIENTED_EDGE('',*,*,#5088,.T.);
#6659=ORIENTED_EDGE('',*,*,#5084,.F.);
#6660=ORIENTED_EDGE('',*,*,#5089,.T.);
#6661=ORIENTED_EDGE('',*,*,#5090,.T.);
#6662=ORIENTED_EDGE('',*,*,#5091,.T.);
#6663=ORIENTED_EDGE('',*,*,#5087,.F.);
#6664=ORIENTED_EDGE('',*,*,#5092,.T.);
#6665=ORIENTED_EDGE('',*,*,#5093,.T.);
#6666=ORIENTED_EDGE('',*,*,#5094,.T.);
#6667=ORIENTED_EDGE('',*,*,#5090,.F.);
#6668=ORIENTED_EDGE('',*,*,#5095,.T.);
#6669=ORIENTED_EDGE('',*,*,#5096,.T.);
#6670=ORIENTED_EDGE('',*,*,#5097,.T.);
#6671=ORIENTED_EDGE('',*,*,#5093,.F.);
#6672=ORIENTED_EDGE('',*,*,#5098,.T.);
#6673=ORIENTED_EDGE('',*,*,#5099,.T.);
#6674=ORIENTED_EDGE('',*,*,#5100,.T.);
#6675=ORIENTED_EDGE('',*,*,#5096,.F.);
#6676=ORIENTED_EDGE('',*,*,#5101,.T.);
#6677=ORIENTED_EDGE('',*,*,#5102,.T.);
#6678=ORIENTED_EDGE('',*,*,#5103,.T.);
#6679=ORIENTED_EDGE('',*,*,#5099,.F.);
#6680=ORIENTED_EDGE('',*,*,#5104,.T.);
#6681=ORIENTED_EDGE('',*,*,#5105,.T.);
#6682=ORIENTED_EDGE('',*,*,#5106,.T.);
#6683=ORIENTED_EDGE('',*,*,#5102,.F.);
#6684=ORIENTED_EDGE('',*,*,#5107,.T.);
#6685=ORIENTED_EDGE('',*,*,#5108,.T.);
#6686=ORIENTED_EDGE('',*,*,#5109,.T.);
#6687=ORIENTED_EDGE('',*,*,#5105,.F.);
#6688=ORIENTED_EDGE('',*,*,#5110,.T.);
#6689=ORIENTED_EDGE('',*,*,#5111,.T.);
#6690=ORIENTED_EDGE('',*,*,#5112,.T.);
#6691=ORIENTED_EDGE('',*,*,#5108,.F.);
#6692=ORIENTED_EDGE('',*,*,#5113,.T.);
#6693=ORIENTED_EDGE('',*,*,#5114,.T.);
#6694=ORIENTED_EDGE('',*,*,#5115,.T.);
#6695=ORIENTED_EDGE('',*,*,#5111,.F.);
#6696=ORIENTED_EDGE('',*,*,#5116,.T.);
#6697=ORIENTED_EDGE('',*,*,#5117,.T.);
#6698=ORIENTED_EDGE('',*,*,#5118,.T.);
#6699=ORIENTED_EDGE('',*,*,#5114,.F.);
#6700=ORIENTED_EDGE('',*,*,#5119,.T.);
#6701=ORIENTED_EDGE('',*,*,#5120,.T.);
#6702=ORIENTED_EDGE('',*,*,#5121,.T.);
#6703=ORIENTED_EDGE('',*,*,#5117,.F.);
#6704=ORIENTED_EDGE('',*,*,#5122,.T.);
#6705=ORIENTED_EDGE('',*,*,#5123,.F.);
#6706=ORIENTED_EDGE('',*,*,#5124,.T.);
#6707=ORIENTED_EDGE('',*,*,#5125,.F.);
#6708=ORIENTED_EDGE('',*,*,#5126,.T.);
#6709=ORIENTED_EDGE('',*,*,#5127,.T.);
#6710=ORIENTED_EDGE('',*,*,#5128,.T.);
#6711=ORIENTED_EDGE('',*,*,#5129,.F.);
#6712=ORIENTED_EDGE('',*,*,#5130,.F.);
#6713=ORIENTED_EDGE('',*,*,#5131,.T.);
#6714=ORIENTED_EDGE('',*,*,#5132,.T.);
#6715=ORIENTED_EDGE('',*,*,#5127,.F.);
#6716=ORIENTED_EDGE('',*,*,#5133,.F.);
#6717=ORIENTED_EDGE('',*,*,#5134,.T.);
#6718=ORIENTED_EDGE('',*,*,#5135,.T.);
#6719=ORIENTED_EDGE('',*,*,#5131,.F.);
#6720=ORIENTED_EDGE('',*,*,#5136,.F.);
#6721=ORIENTED_EDGE('',*,*,#5137,.T.);
#6722=ORIENTED_EDGE('',*,*,#5138,.T.);
#6723=ORIENTED_EDGE('',*,*,#5134,.F.);
#6724=ORIENTED_EDGE('',*,*,#5139,.F.);
#6725=ORIENTED_EDGE('',*,*,#5140,.T.);
#6726=ORIENTED_EDGE('',*,*,#5141,.T.);
#6727=ORIENTED_EDGE('',*,*,#5137,.F.);
#6728=ORIENTED_EDGE('',*,*,#5142,.F.);
#6729=ORIENTED_EDGE('',*,*,#5143,.T.);
#6730=ORIENTED_EDGE('',*,*,#5144,.T.);
#6731=ORIENTED_EDGE('',*,*,#5140,.F.);
#6732=ORIENTED_EDGE('',*,*,#5145,.F.);
#6733=ORIENTED_EDGE('',*,*,#5146,.T.);
#6734=ORIENTED_EDGE('',*,*,#5147,.T.);
#6735=ORIENTED_EDGE('',*,*,#5143,.F.);
#6736=ORIENTED_EDGE('',*,*,#5148,.F.);
#6737=ORIENTED_EDGE('',*,*,#5149,.T.);
#6738=ORIENTED_EDGE('',*,*,#5150,.T.);
#6739=ORIENTED_EDGE('',*,*,#5146,.F.);
#6740=ORIENTED_EDGE('',*,*,#5151,.F.);
#6741=ORIENTED_EDGE('',*,*,#5152,.T.);
#6742=ORIENTED_EDGE('',*,*,#5153,.T.);
#6743=ORIENTED_EDGE('',*,*,#5149,.F.);
#6744=ORIENTED_EDGE('',*,*,#5154,.F.);
#6745=ORIENTED_EDGE('',*,*,#5155,.T.);
#6746=ORIENTED_EDGE('',*,*,#5156,.T.);
#6747=ORIENTED_EDGE('',*,*,#5152,.F.);
#6748=ORIENTED_EDGE('',*,*,#5157,.F.);
#6749=ORIENTED_EDGE('',*,*,#5158,.T.);
#6750=ORIENTED_EDGE('',*,*,#5159,.T.);
#6751=ORIENTED_EDGE('',*,*,#5155,.F.);
#6752=ORIENTED_EDGE('',*,*,#5160,.F.);
#6753=ORIENTED_EDGE('',*,*,#5161,.T.);
#6754=ORIENTED_EDGE('',*,*,#5162,.T.);
#6755=ORIENTED_EDGE('',*,*,#5158,.F.);
#6756=ORIENTED_EDGE('',*,*,#5163,.F.);
#6757=ORIENTED_EDGE('',*,*,#5164,.T.);
#6758=ORIENTED_EDGE('',*,*,#5165,.T.);
#6759=ORIENTED_EDGE('',*,*,#5161,.F.);
#6760=ORIENTED_EDGE('',*,*,#5166,.F.);
#6761=ORIENTED_EDGE('',*,*,#5167,.T.);
#6762=ORIENTED_EDGE('',*,*,#5168,.T.);
#6763=ORIENTED_EDGE('',*,*,#5164,.F.);
#6764=ORIENTED_EDGE('',*,*,#5169,.F.);
#6765=ORIENTED_EDGE('',*,*,#5170,.T.);
#6766=ORIENTED_EDGE('',*,*,#5171,.T.);
#6767=ORIENTED_EDGE('',*,*,#5167,.F.);
#6768=ORIENTED_EDGE('',*,*,#5172,.F.);
#6769=ORIENTED_EDGE('',*,*,#5173,.F.);
#6770=ORIENTED_EDGE('',*,*,#5174,.F.);
#6771=ORIENTED_EDGE('',*,*,#5175,.F.);
#6772=ORIENTED_EDGE('',*,*,#5176,.T.);
#6773=ORIENTED_EDGE('',*,*,#5177,.T.);
#6774=ORIENTED_EDGE('',*,*,#5178,.T.);
#6775=ORIENTED_EDGE('',*,*,#5179,.T.);
#6776=ORIENTED_EDGE('',*,*,#5180,.T.);
#6777=ORIENTED_EDGE('',*,*,#5181,.T.);
#6778=ORIENTED_EDGE('',*,*,#5182,.T.);
#6779=ORIENTED_EDGE('',*,*,#5181,.F.);
#6780=ORIENTED_EDGE('',*,*,#5183,.T.);
#6781=ORIENTED_EDGE('',*,*,#5184,.T.);
#6782=ORIENTED_EDGE('',*,*,#5185,.T.);
#6783=ORIENTED_EDGE('',*,*,#5177,.F.);
#6784=ORIENTED_EDGE('',*,*,#5186,.T.);
#6785=ORIENTED_EDGE('',*,*,#5187,.T.);
#6786=ORIENTED_EDGE('',*,*,#5188,.T.);
#6787=ORIENTED_EDGE('',*,*,#5184,.F.);
#6788=ORIENTED_EDGE('',*,*,#5189,.T.);
#6789=ORIENTED_EDGE('',*,*,#5190,.T.);
#6790=ORIENTED_EDGE('',*,*,#5191,.T.);
#6791=ORIENTED_EDGE('',*,*,#5187,.F.);
#6792=ORIENTED_EDGE('',*,*,#5192,.T.);
#6793=ORIENTED_EDGE('',*,*,#5193,.T.);
#6794=ORIENTED_EDGE('',*,*,#5194,.T.);
#6795=ORIENTED_EDGE('',*,*,#5190,.F.);
#6796=ORIENTED_EDGE('',*,*,#5195,.T.);
#6797=ORIENTED_EDGE('',*,*,#5196,.T.);
#6798=ORIENTED_EDGE('',*,*,#5197,.T.);
#6799=ORIENTED_EDGE('',*,*,#5193,.F.);
#6800=ORIENTED_EDGE('',*,*,#5198,.T.);
#6801=ORIENTED_EDGE('',*,*,#5199,.T.);
#6802=ORIENTED_EDGE('',*,*,#5200,.T.);
#6803=ORIENTED_EDGE('',*,*,#5196,.F.);
#6804=ORIENTED_EDGE('',*,*,#5201,.T.);
#6805=ORIENTED_EDGE('',*,*,#5202,.T.);
#6806=ORIENTED_EDGE('',*,*,#5203,.T.);
#6807=ORIENTED_EDGE('',*,*,#5199,.F.);
#6808=ORIENTED_EDGE('',*,*,#5204,.T.);
#6809=ORIENTED_EDGE('',*,*,#5205,.T.);
#6810=ORIENTED_EDGE('',*,*,#5206,.T.);
#6811=ORIENTED_EDGE('',*,*,#5202,.F.);
#6812=ORIENTED_EDGE('',*,*,#5207,.T.);
#6813=ORIENTED_EDGE('',*,*,#5208,.T.);
#6814=ORIENTED_EDGE('',*,*,#5209,.T.);
#6815=ORIENTED_EDGE('',*,*,#5205,.F.);
#6816=ORIENTED_EDGE('',*,*,#5210,.T.);
#6817=ORIENTED_EDGE('',*,*,#5211,.T.);
#6818=ORIENTED_EDGE('',*,*,#5212,.T.);
#6819=ORIENTED_EDGE('',*,*,#5208,.F.);
#6820=ORIENTED_EDGE('',*,*,#5213,.T.);
#6821=ORIENTED_EDGE('',*,*,#5214,.T.);
#6822=ORIENTED_EDGE('',*,*,#5215,.T.);
#6823=ORIENTED_EDGE('',*,*,#5211,.F.);
#6824=ORIENTED_EDGE('',*,*,#5216,.T.);
#6825=ORIENTED_EDGE('',*,*,#5217,.T.);
#6826=ORIENTED_EDGE('',*,*,#5218,.T.);
#6827=ORIENTED_EDGE('',*,*,#5214,.F.);
#6828=ORIENTED_EDGE('',*,*,#5219,.T.);
#6829=ORIENTED_EDGE('',*,*,#5220,.T.);
#6830=ORIENTED_EDGE('',*,*,#5221,.T.);
#6831=ORIENTED_EDGE('',*,*,#5217,.F.);
#6832=ORIENTED_EDGE('',*,*,#5222,.T.);
#6833=ORIENTED_EDGE('',*,*,#5223,.F.);
#6834=ORIENTED_EDGE('',*,*,#5224,.T.);
#6835=ORIENTED_EDGE('',*,*,#5225,.F.);
#6836=ORIENTED_EDGE('',*,*,#5226,.T.);
#6837=ORIENTED_EDGE('',*,*,#5227,.T.);
#6838=ORIENTED_EDGE('',*,*,#5228,.T.);
#6839=ORIENTED_EDGE('',*,*,#5229,.F.);
#6840=ORIENTED_EDGE('',*,*,#5230,.F.);
#6841=ORIENTED_EDGE('',*,*,#5231,.T.);
#6842=ORIENTED_EDGE('',*,*,#5232,.T.);
#6843=ORIENTED_EDGE('',*,*,#5227,.F.);
#6844=ORIENTED_EDGE('',*,*,#5233,.F.);
#6845=ORIENTED_EDGE('',*,*,#5234,.T.);
#6846=ORIENTED_EDGE('',*,*,#5235,.T.);
#6847=ORIENTED_EDGE('',*,*,#5231,.F.);
#6848=ORIENTED_EDGE('',*,*,#5236,.F.);
#6849=ORIENTED_EDGE('',*,*,#5237,.T.);
#6850=ORIENTED_EDGE('',*,*,#5238,.T.);
#6851=ORIENTED_EDGE('',*,*,#5234,.F.);
#6852=ORIENTED_EDGE('',*,*,#5239,.F.);
#6853=ORIENTED_EDGE('',*,*,#5240,.T.);
#6854=ORIENTED_EDGE('',*,*,#5241,.T.);
#6855=ORIENTED_EDGE('',*,*,#5237,.F.);
#6856=ORIENTED_EDGE('',*,*,#5242,.F.);
#6857=ORIENTED_EDGE('',*,*,#5243,.T.);
#6858=ORIENTED_EDGE('',*,*,#5244,.T.);
#6859=ORIENTED_EDGE('',*,*,#5240,.F.);
#6860=ORIENTED_EDGE('',*,*,#5245,.F.);
#6861=ORIENTED_EDGE('',*,*,#5246,.T.);
#6862=ORIENTED_EDGE('',*,*,#5247,.T.);
#6863=ORIENTED_EDGE('',*,*,#5243,.F.);
#6864=ORIENTED_EDGE('',*,*,#5248,.F.);
#6865=ORIENTED_EDGE('',*,*,#5249,.T.);
#6866=ORIENTED_EDGE('',*,*,#5250,.T.);
#6867=ORIENTED_EDGE('',*,*,#5246,.F.);
#6868=ORIENTED_EDGE('',*,*,#5251,.F.);
#6869=ORIENTED_EDGE('',*,*,#5252,.T.);
#6870=ORIENTED_EDGE('',*,*,#5253,.T.);
#6871=ORIENTED_EDGE('',*,*,#5249,.F.);
#6872=ORIENTED_EDGE('',*,*,#5254,.F.);
#6873=ORIENTED_EDGE('',*,*,#5255,.T.);
#6874=ORIENTED_EDGE('',*,*,#5256,.T.);
#6875=ORIENTED_EDGE('',*,*,#5252,.F.);
#6876=ORIENTED_EDGE('',*,*,#5257,.F.);
#6877=ORIENTED_EDGE('',*,*,#5258,.T.);
#6878=ORIENTED_EDGE('',*,*,#5259,.T.);
#6879=ORIENTED_EDGE('',*,*,#5255,.F.);
#6880=ORIENTED_EDGE('',*,*,#5260,.F.);
#6881=ORIENTED_EDGE('',*,*,#5261,.T.);
#6882=ORIENTED_EDGE('',*,*,#5262,.T.);
#6883=ORIENTED_EDGE('',*,*,#5258,.F.);
#6884=ORIENTED_EDGE('',*,*,#5263,.F.);
#6885=ORIENTED_EDGE('',*,*,#5264,.T.);
#6886=ORIENTED_EDGE('',*,*,#5265,.T.);
#6887=ORIENTED_EDGE('',*,*,#5261,.F.);
#6888=ORIENTED_EDGE('',*,*,#5266,.F.);
#6889=ORIENTED_EDGE('',*,*,#5267,.T.);
#6890=ORIENTED_EDGE('',*,*,#5268,.T.);
#6891=ORIENTED_EDGE('',*,*,#5264,.F.);
#6892=ORIENTED_EDGE('',*,*,#5269,.F.);
#6893=ORIENTED_EDGE('',*,*,#5270,.T.);
#6894=ORIENTED_EDGE('',*,*,#5271,.T.);
#6895=ORIENTED_EDGE('',*,*,#5267,.F.);
#6896=ORIENTED_EDGE('',*,*,#5272,.F.);
#6897=ORIENTED_EDGE('',*,*,#5273,.F.);
#6898=ORIENTED_EDGE('',*,*,#5274,.F.);
#6899=ORIENTED_EDGE('',*,*,#5275,.F.);
#6900=ORIENTED_EDGE('',*,*,#5276,.T.);
#6901=ORIENTED_EDGE('',*,*,#5277,.T.);
#6902=ORIENTED_EDGE('',*,*,#5278,.T.);
#6903=ORIENTED_EDGE('',*,*,#5279,.T.);
#6904=ORIENTED_EDGE('',*,*,#5280,.F.);
#6905=ORIENTED_EDGE('',*,*,#5281,.T.);
#6906=ORIENTED_EDGE('',*,*,#5282,.T.);
#6907=ORIENTED_EDGE('',*,*,#5283,.T.);
#6908=ORIENTED_EDGE('',*,*,#5284,.T.);
#6909=ORIENTED_EDGE('',*,*,#5277,.F.);
#6910=ORIENTED_EDGE('',*,*,#5285,.T.);
#6911=ORIENTED_EDGE('',*,*,#5286,.T.);
#6912=ORIENTED_EDGE('',*,*,#5287,.T.);
#6913=ORIENTED_EDGE('',*,*,#5283,.F.);
#6914=ORIENTED_EDGE('',*,*,#5288,.T.);
#6915=ORIENTED_EDGE('',*,*,#5289,.T.);
#6916=ORIENTED_EDGE('',*,*,#5290,.T.);
#6917=ORIENTED_EDGE('',*,*,#5286,.F.);
#6918=ORIENTED_EDGE('',*,*,#5291,.T.);
#6919=ORIENTED_EDGE('',*,*,#5292,.T.);
#6920=ORIENTED_EDGE('',*,*,#5293,.T.);
#6921=ORIENTED_EDGE('',*,*,#5289,.F.);
#6922=ORIENTED_EDGE('',*,*,#5294,.T.);
#6923=ORIENTED_EDGE('',*,*,#5295,.T.);
#6924=ORIENTED_EDGE('',*,*,#5296,.T.);
#6925=ORIENTED_EDGE('',*,*,#5292,.F.);
#6926=ORIENTED_EDGE('',*,*,#5297,.T.);
#6927=ORIENTED_EDGE('',*,*,#5298,.T.);
#6928=ORIENTED_EDGE('',*,*,#5299,.T.);
#6929=ORIENTED_EDGE('',*,*,#5295,.F.);
#6930=ORIENTED_EDGE('',*,*,#5300,.T.);
#6931=ORIENTED_EDGE('',*,*,#5301,.T.);
#6932=ORIENTED_EDGE('',*,*,#5302,.T.);
#6933=ORIENTED_EDGE('',*,*,#5298,.F.);
#6934=ORIENTED_EDGE('',*,*,#5303,.T.);
#6935=ORIENTED_EDGE('',*,*,#5304,.T.);
#6936=ORIENTED_EDGE('',*,*,#5305,.T.);
#6937=ORIENTED_EDGE('',*,*,#5301,.F.);
#6938=ORIENTED_EDGE('',*,*,#5306,.T.);
#6939=ORIENTED_EDGE('',*,*,#5307,.T.);
#6940=ORIENTED_EDGE('',*,*,#5308,.T.);
#6941=ORIENTED_EDGE('',*,*,#5304,.F.);
#6942=ORIENTED_EDGE('',*,*,#5309,.T.);
#6943=ORIENTED_EDGE('',*,*,#5310,.T.);
#6944=ORIENTED_EDGE('',*,*,#5311,.T.);
#6945=ORIENTED_EDGE('',*,*,#5307,.F.);
#6946=ORIENTED_EDGE('',*,*,#5312,.T.);
#6947=ORIENTED_EDGE('',*,*,#5313,.T.);
#6948=ORIENTED_EDGE('',*,*,#5314,.T.);
#6949=ORIENTED_EDGE('',*,*,#5310,.F.);
#6950=ORIENTED_EDGE('',*,*,#5315,.T.);
#6951=ORIENTED_EDGE('',*,*,#5316,.T.);
#6952=ORIENTED_EDGE('',*,*,#5317,.T.);
#6953=ORIENTED_EDGE('',*,*,#5313,.F.);
#6954=ORIENTED_EDGE('',*,*,#5318,.T.);
#6955=ORIENTED_EDGE('',*,*,#5319,.T.);
#6956=ORIENTED_EDGE('',*,*,#5320,.T.);
#6957=ORIENTED_EDGE('',*,*,#5316,.F.);
#6958=ORIENTED_EDGE('',*,*,#5321,.T.);
#6959=ORIENTED_EDGE('',*,*,#5322,.F.);
#6960=ORIENTED_EDGE('',*,*,#5323,.T.);
#6961=ORIENTED_EDGE('',*,*,#5324,.F.);
#6962=ORIENTED_EDGE('',*,*,#5325,.T.);
#6963=ORIENTED_EDGE('',*,*,#5326,.T.);
#6964=ORIENTED_EDGE('',*,*,#5327,.T.);
#6965=ORIENTED_EDGE('',*,*,#5328,.T.);
#6966=ORIENTED_EDGE('',*,*,#5329,.F.);
#6967=ORIENTED_EDGE('',*,*,#5330,.T.);
#6968=ORIENTED_EDGE('',*,*,#5331,.T.);
#6969=ORIENTED_EDGE('',*,*,#5332,.T.);
#6970=ORIENTED_EDGE('',*,*,#5333,.T.);
#6971=ORIENTED_EDGE('',*,*,#5326,.F.);
#6972=ORIENTED_EDGE('',*,*,#5334,.T.);
#6973=ORIENTED_EDGE('',*,*,#5335,.T.);
#6974=ORIENTED_EDGE('',*,*,#5336,.T.);
#6975=ORIENTED_EDGE('',*,*,#5332,.F.);
#6976=ORIENTED_EDGE('',*,*,#5337,.T.);
#6977=ORIENTED_EDGE('',*,*,#5338,.T.);
#6978=ORIENTED_EDGE('',*,*,#5339,.T.);
#6979=ORIENTED_EDGE('',*,*,#5335,.F.);
#6980=ORIENTED_EDGE('',*,*,#5340,.T.);
#6981=ORIENTED_EDGE('',*,*,#5341,.T.);
#6982=ORIENTED_EDGE('',*,*,#5342,.T.);
#6983=ORIENTED_EDGE('',*,*,#5338,.F.);
#6984=ORIENTED_EDGE('',*,*,#5343,.T.);
#6985=ORIENTED_EDGE('',*,*,#5344,.T.);
#6986=ORIENTED_EDGE('',*,*,#5345,.T.);
#6987=ORIENTED_EDGE('',*,*,#5341,.F.);
#6988=ORIENTED_EDGE('',*,*,#5346,.T.);
#6989=ORIENTED_EDGE('',*,*,#5347,.T.);
#6990=ORIENTED_EDGE('',*,*,#5348,.T.);
#6991=ORIENTED_EDGE('',*,*,#5344,.F.);
#6992=ORIENTED_EDGE('',*,*,#5349,.T.);
#6993=ORIENTED_EDGE('',*,*,#5350,.T.);
#6994=ORIENTED_EDGE('',*,*,#5351,.T.);
#6995=ORIENTED_EDGE('',*,*,#5347,.F.);
#6996=ORIENTED_EDGE('',*,*,#5352,.T.);
#6997=ORIENTED_EDGE('',*,*,#5353,.T.);
#6998=ORIENTED_EDGE('',*,*,#5354,.T.);
#6999=ORIENTED_EDGE('',*,*,#5350,.F.);
#7000=ORIENTED_EDGE('',*,*,#5355,.T.);
#7001=ORIENTED_EDGE('',*,*,#5356,.T.);
#7002=ORIENTED_EDGE('',*,*,#5357,.T.);
#7003=ORIENTED_EDGE('',*,*,#5353,.F.);
#7004=ORIENTED_EDGE('',*,*,#5358,.T.);
#7005=ORIENTED_EDGE('',*,*,#5359,.T.);
#7006=ORIENTED_EDGE('',*,*,#5360,.T.);
#7007=ORIENTED_EDGE('',*,*,#5356,.F.);
#7008=ORIENTED_EDGE('',*,*,#5361,.T.);
#7009=ORIENTED_EDGE('',*,*,#5362,.T.);
#7010=ORIENTED_EDGE('',*,*,#5363,.T.);
#7011=ORIENTED_EDGE('',*,*,#5359,.F.);
#7012=ORIENTED_EDGE('',*,*,#5364,.T.);
#7013=ORIENTED_EDGE('',*,*,#5365,.T.);
#7014=ORIENTED_EDGE('',*,*,#5366,.T.);
#7015=ORIENTED_EDGE('',*,*,#5362,.F.);
#7016=ORIENTED_EDGE('',*,*,#5367,.T.);
#7017=ORIENTED_EDGE('',*,*,#5368,.T.);
#7018=ORIENTED_EDGE('',*,*,#5369,.T.);
#7019=ORIENTED_EDGE('',*,*,#5365,.F.);
#7020=ORIENTED_EDGE('',*,*,#5370,.T.);
#7021=ORIENTED_EDGE('',*,*,#5371,.F.);
#7022=ORIENTED_EDGE('',*,*,#5372,.T.);
#7023=ORIENTED_EDGE('',*,*,#5373,.F.);
#7024=ORIENTED_EDGE('',*,*,#5374,.T.);
#7025=ORIENTED_EDGE('',*,*,#5375,.T.);
#7026=ORIENTED_EDGE('',*,*,#5376,.T.);
#7027=ORIENTED_EDGE('',*,*,#5377,.F.);
#7028=ORIENTED_EDGE('',*,*,#5378,.F.);
#7029=ORIENTED_EDGE('',*,*,#5379,.T.);
#7030=ORIENTED_EDGE('',*,*,#5380,.T.);
#7031=ORIENTED_EDGE('',*,*,#5375,.F.);
#7032=ORIENTED_EDGE('',*,*,#5381,.F.);
#7033=ORIENTED_EDGE('',*,*,#5382,.T.);
#7034=ORIENTED_EDGE('',*,*,#5383,.T.);
#7035=ORIENTED_EDGE('',*,*,#5379,.F.);
#7036=ORIENTED_EDGE('',*,*,#5384,.F.);
#7037=ORIENTED_EDGE('',*,*,#5385,.T.);
#7038=ORIENTED_EDGE('',*,*,#5386,.T.);
#7039=ORIENTED_EDGE('',*,*,#5382,.F.);
#7040=ORIENTED_EDGE('',*,*,#5387,.F.);
#7041=ORIENTED_EDGE('',*,*,#5388,.T.);
#7042=ORIENTED_EDGE('',*,*,#5389,.T.);
#7043=ORIENTED_EDGE('',*,*,#5385,.F.);
#7044=ORIENTED_EDGE('',*,*,#5390,.F.);
#7045=ORIENTED_EDGE('',*,*,#5391,.T.);
#7046=ORIENTED_EDGE('',*,*,#5392,.T.);
#7047=ORIENTED_EDGE('',*,*,#5388,.F.);
#7048=ORIENTED_EDGE('',*,*,#5393,.F.);
#7049=ORIENTED_EDGE('',*,*,#5394,.T.);
#7050=ORIENTED_EDGE('',*,*,#5395,.T.);
#7051=ORIENTED_EDGE('',*,*,#5391,.F.);
#7052=ORIENTED_EDGE('',*,*,#5396,.F.);
#7053=ORIENTED_EDGE('',*,*,#5397,.T.);
#7054=ORIENTED_EDGE('',*,*,#5398,.T.);
#7055=ORIENTED_EDGE('',*,*,#5394,.F.);
#7056=ORIENTED_EDGE('',*,*,#5399,.F.);
#7057=ORIENTED_EDGE('',*,*,#5400,.T.);
#7058=ORIENTED_EDGE('',*,*,#5401,.T.);
#7059=ORIENTED_EDGE('',*,*,#5397,.F.);
#7060=ORIENTED_EDGE('',*,*,#5402,.F.);
#7061=ORIENTED_EDGE('',*,*,#5403,.T.);
#7062=ORIENTED_EDGE('',*,*,#5404,.T.);
#7063=ORIENTED_EDGE('',*,*,#5400,.F.);
#7064=ORIENTED_EDGE('',*,*,#5405,.F.);
#7065=ORIENTED_EDGE('',*,*,#5406,.T.);
#7066=ORIENTED_EDGE('',*,*,#5407,.T.);
#7067=ORIENTED_EDGE('',*,*,#5403,.F.);
#7068=ORIENTED_EDGE('',*,*,#5408,.F.);
#7069=ORIENTED_EDGE('',*,*,#5409,.T.);
#7070=ORIENTED_EDGE('',*,*,#5410,.T.);
#7071=ORIENTED_EDGE('',*,*,#5406,.F.);
#7072=ORIENTED_EDGE('',*,*,#5411,.F.);
#7073=ORIENTED_EDGE('',*,*,#5412,.T.);
#7074=ORIENTED_EDGE('',*,*,#5413,.T.);
#7075=ORIENTED_EDGE('',*,*,#5409,.F.);
#7076=ORIENTED_EDGE('',*,*,#5414,.F.);
#7077=ORIENTED_EDGE('',*,*,#5415,.T.);
#7078=ORIENTED_EDGE('',*,*,#5416,.T.);
#7079=ORIENTED_EDGE('',*,*,#5412,.F.);
#7080=ORIENTED_EDGE('',*,*,#5417,.F.);
#7081=ORIENTED_EDGE('',*,*,#5418,.F.);
#7082=ORIENTED_EDGE('',*,*,#5419,.F.);
#7083=ORIENTED_EDGE('',*,*,#5420,.F.);
#7084=ORIENTED_EDGE('',*,*,#5421,.T.);
#7085=ORIENTED_EDGE('',*,*,#5422,.T.);
#7086=ORIENTED_EDGE('',*,*,#5423,.T.);
#7087=ORIENTED_EDGE('',*,*,#5424,.F.);
#7088=ORIENTED_EDGE('',*,*,#5425,.F.);
#7089=ORIENTED_EDGE('',*,*,#5426,.T.);
#7090=ORIENTED_EDGE('',*,*,#5427,.T.);
#7091=ORIENTED_EDGE('',*,*,#5422,.F.);
#7092=ORIENTED_EDGE('',*,*,#5428,.F.);
#7093=ORIENTED_EDGE('',*,*,#5429,.T.);
#7094=ORIENTED_EDGE('',*,*,#5430,.T.);
#7095=ORIENTED_EDGE('',*,*,#5426,.F.);
#7096=ORIENTED_EDGE('',*,*,#5431,.F.);
#7097=ORIENTED_EDGE('',*,*,#5432,.T.);
#7098=ORIENTED_EDGE('',*,*,#5433,.T.);
#7099=ORIENTED_EDGE('',*,*,#5429,.F.);
#7100=ORIENTED_EDGE('',*,*,#5434,.F.);
#7101=ORIENTED_EDGE('',*,*,#5435,.T.);
#7102=ORIENTED_EDGE('',*,*,#5436,.T.);
#7103=ORIENTED_EDGE('',*,*,#5432,.F.);
#7104=ORIENTED_EDGE('',*,*,#5437,.F.);
#7105=ORIENTED_EDGE('',*,*,#5438,.T.);
#7106=ORIENTED_EDGE('',*,*,#5439,.T.);
#7107=ORIENTED_EDGE('',*,*,#5435,.F.);
#7108=ORIENTED_EDGE('',*,*,#5440,.F.);
#7109=ORIENTED_EDGE('',*,*,#5441,.T.);
#7110=ORIENTED_EDGE('',*,*,#5442,.T.);
#7111=ORIENTED_EDGE('',*,*,#5438,.F.);
#7112=ORIENTED_EDGE('',*,*,#5443,.F.);
#7113=ORIENTED_EDGE('',*,*,#5444,.T.);
#7114=ORIENTED_EDGE('',*,*,#5445,.T.);
#7115=ORIENTED_EDGE('',*,*,#5441,.F.);
#7116=ORIENTED_EDGE('',*,*,#5446,.F.);
#7117=ORIENTED_EDGE('',*,*,#5447,.T.);
#7118=ORIENTED_EDGE('',*,*,#5448,.T.);
#7119=ORIENTED_EDGE('',*,*,#5444,.F.);
#7120=ORIENTED_EDGE('',*,*,#5449,.F.);
#7121=ORIENTED_EDGE('',*,*,#5450,.T.);
#7122=ORIENTED_EDGE('',*,*,#5451,.T.);
#7123=ORIENTED_EDGE('',*,*,#5447,.F.);
#7124=ORIENTED_EDGE('',*,*,#5452,.F.);
#7125=ORIENTED_EDGE('',*,*,#5453,.T.);
#7126=ORIENTED_EDGE('',*,*,#5454,.T.);
#7127=ORIENTED_EDGE('',*,*,#5450,.F.);
#7128=ORIENTED_EDGE('',*,*,#5455,.F.);
#7129=ORIENTED_EDGE('',*,*,#5456,.T.);
#7130=ORIENTED_EDGE('',*,*,#5457,.T.);
#7131=ORIENTED_EDGE('',*,*,#5453,.F.);
#7132=ORIENTED_EDGE('',*,*,#5458,.F.);
#7133=ORIENTED_EDGE('',*,*,#5459,.T.);
#7134=ORIENTED_EDGE('',*,*,#5460,.T.);
#7135=ORIENTED_EDGE('',*,*,#5456,.F.);
#7136=ORIENTED_EDGE('',*,*,#5461,.F.);
#7137=ORIENTED_EDGE('',*,*,#5462,.T.);
#7138=ORIENTED_EDGE('',*,*,#5463,.T.);
#7139=ORIENTED_EDGE('',*,*,#5459,.F.);
#7140=ORIENTED_EDGE('',*,*,#5464,.F.);
#7141=ORIENTED_EDGE('',*,*,#5465,.F.);
#7142=ORIENTED_EDGE('',*,*,#5466,.F.);
#7143=ORIENTED_EDGE('',*,*,#5467,.F.);
#7144=ORIENTED_EDGE('',*,*,#5468,.T.);
#7145=ORIENTED_EDGE('',*,*,#5469,.T.);
#7146=ORIENTED_EDGE('',*,*,#5470,.T.);
#7147=ORIENTED_EDGE('',*,*,#5471,.T.);
#7148=ORIENTED_EDGE('',*,*,#5472,.T.);
#7149=ORIENTED_EDGE('',*,*,#5473,.T.);
#7150=ORIENTED_EDGE('',*,*,#5472,.F.);
#7151=ORIENTED_EDGE('',*,*,#5474,.T.);
#7152=ORIENTED_EDGE('',*,*,#5475,.T.);
#7153=ORIENTED_EDGE('',*,*,#5476,.T.);
#7154=ORIENTED_EDGE('',*,*,#5477,.T.);
#7155=ORIENTED_EDGE('',*,*,#5469,.F.);
#7156=ORIENTED_EDGE('',*,*,#5478,.T.);
#7157=ORIENTED_EDGE('',*,*,#5479,.T.);
#7158=ORIENTED_EDGE('',*,*,#5480,.T.);
#7159=ORIENTED_EDGE('',*,*,#5476,.F.);
#7160=ORIENTED_EDGE('',*,*,#5481,.T.);
#7161=ORIENTED_EDGE('',*,*,#5482,.T.);
#7162=ORIENTED_EDGE('',*,*,#5483,.T.);
#7163=ORIENTED_EDGE('',*,*,#5479,.F.);
#7164=ORIENTED_EDGE('',*,*,#5484,.T.);
#7165=ORIENTED_EDGE('',*,*,#5485,.T.);
#7166=ORIENTED_EDGE('',*,*,#5486,.T.);
#7167=ORIENTED_EDGE('',*,*,#5482,.F.);
#7168=ORIENTED_EDGE('',*,*,#5487,.T.);
#7169=ORIENTED_EDGE('',*,*,#5488,.T.);
#7170=ORIENTED_EDGE('',*,*,#5489,.T.);
#7171=ORIENTED_EDGE('',*,*,#5485,.F.);
#7172=ORIENTED_EDGE('',*,*,#5490,.T.);
#7173=ORIENTED_EDGE('',*,*,#5491,.T.);
#7174=ORIENTED_EDGE('',*,*,#5492,.T.);
#7175=ORIENTED_EDGE('',*,*,#5488,.F.);
#7176=ORIENTED_EDGE('',*,*,#5493,.T.);
#7177=ORIENTED_EDGE('',*,*,#5494,.T.);
#7178=ORIENTED_EDGE('',*,*,#5495,.T.);
#7179=ORIENTED_EDGE('',*,*,#5491,.F.);
#7180=ORIENTED_EDGE('',*,*,#5496,.T.);
#7181=ORIENTED_EDGE('',*,*,#5497,.T.);
#7182=ORIENTED_EDGE('',*,*,#5498,.T.);
#7183=ORIENTED_EDGE('',*,*,#5494,.F.);
#7184=ORIENTED_EDGE('',*,*,#5499,.T.);
#7185=ORIENTED_EDGE('',*,*,#5500,.T.);
#7186=ORIENTED_EDGE('',*,*,#5501,.T.);
#7187=ORIENTED_EDGE('',*,*,#5497,.F.);
#7188=ORIENTED_EDGE('',*,*,#5502,.T.);
#7189=ORIENTED_EDGE('',*,*,#5503,.T.);
#7190=ORIENTED_EDGE('',*,*,#5504,.T.);
#7191=ORIENTED_EDGE('',*,*,#5500,.F.);
#7192=ORIENTED_EDGE('',*,*,#5505,.T.);
#7193=ORIENTED_EDGE('',*,*,#5506,.T.);
#7194=ORIENTED_EDGE('',*,*,#5507,.T.);
#7195=ORIENTED_EDGE('',*,*,#5503,.F.);
#7196=ORIENTED_EDGE('',*,*,#5508,.T.);
#7197=ORIENTED_EDGE('',*,*,#5509,.T.);
#7198=ORIENTED_EDGE('',*,*,#5510,.T.);
#7199=ORIENTED_EDGE('',*,*,#5506,.F.);
#7200=ORIENTED_EDGE('',*,*,#5511,.T.);
#7201=ORIENTED_EDGE('',*,*,#5512,.T.);
#7202=ORIENTED_EDGE('',*,*,#5513,.T.);
#7203=ORIENTED_EDGE('',*,*,#5509,.F.);
#7204=ORIENTED_EDGE('',*,*,#5514,.T.);
#7205=ORIENTED_EDGE('',*,*,#5515,.F.);
#7206=ORIENTED_EDGE('',*,*,#5516,.T.);
#7207=ORIENTED_EDGE('',*,*,#5517,.F.);
#7208=ORIENTED_EDGE('',*,*,#5518,.T.);
#7209=ORIENTED_EDGE('',*,*,#5519,.T.);
#7210=ORIENTED_EDGE('',*,*,#5520,.T.);
#7211=ORIENTED_EDGE('',*,*,#5521,.F.);
#7212=ORIENTED_EDGE('',*,*,#5522,.F.);
#7213=ORIENTED_EDGE('',*,*,#5523,.T.);
#7214=ORIENTED_EDGE('',*,*,#5524,.T.);
#7215=ORIENTED_EDGE('',*,*,#5519,.F.);
#7216=ORIENTED_EDGE('',*,*,#5525,.F.);
#7217=ORIENTED_EDGE('',*,*,#5526,.T.);
#7218=ORIENTED_EDGE('',*,*,#5527,.T.);
#7219=ORIENTED_EDGE('',*,*,#5523,.F.);
#7220=ORIENTED_EDGE('',*,*,#5528,.F.);
#7221=ORIENTED_EDGE('',*,*,#5529,.T.);
#7222=ORIENTED_EDGE('',*,*,#5530,.T.);
#7223=ORIENTED_EDGE('',*,*,#5526,.F.);
#7224=ORIENTED_EDGE('',*,*,#5531,.F.);
#7225=ORIENTED_EDGE('',*,*,#5532,.T.);
#7226=ORIENTED_EDGE('',*,*,#5533,.T.);
#7227=ORIENTED_EDGE('',*,*,#5529,.F.);
#7228=ORIENTED_EDGE('',*,*,#5534,.F.);
#7229=ORIENTED_EDGE('',*,*,#5535,.T.);
#7230=ORIENTED_EDGE('',*,*,#5536,.T.);
#7231=ORIENTED_EDGE('',*,*,#5532,.F.);
#7232=ORIENTED_EDGE('',*,*,#5537,.F.);
#7233=ORIENTED_EDGE('',*,*,#5538,.T.);
#7234=ORIENTED_EDGE('',*,*,#5539,.T.);
#7235=ORIENTED_EDGE('',*,*,#5535,.F.);
#7236=ORIENTED_EDGE('',*,*,#5540,.F.);
#7237=ORIENTED_EDGE('',*,*,#5541,.T.);
#7238=ORIENTED_EDGE('',*,*,#5542,.T.);
#7239=ORIENTED_EDGE('',*,*,#5538,.F.);
#7240=ORIENTED_EDGE('',*,*,#5543,.F.);
#7241=ORIENTED_EDGE('',*,*,#5544,.T.);
#7242=ORIENTED_EDGE('',*,*,#5545,.T.);
#7243=ORIENTED_EDGE('',*,*,#5541,.F.);
#7244=ORIENTED_EDGE('',*,*,#5546,.F.);
#7245=ORIENTED_EDGE('',*,*,#5547,.T.);
#7246=ORIENTED_EDGE('',*,*,#5548,.T.);
#7247=ORIENTED_EDGE('',*,*,#5544,.F.);
#7248=ORIENTED_EDGE('',*,*,#5549,.F.);
#7249=ORIENTED_EDGE('',*,*,#5550,.T.);
#7250=ORIENTED_EDGE('',*,*,#5551,.T.);
#7251=ORIENTED_EDGE('',*,*,#5547,.F.);
#7252=ORIENTED_EDGE('',*,*,#5552,.F.);
#7253=ORIENTED_EDGE('',*,*,#5553,.T.);
#7254=ORIENTED_EDGE('',*,*,#5554,.T.);
#7255=ORIENTED_EDGE('',*,*,#5550,.F.);
#7256=ORIENTED_EDGE('',*,*,#5555,.F.);
#7257=ORIENTED_EDGE('',*,*,#5556,.T.);
#7258=ORIENTED_EDGE('',*,*,#5557,.T.);
#7259=ORIENTED_EDGE('',*,*,#5553,.F.);
#7260=ORIENTED_EDGE('',*,*,#5558,.F.);
#7261=ORIENTED_EDGE('',*,*,#5559,.T.);
#7262=ORIENTED_EDGE('',*,*,#5560,.T.);
#7263=ORIENTED_EDGE('',*,*,#5556,.F.);
#7264=ORIENTED_EDGE('',*,*,#5561,.F.);
#7265=ORIENTED_EDGE('',*,*,#5562,.F.);
#7266=ORIENTED_EDGE('',*,*,#5563,.F.);
#7267=ORIENTED_EDGE('',*,*,#5564,.F.);
#7268=ORIENTED_EDGE('',*,*,#5565,.T.);
#7269=ORIENTED_EDGE('',*,*,#5566,.T.);
#7270=ORIENTED_EDGE('',*,*,#5567,.T.);
#7271=ORIENTED_EDGE('',*,*,#5568,.T.);
#7272=ORIENTED_EDGE('',*,*,#5569,.T.);
#7273=ORIENTED_EDGE('',*,*,#5570,.T.);
#7274=ORIENTED_EDGE('',*,*,#5569,.F.);
#7275=ORIENTED_EDGE('',*,*,#5571,.T.);
#7276=ORIENTED_EDGE('',*,*,#5572,.T.);
#7277=ORIENTED_EDGE('',*,*,#5573,.T.);
#7278=ORIENTED_EDGE('',*,*,#5574,.T.);
#7279=ORIENTED_EDGE('',*,*,#5566,.F.);
#7280=ORIENTED_EDGE('',*,*,#5575,.T.);
#7281=ORIENTED_EDGE('',*,*,#5576,.T.);
#7282=ORIENTED_EDGE('',*,*,#5577,.T.);
#7283=ORIENTED_EDGE('',*,*,#5573,.F.);
#7284=ORIENTED_EDGE('',*,*,#5578,.T.);
#7285=ORIENTED_EDGE('',*,*,#5579,.T.);
#7286=ORIENTED_EDGE('',*,*,#5580,.T.);
#7287=ORIENTED_EDGE('',*,*,#5576,.F.);
#7288=ORIENTED_EDGE('',*,*,#5581,.T.);
#7289=ORIENTED_EDGE('',*,*,#5582,.T.);
#7290=ORIENTED_EDGE('',*,*,#5583,.T.);
#7291=ORIENTED_EDGE('',*,*,#5579,.F.);
#7292=ORIENTED_EDGE('',*,*,#5584,.T.);
#7293=ORIENTED_EDGE('',*,*,#5585,.T.);
#7294=ORIENTED_EDGE('',*,*,#5586,.T.);
#7295=ORIENTED_EDGE('',*,*,#5582,.F.);
#7296=ORIENTED_EDGE('',*,*,#5587,.T.);
#7297=ORIENTED_EDGE('',*,*,#5588,.T.);
#7298=ORIENTED_EDGE('',*,*,#5589,.T.);
#7299=ORIENTED_EDGE('',*,*,#5585,.F.);
#7300=ORIENTED_EDGE('',*,*,#5590,.T.);
#7301=ORIENTED_EDGE('',*,*,#5591,.T.);
#7302=ORIENTED_EDGE('',*,*,#5592,.T.);
#7303=ORIENTED_EDGE('',*,*,#5588,.F.);
#7304=ORIENTED_EDGE('',*,*,#5593,.T.);
#7305=ORIENTED_EDGE('',*,*,#5594,.T.);
#7306=ORIENTED_EDGE('',*,*,#5595,.T.);
#7307=ORIENTED_EDGE('',*,*,#5591,.F.);
#7308=ORIENTED_EDGE('',*,*,#5596,.T.);
#7309=ORIENTED_EDGE('',*,*,#5597,.T.);
#7310=ORIENTED_EDGE('',*,*,#5598,.T.);
#7311=ORIENTED_EDGE('',*,*,#5594,.F.);
#7312=ORIENTED_EDGE('',*,*,#5599,.T.);
#7313=ORIENTED_EDGE('',*,*,#5600,.T.);
#7314=ORIENTED_EDGE('',*,*,#5601,.T.);
#7315=ORIENTED_EDGE('',*,*,#5597,.F.);
#7316=ORIENTED_EDGE('',*,*,#5602,.T.);
#7317=ORIENTED_EDGE('',*,*,#5603,.T.);
#7318=ORIENTED_EDGE('',*,*,#5604,.T.);
#7319=ORIENTED_EDGE('',*,*,#5600,.F.);
#7320=ORIENTED_EDGE('',*,*,#5605,.T.);
#7321=ORIENTED_EDGE('',*,*,#5606,.T.);
#7322=ORIENTED_EDGE('',*,*,#5607,.T.);
#7323=ORIENTED_EDGE('',*,*,#5603,.F.);
#7324=ORIENTED_EDGE('',*,*,#5608,.T.);
#7325=ORIENTED_EDGE('',*,*,#5609,.T.);
#7326=ORIENTED_EDGE('',*,*,#5610,.T.);
#7327=ORIENTED_EDGE('',*,*,#5606,.F.);
#7328=ORIENTED_EDGE('',*,*,#5611,.T.);
#7329=ORIENTED_EDGE('',*,*,#5612,.F.);
#7330=ORIENTED_EDGE('',*,*,#5613,.T.);
#7331=ORIENTED_EDGE('',*,*,#5614,.F.);
#7332=ORIENTED_EDGE('',*,*,#5615,.T.);
#7333=ORIENTED_EDGE('',*,*,#5616,.T.);
#7334=ORIENTED_EDGE('',*,*,#5617,.T.);
#7335=ORIENTED_EDGE('',*,*,#5618,.F.);
#7336=ORIENTED_EDGE('',*,*,#5619,.F.);
#7337=ORIENTED_EDGE('',*,*,#5620,.T.);
#7338=ORIENTED_EDGE('',*,*,#5621,.T.);
#7339=ORIENTED_EDGE('',*,*,#5616,.F.);
#7340=ORIENTED_EDGE('',*,*,#5622,.F.);
#7341=ORIENTED_EDGE('',*,*,#5623,.T.);
#7342=ORIENTED_EDGE('',*,*,#5624,.T.);
#7343=ORIENTED_EDGE('',*,*,#5620,.F.);
#7344=ORIENTED_EDGE('',*,*,#5625,.F.);
#7345=ORIENTED_EDGE('',*,*,#5626,.T.);
#7346=ORIENTED_EDGE('',*,*,#5627,.T.);
#7347=ORIENTED_EDGE('',*,*,#5623,.F.);
#7348=ORIENTED_EDGE('',*,*,#5628,.F.);
#7349=ORIENTED_EDGE('',*,*,#5629,.T.);
#7350=ORIENTED_EDGE('',*,*,#5630,.T.);
#7351=ORIENTED_EDGE('',*,*,#5626,.F.);
#7352=ORIENTED_EDGE('',*,*,#5631,.F.);
#7353=ORIENTED_EDGE('',*,*,#5632,.T.);
#7354=ORIENTED_EDGE('',*,*,#5633,.T.);
#7355=ORIENTED_EDGE('',*,*,#5629,.F.);
#7356=ORIENTED_EDGE('',*,*,#5634,.F.);
#7357=ORIENTED_EDGE('',*,*,#5635,.T.);
#7358=ORIENTED_EDGE('',*,*,#5636,.T.);
#7359=ORIENTED_EDGE('',*,*,#5632,.F.);
#7360=ORIENTED_EDGE('',*,*,#5637,.F.);
#7361=ORIENTED_EDGE('',*,*,#5638,.T.);
#7362=ORIENTED_EDGE('',*,*,#5639,.T.);
#7363=ORIENTED_EDGE('',*,*,#5635,.F.);
#7364=ORIENTED_EDGE('',*,*,#5640,.F.);
#7365=ORIENTED_EDGE('',*,*,#5641,.T.);
#7366=ORIENTED_EDGE('',*,*,#5642,.T.);
#7367=ORIENTED_EDGE('',*,*,#5638,.F.);
#7368=ORIENTED_EDGE('',*,*,#5643,.F.);
#7369=ORIENTED_EDGE('',*,*,#5644,.T.);
#7370=ORIENTED_EDGE('',*,*,#5645,.T.);
#7371=ORIENTED_EDGE('',*,*,#5641,.F.);
#7372=ORIENTED_EDGE('',*,*,#5646,.F.);
#7373=ORIENTED_EDGE('',*,*,#5647,.T.);
#7374=ORIENTED_EDGE('',*,*,#5648,.T.);
#7375=ORIENTED_EDGE('',*,*,#5644,.F.);
#7376=ORIENTED_EDGE('',*,*,#5649,.F.);
#7377=ORIENTED_EDGE('',*,*,#5650,.T.);
#7378=ORIENTED_EDGE('',*,*,#5651,.T.);
#7379=ORIENTED_EDGE('',*,*,#5647,.F.);
#7380=ORIENTED_EDGE('',*,*,#5652,.F.);
#7381=ORIENTED_EDGE('',*,*,#5653,.T.);
#7382=ORIENTED_EDGE('',*,*,#5654,.T.);
#7383=ORIENTED_EDGE('',*,*,#5650,.F.);
#7384=ORIENTED_EDGE('',*,*,#5655,.F.);
#7385=ORIENTED_EDGE('',*,*,#5656,.T.);
#7386=ORIENTED_EDGE('',*,*,#5657,.T.);
#7387=ORIENTED_EDGE('',*,*,#5653,.F.);
#7388=ORIENTED_EDGE('',*,*,#5658,.F.);
#7389=ORIENTED_EDGE('',*,*,#5659,.F.);
#7390=ORIENTED_EDGE('',*,*,#5660,.F.);
#7391=ORIENTED_EDGE('',*,*,#5661,.F.);
#7392=ORIENTED_EDGE('',*,*,#5662,.T.);
#7393=ORIENTED_EDGE('',*,*,#5663,.T.);
#7394=ORIENTED_EDGE('',*,*,#5664,.T.);
#7395=ORIENTED_EDGE('',*,*,#5665,.T.);
#7396=ORIENTED_EDGE('',*,*,#5666,.T.);
#7397=ORIENTED_EDGE('',*,*,#5667,.T.);
#7398=ORIENTED_EDGE('',*,*,#5668,.T.);
#7399=ORIENTED_EDGE('',*,*,#5663,.F.);
#7400=ORIENTED_EDGE('',*,*,#5669,.T.);
#7401=ORIENTED_EDGE('',*,*,#5670,.T.);
#7402=ORIENTED_EDGE('',*,*,#5671,.T.);
#7403=ORIENTED_EDGE('',*,*,#5667,.F.);
#7404=ORIENTED_EDGE('',*,*,#5672,.T.);
#7405=ORIENTED_EDGE('',*,*,#5673,.T.);
#7406=ORIENTED_EDGE('',*,*,#5674,.T.);
#7407=ORIENTED_EDGE('',*,*,#5670,.F.);
#7408=ORIENTED_EDGE('',*,*,#5675,.T.);
#7409=ORIENTED_EDGE('',*,*,#5676,.T.);
#7410=ORIENTED_EDGE('',*,*,#5677,.T.);
#7411=ORIENTED_EDGE('',*,*,#5673,.F.);
#7412=ORIENTED_EDGE('',*,*,#5678,.T.);
#7413=ORIENTED_EDGE('',*,*,#5679,.T.);
#7414=ORIENTED_EDGE('',*,*,#5680,.T.);
#7415=ORIENTED_EDGE('',*,*,#5676,.F.);
#7416=ORIENTED_EDGE('',*,*,#5681,.T.);
#7417=ORIENTED_EDGE('',*,*,#5682,.T.);
#7418=ORIENTED_EDGE('',*,*,#5683,.T.);
#7419=ORIENTED_EDGE('',*,*,#5679,.F.);
#7420=ORIENTED_EDGE('',*,*,#5684,.T.);
#7421=ORIENTED_EDGE('',*,*,#5685,.F.);
#7422=ORIENTED_EDGE('',*,*,#5686,.T.);
#7423=ORIENTED_EDGE('',*,*,#5687,.F.);
#7424=ORIENTED_EDGE('',*,*,#5688,.T.);
#7425=ORIENTED_EDGE('',*,*,#5689,.T.);
#7426=ORIENTED_EDGE('',*,*,#5690,.T.);
#7427=ORIENTED_EDGE('',*,*,#5691,.F.);
#7428=ORIENTED_EDGE('',*,*,#5692,.F.);
#7429=ORIENTED_EDGE('',*,*,#5693,.T.);
#7430=ORIENTED_EDGE('',*,*,#5694,.T.);
#7431=ORIENTED_EDGE('',*,*,#5689,.F.);
#7432=ORIENTED_EDGE('',*,*,#5695,.F.);
#7433=ORIENTED_EDGE('',*,*,#5696,.T.);
#7434=ORIENTED_EDGE('',*,*,#5697,.T.);
#7435=ORIENTED_EDGE('',*,*,#5693,.F.);
#7436=ORIENTED_EDGE('',*,*,#5698,.F.);
#7437=ORIENTED_EDGE('',*,*,#5699,.T.);
#7438=ORIENTED_EDGE('',*,*,#5700,.T.);
#7439=ORIENTED_EDGE('',*,*,#5696,.F.);
#7440=ORIENTED_EDGE('',*,*,#5701,.F.);
#7441=ORIENTED_EDGE('',*,*,#5702,.T.);
#7442=ORIENTED_EDGE('',*,*,#5703,.T.);
#7443=ORIENTED_EDGE('',*,*,#5699,.F.);
#7444=ORIENTED_EDGE('',*,*,#5704,.F.);
#7445=ORIENTED_EDGE('',*,*,#5705,.T.);
#7446=ORIENTED_EDGE('',*,*,#5706,.T.);
#7447=ORIENTED_EDGE('',*,*,#5702,.F.);
#7448=ORIENTED_EDGE('',*,*,#5707,.F.);
#7449=ORIENTED_EDGE('',*,*,#5708,.T.);
#7450=ORIENTED_EDGE('',*,*,#5709,.T.);
#7451=ORIENTED_EDGE('',*,*,#5705,.F.);
#7452=ORIENTED_EDGE('',*,*,#5710,.F.);
#7453=ORIENTED_EDGE('',*,*,#5711,.F.);
#7454=ORIENTED_EDGE('',*,*,#5712,.F.);
#7455=ORIENTED_EDGE('',*,*,#5713,.F.);
#7456=ORIENTED_EDGE('',*,*,#5714,.T.);
#7457=ORIENTED_EDGE('',*,*,#5711,.T.);
#7458=ORIENTED_EDGE('',*,*,#5715,.T.);
#7459=ORIENTED_EDGE('',*,*,#5708,.F.);
#7460=ORIENTED_EDGE('',*,*,#5716,.F.);
#7461=ORIENTED_EDGE('',*,*,#5717,.F.);
#7462=ORIENTED_EDGE('',*,*,#5690,.F.);
#7463=ORIENTED_EDGE('',*,*,#5694,.F.);
#7464=ORIENTED_EDGE('',*,*,#5697,.F.);
#7465=ORIENTED_EDGE('',*,*,#5700,.F.);
#7466=ORIENTED_EDGE('',*,*,#5703,.F.);
#7467=ORIENTED_EDGE('',*,*,#5706,.F.);
#7468=ORIENTED_EDGE('',*,*,#5709,.F.);
#7469=ORIENTED_EDGE('',*,*,#5715,.F.);
#7470=ORIENTED_EDGE('',*,*,#5714,.F.);
#7471=ORIENTED_EDGE('',*,*,#5718,.F.);
#7472=ORIENTED_EDGE('',*,*,#5664,.F.);
#7473=ORIENTED_EDGE('',*,*,#5668,.F.);
#7474=ORIENTED_EDGE('',*,*,#5671,.F.);
#7475=ORIENTED_EDGE('',*,*,#5674,.F.);
#7476=ORIENTED_EDGE('',*,*,#5677,.F.);
#7477=ORIENTED_EDGE('',*,*,#5680,.F.);
#7478=ORIENTED_EDGE('',*,*,#5683,.F.);
#7479=ORIENTED_EDGE('',*,*,#5719,.F.);
#7480=ORIENTED_EDGE('',*,*,#5688,.F.);
#7481=ORIENTED_EDGE('',*,*,#5720,.F.);
#7482=ORIENTED_EDGE('',*,*,#5686,.F.);
#7483=ORIENTED_EDGE('',*,*,#5721,.F.);
#7484=ORIENTED_EDGE('',*,*,#5684,.F.);
#7485=ORIENTED_EDGE('',*,*,#5681,.F.);
#7486=ORIENTED_EDGE('',*,*,#5678,.F.);
#7487=ORIENTED_EDGE('',*,*,#5675,.F.);
#7488=ORIENTED_EDGE('',*,*,#5672,.F.);
#7489=ORIENTED_EDGE('',*,*,#5669,.F.);
#7490=ORIENTED_EDGE('',*,*,#5666,.F.);
#7491=ORIENTED_EDGE('',*,*,#5722,.F.);
#7492=ORIENTED_EDGE('',*,*,#5712,.T.);
#7493=ORIENTED_EDGE('',*,*,#5716,.T.);
#7494=ORIENTED_EDGE('',*,*,#5710,.T.);
#7495=ORIENTED_EDGE('',*,*,#5707,.T.);
#7496=ORIENTED_EDGE('',*,*,#5704,.T.);
#7497=ORIENTED_EDGE('',*,*,#5701,.T.);
#7498=ORIENTED_EDGE('',*,*,#5698,.T.);
#7499=ORIENTED_EDGE('',*,*,#5695,.T.);
#7500=ORIENTED_EDGE('',*,*,#5692,.T.);
#7501=ORIENTED_EDGE('',*,*,#5723,.F.);
#7502=ORIENTED_EDGE('',*,*,#5718,.T.);
#7503=ORIENTED_EDGE('',*,*,#5713,.T.);
#7504=ORIENTED_EDGE('',*,*,#5722,.T.);
#7505=ORIENTED_EDGE('',*,*,#5665,.F.);
#7506=ORIENTED_EDGE('',*,*,#5685,.T.);
#7507=ORIENTED_EDGE('',*,*,#5719,.T.);
#7508=ORIENTED_EDGE('',*,*,#5682,.F.);
#7509=ORIENTED_EDGE('',*,*,#5721,.T.);
#7510=ORIENTED_EDGE('',*,*,#5724,.F.);
#7511=ORIENTED_EDGE('',*,*,#5725,.T.);
#7512=ORIENTED_EDGE('',*,*,#5723,.T.);
#7513=ORIENTED_EDGE('',*,*,#5725,.F.);
#7514=ORIENTED_EDGE('',*,*,#5726,.F.);
#7515=ORIENTED_EDGE('',*,*,#5727,.F.);
#7516=ORIENTED_EDGE('',*,*,#5728,.F.);
#7517=ORIENTED_EDGE('',*,*,#5729,.F.);
#7518=ORIENTED_EDGE('',*,*,#5730,.T.);
#7519=ORIENTED_EDGE('',*,*,#5373,.T.);
#7520=ORIENTED_EDGE('',*,*,#5731,.T.);
#7521=ORIENTED_EDGE('',*,*,#5420,.T.);
#7522=ORIENTED_EDGE('',*,*,#5732,.T.);
#7523=ORIENTED_EDGE('',*,*,#5324,.T.);
#7524=ORIENTED_EDGE('',*,*,#5733,.T.);
#7525=ORIENTED_EDGE('',*,*,#5467,.T.);
#7526=ORIENTED_EDGE('',*,*,#5734,.T.);
#7527=ORIENTED_EDGE('',*,*,#5517,.T.);
#7528=ORIENTED_EDGE('',*,*,#5735,.T.);
#7529=ORIENTED_EDGE('',*,*,#5564,.T.);
#7530=ORIENTED_EDGE('',*,*,#5736,.T.);
#7531=ORIENTED_EDGE('',*,*,#5614,.T.);
#7532=ORIENTED_EDGE('',*,*,#5737,.T.);
#7533=ORIENTED_EDGE('',*,*,#5661,.T.);
#7534=ORIENTED_EDGE('',*,*,#5724,.T.);
#7535=ORIENTED_EDGE('',*,*,#5568,.F.);
#7536=ORIENTED_EDGE('',*,*,#5738,.T.);
#7537=ORIENTED_EDGE('',*,*,#5618,.T.);
#7538=ORIENTED_EDGE('',*,*,#5739,.T.);
#7539=ORIENTED_EDGE('',*,*,#5571,.F.);
#7540=ORIENTED_EDGE('',*,*,#5659,.T.);
#7541=ORIENTED_EDGE('',*,*,#5740,.T.);
#7542=ORIENTED_EDGE('',*,*,#5656,.F.);
#7543=ORIENTED_EDGE('',*,*,#5741,.F.);
#7544=ORIENTED_EDGE('',*,*,#5739,.F.);
#7545=ORIENTED_EDGE('',*,*,#5617,.F.);
#7546=ORIENTED_EDGE('',*,*,#5621,.F.);
#7547=ORIENTED_EDGE('',*,*,#5624,.F.);
#7548=ORIENTED_EDGE('',*,*,#5627,.F.);
#7549=ORIENTED_EDGE('',*,*,#5630,.F.);
#7550=ORIENTED_EDGE('',*,*,#5633,.F.);
#7551=ORIENTED_EDGE('',*,*,#5636,.F.);
#7552=ORIENTED_EDGE('',*,*,#5639,.F.);
#7553=ORIENTED_EDGE('',*,*,#5642,.F.);
#7554=ORIENTED_EDGE('',*,*,#5645,.F.);
#7555=ORIENTED_EDGE('',*,*,#5648,.F.);
#7556=ORIENTED_EDGE('',*,*,#5651,.F.);
#7557=ORIENTED_EDGE('',*,*,#5654,.F.);
#7558=ORIENTED_EDGE('',*,*,#5657,.F.);
#7559=ORIENTED_EDGE('',*,*,#5740,.F.);
#7560=ORIENTED_EDGE('',*,*,#5662,.F.);
#7561=ORIENTED_EDGE('',*,*,#5737,.F.);
#7562=ORIENTED_EDGE('',*,*,#5613,.F.);
#7563=ORIENTED_EDGE('',*,*,#5742,.F.);
#7564=ORIENTED_EDGE('',*,*,#5611,.F.);
#7565=ORIENTED_EDGE('',*,*,#5608,.F.);
#7566=ORIENTED_EDGE('',*,*,#5605,.F.);
#7567=ORIENTED_EDGE('',*,*,#5602,.F.);
#7568=ORIENTED_EDGE('',*,*,#5599,.F.);
#7569=ORIENTED_EDGE('',*,*,#5596,.F.);
#7570=ORIENTED_EDGE('',*,*,#5593,.F.);
#7571=ORIENTED_EDGE('',*,*,#5590,.F.);
#7572=ORIENTED_EDGE('',*,*,#5587,.F.);
#7573=ORIENTED_EDGE('',*,*,#5584,.F.);
#7574=ORIENTED_EDGE('',*,*,#5581,.F.);
#7575=ORIENTED_EDGE('',*,*,#5578,.F.);
#7576=ORIENTED_EDGE('',*,*,#5575,.F.);
#7577=ORIENTED_EDGE('',*,*,#5572,.F.);
#7578=ORIENTED_EDGE('',*,*,#5738,.F.);
#7579=ORIENTED_EDGE('',*,*,#5567,.F.);
#7580=ORIENTED_EDGE('',*,*,#5574,.F.);
#7581=ORIENTED_EDGE('',*,*,#5577,.F.);
#7582=ORIENTED_EDGE('',*,*,#5580,.F.);
#7583=ORIENTED_EDGE('',*,*,#5583,.F.);
#7584=ORIENTED_EDGE('',*,*,#5586,.F.);
#7585=ORIENTED_EDGE('',*,*,#5589,.F.);
#7586=ORIENTED_EDGE('',*,*,#5592,.F.);
#7587=ORIENTED_EDGE('',*,*,#5595,.F.);
#7588=ORIENTED_EDGE('',*,*,#5598,.F.);
#7589=ORIENTED_EDGE('',*,*,#5601,.F.);
#7590=ORIENTED_EDGE('',*,*,#5604,.F.);
#7591=ORIENTED_EDGE('',*,*,#5607,.F.);
#7592=ORIENTED_EDGE('',*,*,#5610,.F.);
#7593=ORIENTED_EDGE('',*,*,#5743,.F.);
#7594=ORIENTED_EDGE('',*,*,#5615,.F.);
#7595=ORIENTED_EDGE('',*,*,#5736,.F.);
#7596=ORIENTED_EDGE('',*,*,#5660,.T.);
#7597=ORIENTED_EDGE('',*,*,#5741,.T.);
#7598=ORIENTED_EDGE('',*,*,#5658,.T.);
#7599=ORIENTED_EDGE('',*,*,#5655,.T.);
#7600=ORIENTED_EDGE('',*,*,#5652,.T.);
#7601=ORIENTED_EDGE('',*,*,#5649,.T.);
#7602=ORIENTED_EDGE('',*,*,#5646,.T.);
#7603=ORIENTED_EDGE('',*,*,#5643,.T.);
#7604=ORIENTED_EDGE('',*,*,#5640,.T.);
#7605=ORIENTED_EDGE('',*,*,#5637,.T.);
#7606=ORIENTED_EDGE('',*,*,#5634,.T.);
#7607=ORIENTED_EDGE('',*,*,#5631,.T.);
#7608=ORIENTED_EDGE('',*,*,#5628,.T.);
#7609=ORIENTED_EDGE('',*,*,#5625,.T.);
#7610=ORIENTED_EDGE('',*,*,#5622,.T.);
#7611=ORIENTED_EDGE('',*,*,#5619,.T.);
#7612=ORIENTED_EDGE('',*,*,#5612,.T.);
#7613=ORIENTED_EDGE('',*,*,#5743,.T.);
#7614=ORIENTED_EDGE('',*,*,#5609,.F.);
#7615=ORIENTED_EDGE('',*,*,#5742,.T.);
#7616=ORIENTED_EDGE('',*,*,#5471,.F.);
#7617=ORIENTED_EDGE('',*,*,#5744,.T.);
#7618=ORIENTED_EDGE('',*,*,#5521,.T.);
#7619=ORIENTED_EDGE('',*,*,#5745,.T.);
#7620=ORIENTED_EDGE('',*,*,#5474,.F.);
#7621=ORIENTED_EDGE('',*,*,#5562,.T.);
#7622=ORIENTED_EDGE('',*,*,#5746,.T.);
#7623=ORIENTED_EDGE('',*,*,#5559,.F.);
#7624=ORIENTED_EDGE('',*,*,#5747,.F.);
#7625=ORIENTED_EDGE('',*,*,#5745,.F.);
#7626=ORIENTED_EDGE('',*,*,#5520,.F.);
#7627=ORIENTED_EDGE('',*,*,#5524,.F.);
#7628=ORIENTED_EDGE('',*,*,#5527,.F.);
#7629=ORIENTED_EDGE('',*,*,#5530,.F.);
#7630=ORIENTED_EDGE('',*,*,#5533,.F.);
#7631=ORIENTED_EDGE('',*,*,#5536,.F.);
#7632=ORIENTED_EDGE('',*,*,#5539,.F.);
#7633=ORIENTED_EDGE('',*,*,#5542,.F.);
#7634=ORIENTED_EDGE('',*,*,#5545,.F.);
#7635=ORIENTED_EDGE('',*,*,#5548,.F.);
#7636=ORIENTED_EDGE('',*,*,#5551,.F.);
#7637=ORIENTED_EDGE('',*,*,#5554,.F.);
#7638=ORIENTED_EDGE('',*,*,#5557,.F.);
#7639=ORIENTED_EDGE('',*,*,#5560,.F.);
#7640=ORIENTED_EDGE('',*,*,#5746,.F.);
#7641=ORIENTED_EDGE('',*,*,#5565,.F.);
#7642=ORIENTED_EDGE('',*,*,#5735,.F.);
#7643=ORIENTED_EDGE('',*,*,#5516,.F.);
#7644=ORIENTED_EDGE('',*,*,#5748,.F.);
#7645=ORIENTED_EDGE('',*,*,#5514,.F.);
#7646=ORIENTED_EDGE('',*,*,#5511,.F.);
#7647=ORIENTED_EDGE('',*,*,#5508,.F.);
#7648=ORIENTED_EDGE('',*,*,#5505,.F.);
#7649=ORIENTED_EDGE('',*,*,#5502,.F.);
#7650=ORIENTED_EDGE('',*,*,#5499,.F.);
#7651=ORIENTED_EDGE('',*,*,#5496,.F.);
#7652=ORIENTED_EDGE('',*,*,#5493,.F.);
#7653=ORIENTED_EDGE('',*,*,#5490,.F.);
#7654=ORIENTED_EDGE('',*,*,#5487,.F.);
#7655=ORIENTED_EDGE('',*,*,#5484,.F.);
#7656=ORIENTED_EDGE('',*,*,#5481,.F.);
#7657=ORIENTED_EDGE('',*,*,#5478,.F.);
#7658=ORIENTED_EDGE('',*,*,#5475,.F.);
#7659=ORIENTED_EDGE('',*,*,#5744,.F.);
#7660=ORIENTED_EDGE('',*,*,#5470,.F.);
#7661=ORIENTED_EDGE('',*,*,#5477,.F.);
#7662=ORIENTED_EDGE('',*,*,#5480,.F.);
#7663=ORIENTED_EDGE('',*,*,#5483,.F.);
#7664=ORIENTED_EDGE('',*,*,#5486,.F.);
#7665=ORIENTED_EDGE('',*,*,#5489,.F.);
#7666=ORIENTED_EDGE('',*,*,#5492,.F.);
#7667=ORIENTED_EDGE('',*,*,#5495,.F.);
#7668=ORIENTED_EDGE('',*,*,#5498,.F.);
#7669=ORIENTED_EDGE('',*,*,#5501,.F.);
#7670=ORIENTED_EDGE('',*,*,#5504,.F.);
#7671=ORIENTED_EDGE('',*,*,#5507,.F.);
#7672=ORIENTED_EDGE('',*,*,#5510,.F.);
#7673=ORIENTED_EDGE('',*,*,#5513,.F.);
#7674=ORIENTED_EDGE('',*,*,#5749,.F.);
#7675=ORIENTED_EDGE('',*,*,#5518,.F.);
#7676=ORIENTED_EDGE('',*,*,#5734,.F.);
#7677=ORIENTED_EDGE('',*,*,#5563,.T.);
#7678=ORIENTED_EDGE('',*,*,#5747,.T.);
#7679=ORIENTED_EDGE('',*,*,#5561,.T.);
#7680=ORIENTED_EDGE('',*,*,#5558,.T.);
#7681=ORIENTED_EDGE('',*,*,#5555,.T.);
#7682=ORIENTED_EDGE('',*,*,#5552,.T.);
#7683=ORIENTED_EDGE('',*,*,#5549,.T.);
#7684=ORIENTED_EDGE('',*,*,#5546,.T.);
#7685=ORIENTED_EDGE('',*,*,#5543,.T.);
#7686=ORIENTED_EDGE('',*,*,#5540,.T.);
#7687=ORIENTED_EDGE('',*,*,#5537,.T.);
#7688=ORIENTED_EDGE('',*,*,#5534,.T.);
#7689=ORIENTED_EDGE('',*,*,#5531,.T.);
#7690=ORIENTED_EDGE('',*,*,#5528,.T.);
#7691=ORIENTED_EDGE('',*,*,#5525,.T.);
#7692=ORIENTED_EDGE('',*,*,#5522,.T.);
#7693=ORIENTED_EDGE('',*,*,#5515,.T.);
#7694=ORIENTED_EDGE('',*,*,#5749,.T.);
#7695=ORIENTED_EDGE('',*,*,#5512,.F.);
#7696=ORIENTED_EDGE('',*,*,#5748,.T.);
#7697=ORIENTED_EDGE('',*,*,#5750,.F.);
#7698=ORIENTED_EDGE('',*,*,#5751,.T.);
#7699=ORIENTED_EDGE('',*,*,#5281,.F.);
#7700=ORIENTED_EDGE('',*,*,#5752,.T.);
#7701=ORIENTED_EDGE('',*,*,#5753,.T.);
#7702=ORIENTED_EDGE('',*,*,#5424,.T.);
#7703=ORIENTED_EDGE('',*,*,#5754,.T.);
#7704=ORIENTED_EDGE('',*,*,#5755,.T.);
#7705=ORIENTED_EDGE('',*,*,#5756,.F.);
#7706=ORIENTED_EDGE('',*,*,#5757,.F.);
#7707=ORIENTED_EDGE('',*,*,#5279,.F.);
#7708=ORIENTED_EDGE('',*,*,#5758,.T.);
#7709=ORIENTED_EDGE('',*,*,#5465,.T.);
#7710=ORIENTED_EDGE('',*,*,#5759,.T.);
#7711=ORIENTED_EDGE('',*,*,#5462,.F.);
#7712=ORIENTED_EDGE('',*,*,#5760,.F.);
#7713=ORIENTED_EDGE('',*,*,#5754,.F.);
#7714=ORIENTED_EDGE('',*,*,#5423,.F.);
#7715=ORIENTED_EDGE('',*,*,#5427,.F.);
#7716=ORIENTED_EDGE('',*,*,#5430,.F.);
#7717=ORIENTED_EDGE('',*,*,#5433,.F.);
#7718=ORIENTED_EDGE('',*,*,#5436,.F.);
#7719=ORIENTED_EDGE('',*,*,#5439,.F.);
#7720=ORIENTED_EDGE('',*,*,#5442,.F.);
#7721=ORIENTED_EDGE('',*,*,#5445,.F.);
#7722=ORIENTED_EDGE('',*,*,#5448,.F.);
#7723=ORIENTED_EDGE('',*,*,#5451,.F.);
#7724=ORIENTED_EDGE('',*,*,#5454,.F.);
#7725=ORIENTED_EDGE('',*,*,#5457,.F.);
#7726=ORIENTED_EDGE('',*,*,#5460,.F.);
#7727=ORIENTED_EDGE('',*,*,#5463,.F.);
#7728=ORIENTED_EDGE('',*,*,#5759,.F.);
#7729=ORIENTED_EDGE('',*,*,#5468,.F.);
#7730=ORIENTED_EDGE('',*,*,#5733,.F.);
#7731=ORIENTED_EDGE('',*,*,#5323,.F.);
#7732=ORIENTED_EDGE('',*,*,#5761,.F.);
#7733=ORIENTED_EDGE('',*,*,#5321,.F.);
#7734=ORIENTED_EDGE('',*,*,#5318,.F.);
#7735=ORIENTED_EDGE('',*,*,#5315,.F.);
#7736=ORIENTED_EDGE('',*,*,#5312,.F.);
#7737=ORIENTED_EDGE('',*,*,#5309,.F.);
#7738=ORIENTED_EDGE('',*,*,#5306,.F.);
#7739=ORIENTED_EDGE('',*,*,#5303,.F.);
#7740=ORIENTED_EDGE('',*,*,#5300,.F.);
#7741=ORIENTED_EDGE('',*,*,#5297,.F.);
#7742=ORIENTED_EDGE('',*,*,#5294,.F.);
#7743=ORIENTED_EDGE('',*,*,#5291,.F.);
#7744=ORIENTED_EDGE('',*,*,#5288,.F.);
#7745=ORIENTED_EDGE('',*,*,#5285,.F.);
#7746=ORIENTED_EDGE('',*,*,#5282,.F.);
#7747=ORIENTED_EDGE('',*,*,#5751,.F.);
#7748=ORIENTED_EDGE('',*,*,#5758,.F.);
#7749=ORIENTED_EDGE('',*,*,#5278,.F.);
#7750=ORIENTED_EDGE('',*,*,#5284,.F.);
#7751=ORIENTED_EDGE('',*,*,#5287,.F.);
#7752=ORIENTED_EDGE('',*,*,#5290,.F.);
#7753=ORIENTED_EDGE('',*,*,#5293,.F.);
#7754=ORIENTED_EDGE('',*,*,#5296,.F.);
#7755=ORIENTED_EDGE('',*,*,#5299,.F.);
#7756=ORIENTED_EDGE('',*,*,#5302,.F.);
#7757=ORIENTED_EDGE('',*,*,#5305,.F.);
#7758=ORIENTED_EDGE('',*,*,#5308,.F.);
#7759=ORIENTED_EDGE('',*,*,#5311,.F.);
#7760=ORIENTED_EDGE('',*,*,#5314,.F.);
#7761=ORIENTED_EDGE('',*,*,#5317,.F.);
#7762=ORIENTED_EDGE('',*,*,#5320,.F.);
#7763=ORIENTED_EDGE('',*,*,#5762,.F.);
#7764=ORIENTED_EDGE('',*,*,#5325,.F.);
#7765=ORIENTED_EDGE('',*,*,#5732,.F.);
#7766=ORIENTED_EDGE('',*,*,#5466,.T.);
#7767=ORIENTED_EDGE('',*,*,#5760,.T.);
#7768=ORIENTED_EDGE('',*,*,#5464,.T.);
#7769=ORIENTED_EDGE('',*,*,#5461,.T.);
#7770=ORIENTED_EDGE('',*,*,#5458,.T.);
#7771=ORIENTED_EDGE('',*,*,#5455,.T.);
#7772=ORIENTED_EDGE('',*,*,#5452,.T.);
#7773=ORIENTED_EDGE('',*,*,#5449,.T.);
#7774=ORIENTED_EDGE('',*,*,#5446,.T.);
#7775=ORIENTED_EDGE('',*,*,#5443,.T.);
#7776=ORIENTED_EDGE('',*,*,#5440,.T.);
#7777=ORIENTED_EDGE('',*,*,#5437,.T.);
#7778=ORIENTED_EDGE('',*,*,#5434,.T.);
#7779=ORIENTED_EDGE('',*,*,#5431,.T.);
#7780=ORIENTED_EDGE('',*,*,#5428,.T.);
#7781=ORIENTED_EDGE('',*,*,#5425,.T.);
#7782=ORIENTED_EDGE('',*,*,#5753,.F.);
#7783=ORIENTED_EDGE('',*,*,#5756,.T.);
#7784=ORIENTED_EDGE('',*,*,#5763,.F.);
#7785=ORIENTED_EDGE('',*,*,#5764,.F.);
#7786=ORIENTED_EDGE('',*,*,#5765,.F.);
#7787=ORIENTED_EDGE('',*,*,#5766,.T.);
#7788=ORIENTED_EDGE('',*,*,#5330,.F.);
#7789=ORIENTED_EDGE('',*,*,#5767,.T.);
#7790=ORIENTED_EDGE('',*,*,#5768,.T.);
#7791=ORIENTED_EDGE('',*,*,#5377,.T.);
#7792=ORIENTED_EDGE('',*,*,#5769,.T.);
#7793=ORIENTED_EDGE('',*,*,#5770,.T.);
#7794=ORIENTED_EDGE('',*,*,#5771,.F.);
#7795=ORIENTED_EDGE('',*,*,#5772,.F.);
#7796=ORIENTED_EDGE('',*,*,#5328,.F.);
#7797=ORIENTED_EDGE('',*,*,#5773,.T.);
#7798=ORIENTED_EDGE('',*,*,#5418,.T.);
#7799=ORIENTED_EDGE('',*,*,#5774,.T.);
#7800=ORIENTED_EDGE('',*,*,#5415,.F.);
#7801=ORIENTED_EDGE('',*,*,#5775,.F.);
#7802=ORIENTED_EDGE('',*,*,#5769,.F.);
#7803=ORIENTED_EDGE('',*,*,#5376,.F.);
#7804=ORIENTED_EDGE('',*,*,#5380,.F.);
#7805=ORIENTED_EDGE('',*,*,#5383,.F.);
#7806=ORIENTED_EDGE('',*,*,#5386,.F.);
#7807=ORIENTED_EDGE('',*,*,#5389,.F.);
#7808=ORIENTED_EDGE('',*,*,#5392,.F.);
#7809=ORIENTED_EDGE('',*,*,#5395,.F.);
#7810=ORIENTED_EDGE('',*,*,#5398,.F.);
#7811=ORIENTED_EDGE('',*,*,#5401,.F.);
#7812=ORIENTED_EDGE('',*,*,#5404,.F.);
#7813=ORIENTED_EDGE('',*,*,#5407,.F.);
#7814=ORIENTED_EDGE('',*,*,#5410,.F.);
#7815=ORIENTED_EDGE('',*,*,#5413,.F.);
#7816=ORIENTED_EDGE('',*,*,#5416,.F.);
#7817=ORIENTED_EDGE('',*,*,#5774,.F.);
#7818=ORIENTED_EDGE('',*,*,#5421,.F.);
#7819=ORIENTED_EDGE('',*,*,#5731,.F.);
#7820=ORIENTED_EDGE('',*,*,#5372,.F.);
#7821=ORIENTED_EDGE('',*,*,#5776,.F.);
#7822=ORIENTED_EDGE('',*,*,#5370,.F.);
#7823=ORIENTED_EDGE('',*,*,#5367,.F.);
#7824=ORIENTED_EDGE('',*,*,#5364,.F.);
#7825=ORIENTED_EDGE('',*,*,#5361,.F.);
#7826=ORIENTED_EDGE('',*,*,#5358,.F.);
#7827=ORIENTED_EDGE('',*,*,#5355,.F.);
#7828=ORIENTED_EDGE('',*,*,#5352,.F.);
#7829=ORIENTED_EDGE('',*,*,#5349,.F.);
#7830=ORIENTED_EDGE('',*,*,#5346,.F.);
#7831=ORIENTED_EDGE('',*,*,#5343,.F.);
#7832=ORIENTED_EDGE('',*,*,#5340,.F.);
#7833=ORIENTED_EDGE('',*,*,#5337,.F.);
#7834=ORIENTED_EDGE('',*,*,#5334,.F.);
#7835=ORIENTED_EDGE('',*,*,#5331,.F.);
#7836=ORIENTED_EDGE('',*,*,#5766,.F.);
#7837=ORIENTED_EDGE('',*,*,#5773,.F.);
#7838=ORIENTED_EDGE('',*,*,#5327,.F.);
#7839=ORIENTED_EDGE('',*,*,#5333,.F.);
#7840=ORIENTED_EDGE('',*,*,#5336,.F.);
#7841=ORIENTED_EDGE('',*,*,#5339,.F.);
#7842=ORIENTED_EDGE('',*,*,#5342,.F.);
#7843=ORIENTED_EDGE('',*,*,#5345,.F.);
#7844=ORIENTED_EDGE('',*,*,#5348,.F.);
#7845=ORIENTED_EDGE('',*,*,#5351,.F.);
#7846=ORIENTED_EDGE('',*,*,#5354,.F.);
#7847=ORIENTED_EDGE('',*,*,#5357,.F.);
#7848=ORIENTED_EDGE('',*,*,#5360,.F.);
#7849=ORIENTED_EDGE('',*,*,#5363,.F.);
#7850=ORIENTED_EDGE('',*,*,#5366,.F.);
#7851=ORIENTED_EDGE('',*,*,#5369,.F.);
#7852=ORIENTED_EDGE('',*,*,#5777,.F.);
#7853=ORIENTED_EDGE('',*,*,#5374,.F.);
#7854=ORIENTED_EDGE('',*,*,#5730,.F.);
#7855=ORIENTED_EDGE('',*,*,#5419,.T.);
#7856=ORIENTED_EDGE('',*,*,#5775,.T.);
#7857=ORIENTED_EDGE('',*,*,#5417,.T.);
#7858=ORIENTED_EDGE('',*,*,#5414,.T.);
#7859=ORIENTED_EDGE('',*,*,#5411,.T.);
#7860=ORIENTED_EDGE('',*,*,#5408,.T.);
#7861=ORIENTED_EDGE('',*,*,#5405,.T.);
#7862=ORIENTED_EDGE('',*,*,#5402,.T.);
#7863=ORIENTED_EDGE('',*,*,#5399,.T.);
#7864=ORIENTED_EDGE('',*,*,#5396,.T.);
#7865=ORIENTED_EDGE('',*,*,#5393,.T.);
#7866=ORIENTED_EDGE('',*,*,#5390,.T.);
#7867=ORIENTED_EDGE('',*,*,#5387,.T.);
#7868=ORIENTED_EDGE('',*,*,#5384,.T.);
#7869=ORIENTED_EDGE('',*,*,#5381,.T.);
#7870=ORIENTED_EDGE('',*,*,#5378,.T.);
#7871=ORIENTED_EDGE('',*,*,#5768,.F.);
#7872=ORIENTED_EDGE('',*,*,#5771,.T.);
#7873=ORIENTED_EDGE('',*,*,#5778,.F.);
#7874=ORIENTED_EDGE('',*,*,#5779,.F.);
#7875=ORIENTED_EDGE('',*,*,#5371,.T.);
#7876=ORIENTED_EDGE('',*,*,#5777,.T.);
#7877=ORIENTED_EDGE('',*,*,#5368,.F.);
#7878=ORIENTED_EDGE('',*,*,#5776,.T.);
#7879=ORIENTED_EDGE('',*,*,#5570,.F.);
#7880=ORIENTED_EDGE('',*,*,#5473,.F.);
#7881=ORIENTED_EDGE('',*,*,#5322,.T.);
#7882=ORIENTED_EDGE('',*,*,#5762,.T.);
#7883=ORIENTED_EDGE('',*,*,#5319,.F.);
#7884=ORIENTED_EDGE('',*,*,#5761,.T.);
#7885=ORIENTED_EDGE('',*,*,#5179,.F.);
#7886=ORIENTED_EDGE('',*,*,#5780,.T.);
#7887=ORIENTED_EDGE('',*,*,#5229,.T.);
#7888=ORIENTED_EDGE('',*,*,#5781,.T.);
#7889=ORIENTED_EDGE('',*,*,#5273,.T.);
#7890=ORIENTED_EDGE('',*,*,#5782,.T.);
#7891=ORIENTED_EDGE('',*,*,#5270,.F.);
#7892=ORIENTED_EDGE('',*,*,#5783,.F.);
#7893=ORIENTED_EDGE('',*,*,#5781,.F.);
#7894=ORIENTED_EDGE('',*,*,#5228,.F.);
#7895=ORIENTED_EDGE('',*,*,#5232,.F.);
#7896=ORIENTED_EDGE('',*,*,#5235,.F.);
#7897=ORIENTED_EDGE('',*,*,#5238,.F.);
#7898=ORIENTED_EDGE('',*,*,#5241,.F.);
#7899=ORIENTED_EDGE('',*,*,#5244,.F.);
#7900=ORIENTED_EDGE('',*,*,#5247,.F.);
#7901=ORIENTED_EDGE('',*,*,#5250,.F.);
#7902=ORIENTED_EDGE('',*,*,#5253,.F.);
#7903=ORIENTED_EDGE('',*,*,#5256,.F.);
#7904=ORIENTED_EDGE('',*,*,#5259,.F.);
#7905=ORIENTED_EDGE('',*,*,#5262,.F.);
#7906=ORIENTED_EDGE('',*,*,#5265,.F.);
#7907=ORIENTED_EDGE('',*,*,#5268,.F.);
#7908=ORIENTED_EDGE('',*,*,#5271,.F.);
#7909=ORIENTED_EDGE('',*,*,#5782,.F.);
#7910=ORIENTED_EDGE('',*,*,#5276,.F.);
#7911=ORIENTED_EDGE('',*,*,#5784,.F.);
#7912=ORIENTED_EDGE('',*,*,#5224,.F.);
#7913=ORIENTED_EDGE('',*,*,#5785,.F.);
#7914=ORIENTED_EDGE('',*,*,#5222,.F.);
#7915=ORIENTED_EDGE('',*,*,#5219,.F.);
#7916=ORIENTED_EDGE('',*,*,#5216,.F.);
#7917=ORIENTED_EDGE('',*,*,#5213,.F.);
#7918=ORIENTED_EDGE('',*,*,#5210,.F.);
#7919=ORIENTED_EDGE('',*,*,#5207,.F.);
#7920=ORIENTED_EDGE('',*,*,#5204,.F.);
#7921=ORIENTED_EDGE('',*,*,#5201,.F.);
#7922=ORIENTED_EDGE('',*,*,#5198,.F.);
#7923=ORIENTED_EDGE('',*,*,#5195,.F.);
#7924=ORIENTED_EDGE('',*,*,#5192,.F.);
#7925=ORIENTED_EDGE('',*,*,#5189,.F.);
#7926=ORIENTED_EDGE('',*,*,#5186,.F.);
#7927=ORIENTED_EDGE('',*,*,#5183,.F.);
#7928=ORIENTED_EDGE('',*,*,#5180,.F.);
#7929=ORIENTED_EDGE('',*,*,#5780,.F.);
#7930=ORIENTED_EDGE('',*,*,#5178,.F.);
#7931=ORIENTED_EDGE('',*,*,#5185,.F.);
#7932=ORIENTED_EDGE('',*,*,#5188,.F.);
#7933=ORIENTED_EDGE('',*,*,#5191,.F.);
#7934=ORIENTED_EDGE('',*,*,#5194,.F.);
#7935=ORIENTED_EDGE('',*,*,#5197,.F.);
#7936=ORIENTED_EDGE('',*,*,#5200,.F.);
#7937=ORIENTED_EDGE('',*,*,#5203,.F.);
#7938=ORIENTED_EDGE('',*,*,#5206,.F.);
#7939=ORIENTED_EDGE('',*,*,#5209,.F.);
#7940=ORIENTED_EDGE('',*,*,#5212,.F.);
#7941=ORIENTED_EDGE('',*,*,#5215,.F.);
#7942=ORIENTED_EDGE('',*,*,#5218,.F.);
#7943=ORIENTED_EDGE('',*,*,#5221,.F.);
#7944=ORIENTED_EDGE('',*,*,#5786,.F.);
#7945=ORIENTED_EDGE('',*,*,#5226,.F.);
#7946=ORIENTED_EDGE('',*,*,#5787,.F.);
#7947=ORIENTED_EDGE('',*,*,#5274,.T.);
#7948=ORIENTED_EDGE('',*,*,#5783,.T.);
#7949=ORIENTED_EDGE('',*,*,#5272,.T.);
#7950=ORIENTED_EDGE('',*,*,#5269,.T.);
#7951=ORIENTED_EDGE('',*,*,#5266,.T.);
#7952=ORIENTED_EDGE('',*,*,#5263,.T.);
#7953=ORIENTED_EDGE('',*,*,#5260,.T.);
#7954=ORIENTED_EDGE('',*,*,#5257,.T.);
#7955=ORIENTED_EDGE('',*,*,#5254,.T.);
#7956=ORIENTED_EDGE('',*,*,#5251,.T.);
#7957=ORIENTED_EDGE('',*,*,#5248,.T.);
#7958=ORIENTED_EDGE('',*,*,#5245,.T.);
#7959=ORIENTED_EDGE('',*,*,#5242,.T.);
#7960=ORIENTED_EDGE('',*,*,#5239,.T.);
#7961=ORIENTED_EDGE('',*,*,#5236,.T.);
#7962=ORIENTED_EDGE('',*,*,#5233,.T.);
#7963=ORIENTED_EDGE('',*,*,#5230,.T.);
#7964=ORIENTED_EDGE('',*,*,#5223,.T.);
#7965=ORIENTED_EDGE('',*,*,#5786,.T.);
#7966=ORIENTED_EDGE('',*,*,#5220,.F.);
#7967=ORIENTED_EDGE('',*,*,#5785,.T.);
#7968=ORIENTED_EDGE('',*,*,#5079,.F.);
#7969=ORIENTED_EDGE('',*,*,#5788,.T.);
#7970=ORIENTED_EDGE('',*,*,#5129,.T.);
#7971=ORIENTED_EDGE('',*,*,#5789,.T.);
#7972=ORIENTED_EDGE('',*,*,#5173,.T.);
#7973=ORIENTED_EDGE('',*,*,#5790,.T.);
#7974=ORIENTED_EDGE('',*,*,#5170,.F.);
#7975=ORIENTED_EDGE('',*,*,#5791,.F.);
#7976=ORIENTED_EDGE('',*,*,#5789,.F.);
#7977=ORIENTED_EDGE('',*,*,#5128,.F.);
#7978=ORIENTED_EDGE('',*,*,#5132,.F.);
#7979=ORIENTED_EDGE('',*,*,#5135,.F.);
#7980=ORIENTED_EDGE('',*,*,#5138,.F.);
#7981=ORIENTED_EDGE('',*,*,#5141,.F.);
#7982=ORIENTED_EDGE('',*,*,#5144,.F.);
#7983=ORIENTED_EDGE('',*,*,#5147,.F.);
#7984=ORIENTED_EDGE('',*,*,#5150,.F.);
#7985=ORIENTED_EDGE('',*,*,#5153,.F.);
#7986=ORIENTED_EDGE('',*,*,#5156,.F.);
#7987=ORIENTED_EDGE('',*,*,#5159,.F.);
#7988=ORIENTED_EDGE('',*,*,#5162,.F.);
#7989=ORIENTED_EDGE('',*,*,#5165,.F.);
#7990=ORIENTED_EDGE('',*,*,#5168,.F.);
#7991=ORIENTED_EDGE('',*,*,#5171,.F.);
#7992=ORIENTED_EDGE('',*,*,#5790,.F.);
#7993=ORIENTED_EDGE('',*,*,#5176,.F.);
#7994=ORIENTED_EDGE('',*,*,#5792,.F.);
#7995=ORIENTED_EDGE('',*,*,#5124,.F.);
#7996=ORIENTED_EDGE('',*,*,#5793,.F.);
#7997=ORIENTED_EDGE('',*,*,#5122,.F.);
#7998=ORIENTED_EDGE('',*,*,#5119,.F.);
#7999=ORIENTED_EDGE('',*,*,#5116,.F.);
#8000=ORIENTED_EDGE('',*,*,#5113,.F.);
#8001=ORIENTED_EDGE('',*,*,#5110,.F.);
#8002=ORIENTED_EDGE('',*,*,#5107,.F.);
#8003=ORIENTED_EDGE('',*,*,#5104,.F.);
#8004=ORIENTED_EDGE('',*,*,#5101,.F.);
#8005=ORIENTED_EDGE('',*,*,#5098,.F.);
#8006=ORIENTED_EDGE('',*,*,#5095,.F.);
#8007=ORIENTED_EDGE('',*,*,#5092,.F.);
#8008=ORIENTED_EDGE('',*,*,#5089,.F.);
#8009=ORIENTED_EDGE('',*,*,#5086,.F.);
#8010=ORIENTED_EDGE('',*,*,#5083,.F.);
#8011=ORIENTED_EDGE('',*,*,#5080,.F.);
#8012=ORIENTED_EDGE('',*,*,#5788,.F.);
#8013=ORIENTED_EDGE('',*,*,#5078,.F.);
#8014=ORIENTED_EDGE('',*,*,#5085,.F.);
#8015=ORIENTED_EDGE('',*,*,#5088,.F.);
#8016=ORIENTED_EDGE('',*,*,#5091,.F.);
#8017=ORIENTED_EDGE('',*,*,#5094,.F.);
#8018=ORIENTED_EDGE('',*,*,#5097,.F.);
#8019=ORIENTED_EDGE('',*,*,#5100,.F.);
#8020=ORIENTED_EDGE('',*,*,#5103,.F.);
#8021=ORIENTED_EDGE('',*,*,#5106,.F.);
#8022=ORIENTED_EDGE('',*,*,#5109,.F.);
#8023=ORIENTED_EDGE('',*,*,#5112,.F.);
#8024=ORIENTED_EDGE('',*,*,#5115,.F.);
#8025=ORIENTED_EDGE('',*,*,#5118,.F.);
#8026=ORIENTED_EDGE('',*,*,#5121,.F.);
#8027=ORIENTED_EDGE('',*,*,#5794,.F.);
#8028=ORIENTED_EDGE('',*,*,#5126,.F.);
#8029=ORIENTED_EDGE('',*,*,#5795,.F.);
#8030=ORIENTED_EDGE('',*,*,#5174,.T.);
#8031=ORIENTED_EDGE('',*,*,#5791,.T.);
#8032=ORIENTED_EDGE('',*,*,#5172,.T.);
#8033=ORIENTED_EDGE('',*,*,#5169,.T.);
#8034=ORIENTED_EDGE('',*,*,#5166,.T.);
#8035=ORIENTED_EDGE('',*,*,#5163,.T.);
#8036=ORIENTED_EDGE('',*,*,#5160,.T.);
#8037=ORIENTED_EDGE('',*,*,#5157,.T.);
#8038=ORIENTED_EDGE('',*,*,#5154,.T.);
#8039=ORIENTED_EDGE('',*,*,#5151,.T.);
#8040=ORIENTED_EDGE('',*,*,#5148,.T.);
#8041=ORIENTED_EDGE('',*,*,#5145,.T.);
#8042=ORIENTED_EDGE('',*,*,#5142,.T.);
#8043=ORIENTED_EDGE('',*,*,#5139,.T.);
#8044=ORIENTED_EDGE('',*,*,#5136,.T.);
#8045=ORIENTED_EDGE('',*,*,#5133,.T.);
#8046=ORIENTED_EDGE('',*,*,#5130,.T.);
#8047=ORIENTED_EDGE('',*,*,#5123,.T.);
#8048=ORIENTED_EDGE('',*,*,#5794,.T.);
#8049=ORIENTED_EDGE('',*,*,#5120,.F.);
#8050=ORIENTED_EDGE('',*,*,#5793,.T.);
#8051=ORIENTED_EDGE('',*,*,#4979,.F.);
#8052=ORIENTED_EDGE('',*,*,#5796,.T.);
#8053=ORIENTED_EDGE('',*,*,#5029,.T.);
#8054=ORIENTED_EDGE('',*,*,#5797,.T.);
#8055=ORIENTED_EDGE('',*,*,#5073,.T.);
#8056=ORIENTED_EDGE('',*,*,#5798,.T.);
#8057=ORIENTED_EDGE('',*,*,#5070,.F.);
#8058=ORIENTED_EDGE('',*,*,#5799,.F.);
#8059=ORIENTED_EDGE('',*,*,#5797,.F.);
#8060=ORIENTED_EDGE('',*,*,#5028,.F.);
#8061=ORIENTED_EDGE('',*,*,#5032,.F.);
#8062=ORIENTED_EDGE('',*,*,#5035,.F.);
#8063=ORIENTED_EDGE('',*,*,#5038,.F.);
#8064=ORIENTED_EDGE('',*,*,#5041,.F.);
#8065=ORIENTED_EDGE('',*,*,#5044,.F.);
#8066=ORIENTED_EDGE('',*,*,#5047,.F.);
#8067=ORIENTED_EDGE('',*,*,#5050,.F.);
#8068=ORIENTED_EDGE('',*,*,#5053,.F.);
#8069=ORIENTED_EDGE('',*,*,#5056,.F.);
#8070=ORIENTED_EDGE('',*,*,#5059,.F.);
#8071=ORIENTED_EDGE('',*,*,#5062,.F.);
#8072=ORIENTED_EDGE('',*,*,#5065,.F.);
#8073=ORIENTED_EDGE('',*,*,#5068,.F.);
#8074=ORIENTED_EDGE('',*,*,#5071,.F.);
#8075=ORIENTED_EDGE('',*,*,#5798,.F.);
#8076=ORIENTED_EDGE('',*,*,#5076,.F.);
#8077=ORIENTED_EDGE('',*,*,#5800,.F.);
#8078=ORIENTED_EDGE('',*,*,#5024,.F.);
#8079=ORIENTED_EDGE('',*,*,#5801,.F.);
#8080=ORIENTED_EDGE('',*,*,#5022,.F.);
#8081=ORIENTED_EDGE('',*,*,#5019,.F.);
#8082=ORIENTED_EDGE('',*,*,#5016,.F.);
#8083=ORIENTED_EDGE('',*,*,#5013,.F.);
#8084=ORIENTED_EDGE('',*,*,#5010,.F.);
#8085=ORIENTED_EDGE('',*,*,#5007,.F.);
#8086=ORIENTED_EDGE('',*,*,#5004,.F.);
#8087=ORIENTED_EDGE('',*,*,#5001,.F.);
#8088=ORIENTED_EDGE('',*,*,#4998,.F.);
#8089=ORIENTED_EDGE('',*,*,#4995,.F.);
#8090=ORIENTED_EDGE('',*,*,#4992,.F.);
#8091=ORIENTED_EDGE('',*,*,#4989,.F.);
#8092=ORIENTED_EDGE('',*,*,#4986,.F.);
#8093=ORIENTED_EDGE('',*,*,#4983,.F.);
#8094=ORIENTED_EDGE('',*,*,#4980,.F.);
#8095=ORIENTED_EDGE('',*,*,#5796,.F.);
#8096=ORIENTED_EDGE('',*,*,#4978,.F.);
#8097=ORIENTED_EDGE('',*,*,#4985,.F.);
#8098=ORIENTED_EDGE('',*,*,#4988,.F.);
#8099=ORIENTED_EDGE('',*,*,#4991,.F.);
#8100=ORIENTED_EDGE('',*,*,#4994,.F.);
#8101=ORIENTED_EDGE('',*,*,#4997,.F.);
#8102=ORIENTED_EDGE('',*,*,#5000,.F.);
#8103=ORIENTED_EDGE('',*,*,#5003,.F.);
#8104=ORIENTED_EDGE('',*,*,#5006,.F.);
#8105=ORIENTED_EDGE('',*,*,#5009,.F.);
#8106=ORIENTED_EDGE('',*,*,#5012,.F.);
#8107=ORIENTED_EDGE('',*,*,#5015,.F.);
#8108=ORIENTED_EDGE('',*,*,#5018,.F.);
#8109=ORIENTED_EDGE('',*,*,#5021,.F.);
#8110=ORIENTED_EDGE('',*,*,#5802,.F.);
#8111=ORIENTED_EDGE('',*,*,#5026,.F.);
#8112=ORIENTED_EDGE('',*,*,#5803,.F.);
#8113=ORIENTED_EDGE('',*,*,#5074,.T.);
#8114=ORIENTED_EDGE('',*,*,#5799,.T.);
#8115=ORIENTED_EDGE('',*,*,#5072,.T.);
#8116=ORIENTED_EDGE('',*,*,#5069,.T.);
#8117=ORIENTED_EDGE('',*,*,#5066,.T.);
#8118=ORIENTED_EDGE('',*,*,#5063,.T.);
#8119=ORIENTED_EDGE('',*,*,#5060,.T.);
#8120=ORIENTED_EDGE('',*,*,#5057,.T.);
#8121=ORIENTED_EDGE('',*,*,#5054,.T.);
#8122=ORIENTED_EDGE('',*,*,#5051,.T.);
#8123=ORIENTED_EDGE('',*,*,#5048,.T.);
#8124=ORIENTED_EDGE('',*,*,#5045,.T.);
#8125=ORIENTED_EDGE('',*,*,#5042,.T.);
#8126=ORIENTED_EDGE('',*,*,#5039,.T.);
#8127=ORIENTED_EDGE('',*,*,#5036,.T.);
#8128=ORIENTED_EDGE('',*,*,#5033,.T.);
#8129=ORIENTED_EDGE('',*,*,#5030,.T.);
#8130=ORIENTED_EDGE('',*,*,#5023,.T.);
#8131=ORIENTED_EDGE('',*,*,#5802,.T.);
#8132=ORIENTED_EDGE('',*,*,#5020,.F.);
#8133=ORIENTED_EDGE('',*,*,#5801,.T.);
#8134=ORIENTED_EDGE('',*,*,#4879,.F.);
#8135=ORIENTED_EDGE('',*,*,#5804,.T.);
#8136=ORIENTED_EDGE('',*,*,#4929,.T.);
#8137=ORIENTED_EDGE('',*,*,#5805,.T.);
#8138=ORIENTED_EDGE('',*,*,#4973,.T.);
#8139=ORIENTED_EDGE('',*,*,#5806,.T.);
#8140=ORIENTED_EDGE('',*,*,#4970,.F.);
#8141=ORIENTED_EDGE('',*,*,#5807,.F.);
#8142=ORIENTED_EDGE('',*,*,#5805,.F.);
#8143=ORIENTED_EDGE('',*,*,#4928,.F.);
#8144=ORIENTED_EDGE('',*,*,#4932,.F.);
#8145=ORIENTED_EDGE('',*,*,#4935,.F.);
#8146=ORIENTED_EDGE('',*,*,#4938,.F.);
#8147=ORIENTED_EDGE('',*,*,#4941,.F.);
#8148=ORIENTED_EDGE('',*,*,#4944,.F.);
#8149=ORIENTED_EDGE('',*,*,#4947,.F.);
#8150=ORIENTED_EDGE('',*,*,#4950,.F.);
#8151=ORIENTED_EDGE('',*,*,#4953,.F.);
#8152=ORIENTED_EDGE('',*,*,#4956,.F.);
#8153=ORIENTED_EDGE('',*,*,#4959,.F.);
#8154=ORIENTED_EDGE('',*,*,#4962,.F.);
#8155=ORIENTED_EDGE('',*,*,#4965,.F.);
#8156=ORIENTED_EDGE('',*,*,#4968,.F.);
#8157=ORIENTED_EDGE('',*,*,#4971,.F.);
#8158=ORIENTED_EDGE('',*,*,#5806,.F.);
#8159=ORIENTED_EDGE('',*,*,#4976,.F.);
#8160=ORIENTED_EDGE('',*,*,#5808,.F.);
#8161=ORIENTED_EDGE('',*,*,#4924,.F.);
#8162=ORIENTED_EDGE('',*,*,#5809,.F.);
#8163=ORIENTED_EDGE('',*,*,#4922,.F.);
#8164=ORIENTED_EDGE('',*,*,#4919,.F.);
#8165=ORIENTED_EDGE('',*,*,#4916,.F.);
#8166=ORIENTED_EDGE('',*,*,#4913,.F.);
#8167=ORIENTED_EDGE('',*,*,#4910,.F.);
#8168=ORIENTED_EDGE('',*,*,#4907,.F.);
#8169=ORIENTED_EDGE('',*,*,#4904,.F.);
#8170=ORIENTED_EDGE('',*,*,#4901,.F.);
#8171=ORIENTED_EDGE('',*,*,#4898,.F.);
#8172=ORIENTED_EDGE('',*,*,#4895,.F.);
#8173=ORIENTED_EDGE('',*,*,#4892,.F.);
#8174=ORIENTED_EDGE('',*,*,#4889,.F.);
#8175=ORIENTED_EDGE('',*,*,#4886,.F.);
#8176=ORIENTED_EDGE('',*,*,#4883,.F.);
#8177=ORIENTED_EDGE('',*,*,#4880,.F.);
#8178=ORIENTED_EDGE('',*,*,#5804,.F.);
#8179=ORIENTED_EDGE('',*,*,#4878,.F.);
#8180=ORIENTED_EDGE('',*,*,#4885,.F.);
#8181=ORIENTED_EDGE('',*,*,#4888,.F.);
#8182=ORIENTED_EDGE('',*,*,#4891,.F.);
#8183=ORIENTED_EDGE('',*,*,#4894,.F.);
#8184=ORIENTED_EDGE('',*,*,#4897,.F.);
#8185=ORIENTED_EDGE('',*,*,#4900,.F.);
#8186=ORIENTED_EDGE('',*,*,#4903,.F.);
#8187=ORIENTED_EDGE('',*,*,#4906,.F.);
#8188=ORIENTED_EDGE('',*,*,#4909,.F.);
#8189=ORIENTED_EDGE('',*,*,#4912,.F.);
#8190=ORIENTED_EDGE('',*,*,#4915,.F.);
#8191=ORIENTED_EDGE('',*,*,#4918,.F.);
#8192=ORIENTED_EDGE('',*,*,#4921,.F.);
#8193=ORIENTED_EDGE('',*,*,#5810,.F.);
#8194=ORIENTED_EDGE('',*,*,#4926,.F.);
#8195=ORIENTED_EDGE('',*,*,#5811,.F.);
#8196=ORIENTED_EDGE('',*,*,#4974,.T.);
#8197=ORIENTED_EDGE('',*,*,#5807,.T.);
#8198=ORIENTED_EDGE('',*,*,#4972,.T.);
#8199=ORIENTED_EDGE('',*,*,#4969,.T.);
#8200=ORIENTED_EDGE('',*,*,#4966,.T.);
#8201=ORIENTED_EDGE('',*,*,#4963,.T.);
#8202=ORIENTED_EDGE('',*,*,#4960,.T.);
#8203=ORIENTED_EDGE('',*,*,#4957,.T.);
#8204=ORIENTED_EDGE('',*,*,#4954,.T.);
#8205=ORIENTED_EDGE('',*,*,#4951,.T.);
#8206=ORIENTED_EDGE('',*,*,#4948,.T.);
#8207=ORIENTED_EDGE('',*,*,#4945,.T.);
#8208=ORIENTED_EDGE('',*,*,#4942,.T.);
#8209=ORIENTED_EDGE('',*,*,#4939,.T.);
#8210=ORIENTED_EDGE('',*,*,#4936,.T.);
#8211=ORIENTED_EDGE('',*,*,#4933,.T.);
#8212=ORIENTED_EDGE('',*,*,#4930,.T.);
#8213=ORIENTED_EDGE('',*,*,#4923,.T.);
#8214=ORIENTED_EDGE('',*,*,#5810,.T.);
#8215=ORIENTED_EDGE('',*,*,#4920,.F.);
#8216=ORIENTED_EDGE('',*,*,#5809,.T.);
#8217=ORIENTED_EDGE('',*,*,#4982,.F.);
#8218=ORIENTED_EDGE('',*,*,#4882,.F.);
#8219=ORIENTED_EDGE('',*,*,#5082,.F.);
#8220=ORIENTED_EDGE('',*,*,#5182,.F.);
#8221=ORIENTED_EDGE('',*,*,#5812,.F.);
#8222=ORIENTED_EDGE('',*,*,#5813,.T.);
#8223=ORIENTED_EDGE('',*,*,#5814,.F.);
#8224=ORIENTED_EDGE('',*,*,#5813,.F.);
#8225=ORIENTED_EDGE('',*,*,#5815,.F.);
#8226=ORIENTED_EDGE('',*,*,#5816,.T.);
#8227=ORIENTED_EDGE('',*,*,#5817,.F.);
#8228=ORIENTED_EDGE('',*,*,#5816,.F.);
#8229=ORIENTED_EDGE('',*,*,#5818,.F.);
#8230=ORIENTED_EDGE('',*,*,#5819,.T.);
#8231=ORIENTED_EDGE('',*,*,#5820,.F.);
#8232=ORIENTED_EDGE('',*,*,#5819,.F.);
#8233=ORIENTED_EDGE('',*,*,#5821,.F.);
#8234=ORIENTED_EDGE('',*,*,#5822,.T.);
#8235=ORIENTED_EDGE('',*,*,#5823,.F.);
#8236=ORIENTED_EDGE('',*,*,#5822,.F.);
#8237=ORIENTED_EDGE('',*,*,#5824,.F.);
#8238=ORIENTED_EDGE('',*,*,#5825,.T.);
#8239=ORIENTED_EDGE('',*,*,#5826,.F.);
#8240=ORIENTED_EDGE('',*,*,#5825,.F.);
#8241=ORIENTED_EDGE('',*,*,#5827,.F.);
#8242=ORIENTED_EDGE('',*,*,#5828,.T.);
#8243=ORIENTED_EDGE('',*,*,#5829,.F.);
#8244=ORIENTED_EDGE('',*,*,#5828,.F.);
#8245=ORIENTED_EDGE('',*,*,#5830,.F.);
#8246=ORIENTED_EDGE('',*,*,#5831,.T.);
#8247=ORIENTED_EDGE('',*,*,#5832,.F.);
#8248=ORIENTED_EDGE('',*,*,#5831,.F.);
#8249=ORIENTED_EDGE('',*,*,#5833,.F.);
#8250=ORIENTED_EDGE('',*,*,#5834,.T.);
#8251=ORIENTED_EDGE('',*,*,#5835,.F.);
#8252=ORIENTED_EDGE('',*,*,#5834,.F.);
#8253=ORIENTED_EDGE('',*,*,#5836,.F.);
#8254=ORIENTED_EDGE('',*,*,#5837,.T.);
#8255=ORIENTED_EDGE('',*,*,#5767,.F.);
#8256=ORIENTED_EDGE('',*,*,#5779,.T.);
#8257=ORIENTED_EDGE('',*,*,#5778,.T.);
#8258=ORIENTED_EDGE('',*,*,#5770,.F.);
#8259=ORIENTED_EDGE('',*,*,#5838,.T.);
#8260=ORIENTED_EDGE('',*,*,#5839,.F.);
#8261=ORIENTED_EDGE('',*,*,#5838,.F.);
#8262=ORIENTED_EDGE('',*,*,#5765,.T.);
#8263=ORIENTED_EDGE('',*,*,#5329,.T.);
#8264=ORIENTED_EDGE('',*,*,#5772,.T.);
#8265=ORIENTED_EDGE('',*,*,#5837,.F.);
#8266=ORIENTED_EDGE('',*,*,#5840,.F.);
#8267=ORIENTED_EDGE('',*,*,#5841,.T.);
#8268=ORIENTED_EDGE('',*,*,#5842,.F.);
#8269=ORIENTED_EDGE('',*,*,#5841,.F.);
#8270=ORIENTED_EDGE('',*,*,#5843,.F.);
#8271=ORIENTED_EDGE('',*,*,#5844,.T.);
#8272=ORIENTED_EDGE('',*,*,#5845,.F.);
#8273=ORIENTED_EDGE('',*,*,#5844,.F.);
#8274=ORIENTED_EDGE('',*,*,#5846,.F.);
#8275=ORIENTED_EDGE('',*,*,#5847,.T.);
#8276=ORIENTED_EDGE('',*,*,#5848,.F.);
#8277=ORIENTED_EDGE('',*,*,#5847,.F.);
#8278=ORIENTED_EDGE('',*,*,#5849,.F.);
#8279=ORIENTED_EDGE('',*,*,#5850,.T.);
#8280=ORIENTED_EDGE('',*,*,#5851,.F.);
#8281=ORIENTED_EDGE('',*,*,#5850,.F.);
#8282=ORIENTED_EDGE('',*,*,#5852,.F.);
#8283=ORIENTED_EDGE('',*,*,#5853,.T.);
#8284=ORIENTED_EDGE('',*,*,#5854,.F.);
#8285=ORIENTED_EDGE('',*,*,#5853,.F.);
#8286=ORIENTED_EDGE('',*,*,#5855,.F.);
#8287=ORIENTED_EDGE('',*,*,#5856,.T.);
#8288=ORIENTED_EDGE('',*,*,#5857,.F.);
#8289=ORIENTED_EDGE('',*,*,#5856,.F.);
#8290=ORIENTED_EDGE('',*,*,#5858,.F.);
#8291=ORIENTED_EDGE('',*,*,#5859,.T.);
#8292=ORIENTED_EDGE('',*,*,#5860,.F.);
#8293=ORIENTED_EDGE('',*,*,#5859,.F.);
#8294=ORIENTED_EDGE('',*,*,#5861,.F.);
#8295=ORIENTED_EDGE('',*,*,#5862,.T.);
#8296=ORIENTED_EDGE('',*,*,#5752,.F.);
#8297=ORIENTED_EDGE('',*,*,#5764,.T.);
#8298=ORIENTED_EDGE('',*,*,#5763,.T.);
#8299=ORIENTED_EDGE('',*,*,#5755,.F.);
#8300=ORIENTED_EDGE('',*,*,#5863,.T.);
#8301=ORIENTED_EDGE('',*,*,#5864,.F.);
#8302=ORIENTED_EDGE('',*,*,#5863,.F.);
#8303=ORIENTED_EDGE('',*,*,#5750,.T.);
#8304=ORIENTED_EDGE('',*,*,#5280,.T.);
#8305=ORIENTED_EDGE('',*,*,#5757,.T.);
#8306=ORIENTED_EDGE('',*,*,#5862,.F.);
#8307=ORIENTED_EDGE('',*,*,#5865,.F.);
#8308=ORIENTED_EDGE('',*,*,#5866,.T.);
#8309=ORIENTED_EDGE('',*,*,#5867,.F.);
#8310=ORIENTED_EDGE('',*,*,#5866,.F.);
#8311=ORIENTED_EDGE('',*,*,#5868,.F.);
#8312=ORIENTED_EDGE('',*,*,#5869,.T.);
#8313=ORIENTED_EDGE('',*,*,#5870,.T.);
#8314=ORIENTED_EDGE('',*,*,#5871,.F.);
#8315=ORIENTED_EDGE('',*,*,#5872,.F.);
#8316=ORIENTED_EDGE('',*,*,#5873,.T.);
#8317=ORIENTED_EDGE('',*,*,#5874,.T.);
#8318=ORIENTED_EDGE('',*,*,#5869,.F.);
#8319=ORIENTED_EDGE('',*,*,#5867,.T.);
#8320=ORIENTED_EDGE('',*,*,#5864,.T.);
#8321=ORIENTED_EDGE('',*,*,#5860,.T.);
#8322=ORIENTED_EDGE('',*,*,#5857,.T.);
#8323=ORIENTED_EDGE('',*,*,#5854,.T.);
#8324=ORIENTED_EDGE('',*,*,#5851,.T.);
#8325=ORIENTED_EDGE('',*,*,#5848,.T.);
#8326=ORIENTED_EDGE('',*,*,#5845,.T.);
#8327=ORIENTED_EDGE('',*,*,#5842,.T.);
#8328=ORIENTED_EDGE('',*,*,#5839,.T.);
#8329=ORIENTED_EDGE('',*,*,#5835,.T.);
#8330=ORIENTED_EDGE('',*,*,#5832,.T.);
#8331=ORIENTED_EDGE('',*,*,#5829,.T.);
#8332=ORIENTED_EDGE('',*,*,#5826,.T.);
#8333=ORIENTED_EDGE('',*,*,#5823,.T.);
#8334=ORIENTED_EDGE('',*,*,#5820,.T.);
#8335=ORIENTED_EDGE('',*,*,#5817,.T.);
#8336=ORIENTED_EDGE('',*,*,#5814,.T.);
#8337=ORIENTED_EDGE('',*,*,#5875,.F.);
#8338=ORIENTED_EDGE('',*,*,#5876,.T.);
#8339=ORIENTED_EDGE('',*,*,#5877,.T.);
#8340=ORIENTED_EDGE('',*,*,#5873,.F.);
#8341=ORIENTED_EDGE('',*,*,#5878,.F.);
#8342=ORIENTED_EDGE('',*,*,#5871,.T.);
#8343=ORIENTED_EDGE('',*,*,#5879,.T.);
#8344=ORIENTED_EDGE('',*,*,#5876,.F.);
#8345=ORIENTED_EDGE('',*,*,#5879,.F.);
#8346=ORIENTED_EDGE('',*,*,#5870,.F.);
#8347=ORIENTED_EDGE('',*,*,#5874,.F.);
#8348=ORIENTED_EDGE('',*,*,#5877,.F.);
#8349=ORIENTED_EDGE('',*,*,#5717,.T.);
#8350=ORIENTED_EDGE('',*,*,#5687,.T.);
#8351=ORIENTED_EDGE('',*,*,#5720,.T.);
#8352=ORIENTED_EDGE('',*,*,#5691,.T.);
#8353=ORIENTED_EDGE('',*,*,#5727,.T.);
#8354=ORIENTED_EDGE('',*,*,#5880,.T.);
#8355=ORIENTED_EDGE('',*,*,#5881,.F.);
#8356=ORIENTED_EDGE('',*,*,#5882,.F.);
#8357=ORIENTED_EDGE('',*,*,#5728,.T.);
#8358=ORIENTED_EDGE('',*,*,#5882,.T.);
#8359=ORIENTED_EDGE('',*,*,#5883,.F.);
#8360=ORIENTED_EDGE('',*,*,#5884,.F.);
#8361=ORIENTED_EDGE('',*,*,#5865,.T.);
#8362=ORIENTED_EDGE('',*,*,#5861,.T.);
#8363=ORIENTED_EDGE('',*,*,#5858,.T.);
#8364=ORIENTED_EDGE('',*,*,#5855,.T.);
#8365=ORIENTED_EDGE('',*,*,#5852,.T.);
#8366=ORIENTED_EDGE('',*,*,#5849,.T.);
#8367=ORIENTED_EDGE('',*,*,#5846,.T.);
#8368=ORIENTED_EDGE('',*,*,#5843,.T.);
#8369=ORIENTED_EDGE('',*,*,#5840,.T.);
#8370=ORIENTED_EDGE('',*,*,#5836,.T.);
#8371=ORIENTED_EDGE('',*,*,#5833,.T.);
#8372=ORIENTED_EDGE('',*,*,#5830,.T.);
#8373=ORIENTED_EDGE('',*,*,#5827,.T.);
#8374=ORIENTED_EDGE('',*,*,#5824,.T.);
#8375=ORIENTED_EDGE('',*,*,#5821,.T.);
#8376=ORIENTED_EDGE('',*,*,#5818,.T.);
#8377=ORIENTED_EDGE('',*,*,#5815,.T.);
#8378=ORIENTED_EDGE('',*,*,#5812,.T.);
#8379=ORIENTED_EDGE('',*,*,#5729,.T.);
#8380=ORIENTED_EDGE('',*,*,#5884,.T.);
#8381=ORIENTED_EDGE('',*,*,#5885,.F.);
#8382=ORIENTED_EDGE('',*,*,#5886,.F.);
#8383=ORIENTED_EDGE('',*,*,#5726,.T.);
#8384=ORIENTED_EDGE('',*,*,#5886,.T.);
#8385=ORIENTED_EDGE('',*,*,#5887,.F.);
#8386=ORIENTED_EDGE('',*,*,#5880,.F.);
#8387=ORIENTED_EDGE('',*,*,#5887,.T.);
#8388=ORIENTED_EDGE('',*,*,#5885,.T.);
#8389=ORIENTED_EDGE('',*,*,#5883,.T.);
#8390=ORIENTED_EDGE('',*,*,#5881,.T.);
#8391=ORIENTED_EDGE('',*,*,#5787,.T.);
#8392=ORIENTED_EDGE('',*,*,#5225,.T.);
#8393=ORIENTED_EDGE('',*,*,#5784,.T.);
#8394=ORIENTED_EDGE('',*,*,#5275,.T.);
#8395=ORIENTED_EDGE('',*,*,#5795,.T.);
#8396=ORIENTED_EDGE('',*,*,#5125,.T.);
#8397=ORIENTED_EDGE('',*,*,#5792,.T.);
#8398=ORIENTED_EDGE('',*,*,#5175,.T.);
#8399=ORIENTED_EDGE('',*,*,#5803,.T.);
#8400=ORIENTED_EDGE('',*,*,#5025,.T.);
#8401=ORIENTED_EDGE('',*,*,#5800,.T.);
#8402=ORIENTED_EDGE('',*,*,#5075,.T.);
#8403=ORIENTED_EDGE('',*,*,#5811,.T.);
#8404=ORIENTED_EDGE('',*,*,#4925,.T.);
#8405=ORIENTED_EDGE('',*,*,#5808,.T.);
#8406=ORIENTED_EDGE('',*,*,#4975,.T.);
#8407=ORIENTED_EDGE('',*,*,#5868,.T.);
#8408=ORIENTED_EDGE('',*,*,#5878,.T.);
#8409=ORIENTED_EDGE('',*,*,#5875,.T.);
#8410=ORIENTED_EDGE('',*,*,#5872,.T.);
#8411=ORIENTED_EDGE('',*,*,#5888,.F.);
#8412=ORIENTED_EDGE('',*,*,#5889,.T.);
#8413=ORIENTED_EDGE('',*,*,#5890,.F.);
#8414=ORIENTED_EDGE('',*,*,#5889,.F.);
#8415=ORIENTED_EDGE('',*,*,#5891,.F.);
#8416=ORIENTED_EDGE('',*,*,#5892,.T.);
#8417=ORIENTED_EDGE('',*,*,#5893,.F.);
#8418=ORIENTED_EDGE('',*,*,#5892,.F.);
#8419=ORIENTED_EDGE('',*,*,#5894,.F.);
#8420=ORIENTED_EDGE('',*,*,#5895,.T.);
#8421=ORIENTED_EDGE('',*,*,#5896,.F.);
#8422=ORIENTED_EDGE('',*,*,#5895,.F.);
#8423=ORIENTED_EDGE('',*,*,#5897,.F.);
#8424=ORIENTED_EDGE('',*,*,#5898,.T.);
#8425=ORIENTED_EDGE('',*,*,#5899,.F.);
#8426=ORIENTED_EDGE('',*,*,#5898,.F.);
#8427=ORIENTED_EDGE('',*,*,#5900,.T.);
#8428=ORIENTED_EDGE('',*,*,#5901,.T.);
#8429=ORIENTED_EDGE('',*,*,#5902,.F.);
#8430=ORIENTED_EDGE('',*,*,#5903,.F.);
#8431=ORIENTED_EDGE('',*,*,#5904,.T.);
#8432=ORIENTED_EDGE('',*,*,#5903,.T.);
#8433=ORIENTED_EDGE('',*,*,#5905,.F.);
#8434=ORIENTED_EDGE('',*,*,#5906,.F.);
#8435=ORIENTED_EDGE('',*,*,#5907,.T.);
#8436=ORIENTED_EDGE('',*,*,#5906,.T.);
#8437=ORIENTED_EDGE('',*,*,#5908,.F.);
#8438=ORIENTED_EDGE('',*,*,#5909,.F.);
#8439=ORIENTED_EDGE('',*,*,#5910,.T.);
#8440=ORIENTED_EDGE('',*,*,#5909,.T.);
#8441=ORIENTED_EDGE('',*,*,#5911,.F.);
#8442=ORIENTED_EDGE('',*,*,#5901,.F.);
#8443=ORIENTED_EDGE('',*,*,#5911,.T.);
#8444=ORIENTED_EDGE('',*,*,#5908,.T.);
#8445=ORIENTED_EDGE('',*,*,#5905,.T.);
#8446=ORIENTED_EDGE('',*,*,#5902,.T.);
#8447=ORIENTED_EDGE('',*,*,#5888,.T.);
#8448=ORIENTED_EDGE('',*,*,#5891,.T.);
#8449=ORIENTED_EDGE('',*,*,#5894,.T.);
#8450=ORIENTED_EDGE('',*,*,#5897,.T.);
#8451=ORIENTED_EDGE('',*,*,#5910,.F.);
#8452=ORIENTED_EDGE('',*,*,#5900,.F.);
#8453=ORIENTED_EDGE('',*,*,#5904,.F.);
#8454=ORIENTED_EDGE('',*,*,#5907,.F.);
#8455=ORIENTED_EDGE('',*,*,#5890,.T.);
#8456=ORIENTED_EDGE('',*,*,#5893,.T.);
#8457=ORIENTED_EDGE('',*,*,#5896,.T.);
#8458=ORIENTED_EDGE('',*,*,#5899,.T.);
#8459=ORIENTED_EDGE('',*,*,#5912,.F.);
#8460=ORIENTED_EDGE('',*,*,#5913,.T.);
#8461=ORIENTED_EDGE('',*,*,#5914,.F.);
#8462=ORIENTED_EDGE('',*,*,#5913,.F.);
#8463=ORIENTED_EDGE('',*,*,#5915,.F.);
#8464=ORIENTED_EDGE('',*,*,#5916,.T.);
#8465=ORIENTED_EDGE('',*,*,#5917,.F.);
#8466=ORIENTED_EDGE('',*,*,#5916,.F.);
#8467=ORIENTED_EDGE('',*,*,#5918,.F.);
#8468=ORIENTED_EDGE('',*,*,#5919,.T.);
#8469=ORIENTED_EDGE('',*,*,#5920,.F.);
#8470=ORIENTED_EDGE('',*,*,#5919,.F.);
#8471=ORIENTED_EDGE('',*,*,#5921,.F.);
#8472=ORIENTED_EDGE('',*,*,#5922,.T.);
#8473=ORIENTED_EDGE('',*,*,#5923,.F.);
#8474=ORIENTED_EDGE('',*,*,#5922,.F.);
#8475=ORIENTED_EDGE('',*,*,#5924,.F.);
#8476=ORIENTED_EDGE('',*,*,#5925,.T.);
#8477=ORIENTED_EDGE('',*,*,#5926,.F.);
#8478=ORIENTED_EDGE('',*,*,#5927,.F.);
#8479=ORIENTED_EDGE('',*,*,#5928,.F.);
#8480=ORIENTED_EDGE('',*,*,#5929,.T.);
#8481=ORIENTED_EDGE('',*,*,#5930,.F.);
#8482=ORIENTED_EDGE('',*,*,#5925,.F.);
#8483=ORIENTED_EDGE('',*,*,#5931,.F.);
#8484=ORIENTED_EDGE('',*,*,#5932,.T.);
#8485=ORIENTED_EDGE('',*,*,#5933,.F.);
#8486=ORIENTED_EDGE('',*,*,#5929,.F.);
#8487=ORIENTED_EDGE('',*,*,#5934,.F.);
#8488=ORIENTED_EDGE('',*,*,#5927,.T.);
#8489=ORIENTED_EDGE('',*,*,#5935,.F.);
#8490=ORIENTED_EDGE('',*,*,#5932,.F.);
#8491=ORIENTED_EDGE('',*,*,#5936,.T.);
#8492=ORIENTED_EDGE('',*,*,#5937,.T.);
#8493=ORIENTED_EDGE('',*,*,#5938,.F.);
#8494=ORIENTED_EDGE('',*,*,#5939,.F.);
#8495=ORIENTED_EDGE('',*,*,#5940,.T.);
#8496=ORIENTED_EDGE('',*,*,#5939,.T.);
#8497=ORIENTED_EDGE('',*,*,#5941,.F.);
#8498=ORIENTED_EDGE('',*,*,#5942,.F.);
#8499=ORIENTED_EDGE('',*,*,#5943,.T.);
#8500=ORIENTED_EDGE('',*,*,#5942,.T.);
#8501=ORIENTED_EDGE('',*,*,#5944,.F.);
#8502=ORIENTED_EDGE('',*,*,#5945,.F.);
#8503=ORIENTED_EDGE('',*,*,#5946,.T.);
#8504=ORIENTED_EDGE('',*,*,#5945,.T.);
#8505=ORIENTED_EDGE('',*,*,#5947,.F.);
#8506=ORIENTED_EDGE('',*,*,#5937,.F.);
#8507=ORIENTED_EDGE('',*,*,#5947,.T.);
#8508=ORIENTED_EDGE('',*,*,#5944,.T.);
#8509=ORIENTED_EDGE('',*,*,#5941,.T.);
#8510=ORIENTED_EDGE('',*,*,#5938,.T.);
#8511=ORIENTED_EDGE('',*,*,#5924,.T.);
#8512=ORIENTED_EDGE('',*,*,#5934,.T.);
#8513=ORIENTED_EDGE('',*,*,#5931,.T.);
#8514=ORIENTED_EDGE('',*,*,#5928,.T.);
#8515=ORIENTED_EDGE('',*,*,#5921,.T.);
#8516=ORIENTED_EDGE('',*,*,#5918,.T.);
#8517=ORIENTED_EDGE('',*,*,#5915,.T.);
#8518=ORIENTED_EDGE('',*,*,#5912,.T.);
#8519=ORIENTED_EDGE('',*,*,#5946,.F.);
#8520=ORIENTED_EDGE('',*,*,#5936,.F.);
#8521=ORIENTED_EDGE('',*,*,#5940,.F.);
#8522=ORIENTED_EDGE('',*,*,#5943,.F.);
#8523=ORIENTED_EDGE('',*,*,#5926,.T.);
#8524=ORIENTED_EDGE('',*,*,#5930,.T.);
#8525=ORIENTED_EDGE('',*,*,#5933,.T.);
#8526=ORIENTED_EDGE('',*,*,#5935,.T.);
#8527=ORIENTED_EDGE('',*,*,#5923,.T.);
#8528=ORIENTED_EDGE('',*,*,#5920,.T.);
#8529=ORIENTED_EDGE('',*,*,#5917,.T.);
#8530=ORIENTED_EDGE('',*,*,#5914,.T.);
#8531=ORIENTED_EDGE('',*,*,#5948,.F.);
#8532=ORIENTED_EDGE('',*,*,#5949,.T.);
#8533=ORIENTED_EDGE('',*,*,#5950,.T.);
#8534=ORIENTED_EDGE('',*,*,#5949,.F.);
#8535=ORIENTED_EDGE('',*,*,#5951,.F.);
#8536=ORIENTED_EDGE('',*,*,#5952,.T.);
#8537=ORIENTED_EDGE('',*,*,#5953,.T.);
#8538=ORIENTED_EDGE('',*,*,#5952,.F.);
#8539=ORIENTED_EDGE('',*,*,#5951,.T.);
#8540=ORIENTED_EDGE('',*,*,#5948,.T.);
#8541=ORIENTED_EDGE('',*,*,#5953,.F.);
#8542=ORIENTED_EDGE('',*,*,#5950,.F.);
#8543=ORIENTED_EDGE('',*,*,#5954,.F.);
#8544=ORIENTED_EDGE('',*,*,#5955,.T.);
#8545=ORIENTED_EDGE('',*,*,#5956,.F.);
#8546=ORIENTED_EDGE('',*,*,#5955,.F.);
#8547=ORIENTED_EDGE('',*,*,#5957,.F.);
#8548=ORIENTED_EDGE('',*,*,#5958,.T.);
#8549=ORIENTED_EDGE('',*,*,#5959,.F.);
#8550=ORIENTED_EDGE('',*,*,#5958,.F.);
#8551=ORIENTED_EDGE('',*,*,#5960,.F.);
#8552=ORIENTED_EDGE('',*,*,#5961,.T.);
#8553=ORIENTED_EDGE('',*,*,#5962,.F.);
#8554=ORIENTED_EDGE('',*,*,#5961,.F.);
#8555=ORIENTED_EDGE('',*,*,#5963,.F.);
#8556=ORIENTED_EDGE('',*,*,#5964,.T.);
#8557=ORIENTED_EDGE('',*,*,#5965,.F.);
#8558=ORIENTED_EDGE('',*,*,#5964,.F.);
#8559=ORIENTED_EDGE('',*,*,#5966,.F.);
#8560=ORIENTED_EDGE('',*,*,#5967,.T.);
#8561=ORIENTED_EDGE('',*,*,#5968,.F.);
#8562=ORIENTED_EDGE('',*,*,#5967,.F.);
#8563=ORIENTED_EDGE('',*,*,#5969,.F.);
#8564=ORIENTED_EDGE('',*,*,#5970,.T.);
#8565=ORIENTED_EDGE('',*,*,#5971,.F.);
#8566=ORIENTED_EDGE('',*,*,#5970,.F.);
#8567=ORIENTED_EDGE('',*,*,#5972,.F.);
#8568=ORIENTED_EDGE('',*,*,#5973,.T.);
#8569=ORIENTED_EDGE('',*,*,#5974,.F.);
#8570=ORIENTED_EDGE('',*,*,#5973,.F.);
#8571=ORIENTED_EDGE('',*,*,#5975,.F.);
#8572=ORIENTED_EDGE('',*,*,#5976,.T.);
#8573=ORIENTED_EDGE('',*,*,#5977,.F.);
#8574=ORIENTED_EDGE('',*,*,#5976,.F.);
#8575=ORIENTED_EDGE('',*,*,#5978,.F.);
#8576=ORIENTED_EDGE('',*,*,#5979,.T.);
#8577=ORIENTED_EDGE('',*,*,#5980,.F.);
#8578=ORIENTED_EDGE('',*,*,#5979,.F.);
#8579=ORIENTED_EDGE('',*,*,#5981,.F.);
#8580=ORIENTED_EDGE('',*,*,#5982,.T.);
#8581=ORIENTED_EDGE('',*,*,#5983,.F.);
#8582=ORIENTED_EDGE('',*,*,#5982,.F.);
#8583=ORIENTED_EDGE('',*,*,#5984,.F.);
#8584=ORIENTED_EDGE('',*,*,#5985,.T.);
#8585=ORIENTED_EDGE('',*,*,#5986,.F.);
#8586=ORIENTED_EDGE('',*,*,#5985,.F.);
#8587=ORIENTED_EDGE('',*,*,#5987,.F.);
#8588=ORIENTED_EDGE('',*,*,#5988,.T.);
#8589=ORIENTED_EDGE('',*,*,#5989,.F.);
#8590=ORIENTED_EDGE('',*,*,#5988,.F.);
#8591=ORIENTED_EDGE('',*,*,#5990,.F.);
#8592=ORIENTED_EDGE('',*,*,#5991,.T.);
#8593=ORIENTED_EDGE('',*,*,#5992,.F.);
#8594=ORIENTED_EDGE('',*,*,#5991,.F.);
#8595=ORIENTED_EDGE('',*,*,#5993,.F.);
#8596=ORIENTED_EDGE('',*,*,#5994,.T.);
#8597=ORIENTED_EDGE('',*,*,#5995,.F.);
#8598=ORIENTED_EDGE('',*,*,#5994,.F.);
#8599=ORIENTED_EDGE('',*,*,#5996,.F.);
#8600=ORIENTED_EDGE('',*,*,#5997,.T.);
#8601=ORIENTED_EDGE('',*,*,#5998,.F.);
#8602=ORIENTED_EDGE('',*,*,#5997,.F.);
#8603=ORIENTED_EDGE('',*,*,#5999,.F.);
#8604=ORIENTED_EDGE('',*,*,#6000,.T.);
#8605=ORIENTED_EDGE('',*,*,#6001,.F.);
#8606=ORIENTED_EDGE('',*,*,#6000,.F.);
#8607=ORIENTED_EDGE('',*,*,#6002,.F.);
#8608=ORIENTED_EDGE('',*,*,#6003,.T.);
#8609=ORIENTED_EDGE('',*,*,#6004,.F.);
#8610=ORIENTED_EDGE('',*,*,#6003,.F.);
#8611=ORIENTED_EDGE('',*,*,#6005,.F.);
#8612=ORIENTED_EDGE('',*,*,#6006,.T.);
#8613=ORIENTED_EDGE('',*,*,#6007,.F.);
#8614=ORIENTED_EDGE('',*,*,#6006,.F.);
#8615=ORIENTED_EDGE('',*,*,#6008,.T.);
#8616=ORIENTED_EDGE('',*,*,#6009,.T.);
#8617=ORIENTED_EDGE('',*,*,#6010,.F.);
#8618=ORIENTED_EDGE('',*,*,#6011,.F.);
#8619=ORIENTED_EDGE('',*,*,#6012,.T.);
#8620=ORIENTED_EDGE('',*,*,#6011,.T.);
#8621=ORIENTED_EDGE('',*,*,#6013,.F.);
#8622=ORIENTED_EDGE('',*,*,#6014,.F.);
#8623=ORIENTED_EDGE('',*,*,#6015,.T.);
#8624=ORIENTED_EDGE('',*,*,#6014,.T.);
#8625=ORIENTED_EDGE('',*,*,#6016,.F.);
#8626=ORIENTED_EDGE('',*,*,#6017,.F.);
#8627=ORIENTED_EDGE('',*,*,#6018,.T.);
#8628=ORIENTED_EDGE('',*,*,#6017,.T.);
#8629=ORIENTED_EDGE('',*,*,#6019,.F.);
#8630=ORIENTED_EDGE('',*,*,#6009,.F.);
#8631=ORIENTED_EDGE('',*,*,#6019,.T.);
#8632=ORIENTED_EDGE('',*,*,#6016,.T.);
#8633=ORIENTED_EDGE('',*,*,#6013,.T.);
#8634=ORIENTED_EDGE('',*,*,#6010,.T.);
#8635=ORIENTED_EDGE('',*,*,#6005,.T.);
#8636=ORIENTED_EDGE('',*,*,#6002,.T.);
#8637=ORIENTED_EDGE('',*,*,#5999,.T.);
#8638=ORIENTED_EDGE('',*,*,#5996,.T.);
#8639=ORIENTED_EDGE('',*,*,#5993,.T.);
#8640=ORIENTED_EDGE('',*,*,#5990,.T.);
#8641=ORIENTED_EDGE('',*,*,#5987,.T.);
#8642=ORIENTED_EDGE('',*,*,#5984,.T.);
#8643=ORIENTED_EDGE('',*,*,#5981,.T.);
#8644=ORIENTED_EDGE('',*,*,#5978,.T.);
#8645=ORIENTED_EDGE('',*,*,#5975,.T.);
#8646=ORIENTED_EDGE('',*,*,#5972,.T.);
#8647=ORIENTED_EDGE('',*,*,#5969,.T.);
#8648=ORIENTED_EDGE('',*,*,#5966,.T.);
#8649=ORIENTED_EDGE('',*,*,#5963,.T.);
#8650=ORIENTED_EDGE('',*,*,#5960,.T.);
#8651=ORIENTED_EDGE('',*,*,#5957,.T.);
#8652=ORIENTED_EDGE('',*,*,#5954,.T.);
#8653=ORIENTED_EDGE('',*,*,#6018,.F.);
#8654=ORIENTED_EDGE('',*,*,#6008,.F.);
#8655=ORIENTED_EDGE('',*,*,#6012,.F.);
#8656=ORIENTED_EDGE('',*,*,#6015,.F.);
#8657=ORIENTED_EDGE('',*,*,#6007,.T.);
#8658=ORIENTED_EDGE('',*,*,#6004,.T.);
#8659=ORIENTED_EDGE('',*,*,#6001,.T.);
#8660=ORIENTED_EDGE('',*,*,#5998,.T.);
#8661=ORIENTED_EDGE('',*,*,#5995,.T.);
#8662=ORIENTED_EDGE('',*,*,#5992,.T.);
#8663=ORIENTED_EDGE('',*,*,#5989,.T.);
#8664=ORIENTED_EDGE('',*,*,#5986,.T.);
#8665=ORIENTED_EDGE('',*,*,#5983,.T.);
#8666=ORIENTED_EDGE('',*,*,#5980,.T.);
#8667=ORIENTED_EDGE('',*,*,#5977,.T.);
#8668=ORIENTED_EDGE('',*,*,#5974,.T.);
#8669=ORIENTED_EDGE('',*,*,#5971,.T.);
#8670=ORIENTED_EDGE('',*,*,#5968,.T.);
#8671=ORIENTED_EDGE('',*,*,#5965,.T.);
#8672=ORIENTED_EDGE('',*,*,#5962,.T.);
#8673=ORIENTED_EDGE('',*,*,#5959,.T.);
#8674=ORIENTED_EDGE('',*,*,#5956,.T.);
#8675=ORIENTED_EDGE('',*,*,#6020,.F.);
#8676=ORIENTED_EDGE('',*,*,#6021,.T.);
#8677=ORIENTED_EDGE('',*,*,#6022,.F.);
#8678=ORIENTED_EDGE('',*,*,#6021,.F.);
#8679=ORIENTED_EDGE('',*,*,#6023,.F.);
#8680=ORIENTED_EDGE('',*,*,#6024,.T.);
#8681=ORIENTED_EDGE('',*,*,#6025,.F.);
#8682=ORIENTED_EDGE('',*,*,#6024,.F.);
#8683=ORIENTED_EDGE('',*,*,#6026,.F.);
#8684=ORIENTED_EDGE('',*,*,#6027,.T.);
#8685=ORIENTED_EDGE('',*,*,#6028,.F.);
#8686=ORIENTED_EDGE('',*,*,#6027,.F.);
#8687=ORIENTED_EDGE('',*,*,#6029,.F.);
#8688=ORIENTED_EDGE('',*,*,#6030,.T.);
#8689=ORIENTED_EDGE('',*,*,#6031,.F.);
#8690=ORIENTED_EDGE('',*,*,#6030,.F.);
#8691=ORIENTED_EDGE('',*,*,#6032,.F.);
#8692=ORIENTED_EDGE('',*,*,#6033,.T.);
#8693=ORIENTED_EDGE('',*,*,#6034,.F.);
#8694=ORIENTED_EDGE('',*,*,#6033,.F.);
#8695=ORIENTED_EDGE('',*,*,#6035,.F.);
#8696=ORIENTED_EDGE('',*,*,#6036,.T.);
#8697=ORIENTED_EDGE('',*,*,#6037,.F.);
#8698=ORIENTED_EDGE('',*,*,#6036,.F.);
#8699=ORIENTED_EDGE('',*,*,#6038,.F.);
#8700=ORIENTED_EDGE('',*,*,#6039,.T.);
#8701=ORIENTED_EDGE('',*,*,#6040,.F.);
#8702=ORIENTED_EDGE('',*,*,#6039,.F.);
#8703=ORIENTED_EDGE('',*,*,#6041,.T.);
#8704=ORIENTED_EDGE('',*,*,#6042,.T.);
#8705=ORIENTED_EDGE('',*,*,#6043,.F.);
#8706=ORIENTED_EDGE('',*,*,#6044,.F.);
#8707=ORIENTED_EDGE('',*,*,#6045,.T.);
#8708=ORIENTED_EDGE('',*,*,#6044,.T.);
#8709=ORIENTED_EDGE('',*,*,#6046,.F.);
#8710=ORIENTED_EDGE('',*,*,#6047,.F.);
#8711=ORIENTED_EDGE('',*,*,#6048,.T.);
#8712=ORIENTED_EDGE('',*,*,#6047,.T.);
#8713=ORIENTED_EDGE('',*,*,#6049,.F.);
#8714=ORIENTED_EDGE('',*,*,#6050,.F.);
#8715=ORIENTED_EDGE('',*,*,#6051,.T.);
#8716=ORIENTED_EDGE('',*,*,#6050,.T.);
#8717=ORIENTED_EDGE('',*,*,#6052,.F.);
#8718=ORIENTED_EDGE('',*,*,#6042,.F.);
#8719=ORIENTED_EDGE('',*,*,#6052,.T.);
#8720=ORIENTED_EDGE('',*,*,#6049,.T.);
#8721=ORIENTED_EDGE('',*,*,#6046,.T.);
#8722=ORIENTED_EDGE('',*,*,#6043,.T.);
#8723=ORIENTED_EDGE('',*,*,#6020,.T.);
#8724=ORIENTED_EDGE('',*,*,#6023,.T.);
#8725=ORIENTED_EDGE('',*,*,#6026,.T.);
#8726=ORIENTED_EDGE('',*,*,#6029,.T.);
#8727=ORIENTED_EDGE('',*,*,#6032,.T.);
#8728=ORIENTED_EDGE('',*,*,#6035,.T.);
#8729=ORIENTED_EDGE('',*,*,#6038,.T.);
#8730=ORIENTED_EDGE('',*,*,#6051,.F.);
#8731=ORIENTED_EDGE('',*,*,#6041,.F.);
#8732=ORIENTED_EDGE('',*,*,#6045,.F.);
#8733=ORIENTED_EDGE('',*,*,#6048,.F.);
#8734=ORIENTED_EDGE('',*,*,#6022,.T.);
#8735=ORIENTED_EDGE('',*,*,#6025,.T.);
#8736=ORIENTED_EDGE('',*,*,#6028,.T.);
#8737=ORIENTED_EDGE('',*,*,#6031,.T.);
#8738=ORIENTED_EDGE('',*,*,#6034,.T.);
#8739=ORIENTED_EDGE('',*,*,#6037,.T.);
#8740=ORIENTED_EDGE('',*,*,#6040,.T.);
#8741=ORIENTED_EDGE('',*,*,#6053,.F.);
#8742=ORIENTED_EDGE('',*,*,#6054,.T.);
#8743=ORIENTED_EDGE('',*,*,#6055,.T.);
#8744=ORIENTED_EDGE('',*,*,#6056,.T.);
#8745=ORIENTED_EDGE('',*,*,#6057,.F.);
#8746=ORIENTED_EDGE('',*,*,#6058,.T.);
#8747=ORIENTED_EDGE('',*,*,#6053,.T.);
#8748=ORIENTED_EDGE('',*,*,#6059,.T.);
#8749=ORIENTED_EDGE('',*,*,#6060,.F.);
#8750=ORIENTED_EDGE('',*,*,#6061,.T.);
#8751=ORIENTED_EDGE('',*,*,#6057,.T.);
#8752=ORIENTED_EDGE('',*,*,#6062,.T.);
#8753=ORIENTED_EDGE('',*,*,#6063,.F.);
#8754=ORIENTED_EDGE('',*,*,#6064,.T.);
#8755=ORIENTED_EDGE('',*,*,#6060,.T.);
#8756=ORIENTED_EDGE('',*,*,#6065,.T.);
#8757=ORIENTED_EDGE('',*,*,#6066,.F.);
#8758=ORIENTED_EDGE('',*,*,#6067,.T.);
#8759=ORIENTED_EDGE('',*,*,#6063,.T.);
#8760=ORIENTED_EDGE('',*,*,#6068,.T.);
#8761=ORIENTED_EDGE('',*,*,#6069,.F.);
#8762=ORIENTED_EDGE('',*,*,#6070,.T.);
#8763=ORIENTED_EDGE('',*,*,#6066,.T.);
#8764=ORIENTED_EDGE('',*,*,#6071,.T.);
#8765=ORIENTED_EDGE('',*,*,#6072,.F.);
#8766=ORIENTED_EDGE('',*,*,#6073,.T.);
#8767=ORIENTED_EDGE('',*,*,#6069,.T.);
#8768=ORIENTED_EDGE('',*,*,#6074,.T.);
#8769=ORIENTED_EDGE('',*,*,#6075,.F.);
#8770=ORIENTED_EDGE('',*,*,#6076,.T.);
#8771=ORIENTED_EDGE('',*,*,#6072,.T.);
#8772=ORIENTED_EDGE('',*,*,#6077,.T.);
#8773=ORIENTED_EDGE('',*,*,#6078,.F.);
#8774=ORIENTED_EDGE('',*,*,#6079,.T.);
#8775=ORIENTED_EDGE('',*,*,#6075,.T.);
#8776=ORIENTED_EDGE('',*,*,#6080,.T.);
#8777=ORIENTED_EDGE('',*,*,#6081,.F.);
#8778=ORIENTED_EDGE('',*,*,#6082,.T.);
#8779=ORIENTED_EDGE('',*,*,#6078,.T.);
#8780=ORIENTED_EDGE('',*,*,#6083,.T.);
#8781=ORIENTED_EDGE('',*,*,#6084,.F.);
#8782=ORIENTED_EDGE('',*,*,#6085,.T.);
#8783=ORIENTED_EDGE('',*,*,#6081,.T.);
#8784=ORIENTED_EDGE('',*,*,#6086,.T.);
#8785=ORIENTED_EDGE('',*,*,#6087,.F.);
#8786=ORIENTED_EDGE('',*,*,#6088,.T.);
#8787=ORIENTED_EDGE('',*,*,#6084,.T.);
#8788=ORIENTED_EDGE('',*,*,#6089,.T.);
#8789=ORIENTED_EDGE('',*,*,#6090,.F.);
#8790=ORIENTED_EDGE('',*,*,#6091,.T.);
#8791=ORIENTED_EDGE('',*,*,#6087,.T.);
#8792=ORIENTED_EDGE('',*,*,#6092,.T.);
#8793=ORIENTED_EDGE('',*,*,#6093,.F.);
#8794=ORIENTED_EDGE('',*,*,#6094,.T.);
#8795=ORIENTED_EDGE('',*,*,#6090,.T.);
#8796=ORIENTED_EDGE('',*,*,#6095,.T.);
#8797=ORIENTED_EDGE('',*,*,#6096,.F.);
#8798=ORIENTED_EDGE('',*,*,#6097,.T.);
#8799=ORIENTED_EDGE('',*,*,#6093,.T.);
#8800=ORIENTED_EDGE('',*,*,#6098,.T.);
#8801=ORIENTED_EDGE('',*,*,#6099,.F.);
#8802=ORIENTED_EDGE('',*,*,#6100,.T.);
#8803=ORIENTED_EDGE('',*,*,#6096,.T.);
#8804=ORIENTED_EDGE('',*,*,#6101,.T.);
#8805=ORIENTED_EDGE('',*,*,#6102,.F.);
#8806=ORIENTED_EDGE('',*,*,#6103,.T.);
#8807=ORIENTED_EDGE('',*,*,#6104,.T.);
#8808=ORIENTED_EDGE('',*,*,#6105,.F.);
#8809=ORIENTED_EDGE('',*,*,#6106,.F.);
#8810=ORIENTED_EDGE('',*,*,#6107,.T.);
#8811=ORIENTED_EDGE('',*,*,#6102,.T.);
#8812=ORIENTED_EDGE('',*,*,#6108,.F.);
#8813=ORIENTED_EDGE('',*,*,#6109,.F.);
#8814=ORIENTED_EDGE('',*,*,#6110,.T.);
#8815=ORIENTED_EDGE('',*,*,#6106,.T.);
#8816=ORIENTED_EDGE('',*,*,#6111,.F.);
#8817=ORIENTED_EDGE('',*,*,#6112,.F.);
#8818=ORIENTED_EDGE('',*,*,#6113,.T.);
#8819=ORIENTED_EDGE('',*,*,#6109,.T.);
#8820=ORIENTED_EDGE('',*,*,#6114,.F.);
#8821=ORIENTED_EDGE('',*,*,#6115,.F.);
#8822=ORIENTED_EDGE('',*,*,#6116,.T.);
#8823=ORIENTED_EDGE('',*,*,#6112,.T.);
#8824=ORIENTED_EDGE('',*,*,#6117,.F.);
#8825=ORIENTED_EDGE('',*,*,#6118,.F.);
#8826=ORIENTED_EDGE('',*,*,#6119,.T.);
#8827=ORIENTED_EDGE('',*,*,#6115,.T.);
#8828=ORIENTED_EDGE('',*,*,#6120,.F.);
#8829=ORIENTED_EDGE('',*,*,#6121,.F.);
#8830=ORIENTED_EDGE('',*,*,#6122,.T.);
#8831=ORIENTED_EDGE('',*,*,#6118,.T.);
#8832=ORIENTED_EDGE('',*,*,#6123,.F.);
#8833=ORIENTED_EDGE('',*,*,#6124,.F.);
#8834=ORIENTED_EDGE('',*,*,#6125,.T.);
#8835=ORIENTED_EDGE('',*,*,#6121,.T.);
#8836=ORIENTED_EDGE('',*,*,#6126,.F.);
#8837=ORIENTED_EDGE('',*,*,#6127,.F.);
#8838=ORIENTED_EDGE('',*,*,#6128,.T.);
#8839=ORIENTED_EDGE('',*,*,#6124,.T.);
#8840=ORIENTED_EDGE('',*,*,#6129,.F.);
#8841=ORIENTED_EDGE('',*,*,#6130,.F.);
#8842=ORIENTED_EDGE('',*,*,#6131,.T.);
#8843=ORIENTED_EDGE('',*,*,#6127,.T.);
#8844=ORIENTED_EDGE('',*,*,#6132,.F.);
#8845=ORIENTED_EDGE('',*,*,#6133,.F.);
#8846=ORIENTED_EDGE('',*,*,#6134,.T.);
#8847=ORIENTED_EDGE('',*,*,#6130,.T.);
#8848=ORIENTED_EDGE('',*,*,#6135,.F.);
#8849=ORIENTED_EDGE('',*,*,#6136,.F.);
#8850=ORIENTED_EDGE('',*,*,#6137,.T.);
#8851=ORIENTED_EDGE('',*,*,#6133,.T.);
#8852=ORIENTED_EDGE('',*,*,#6138,.F.);
#8853=ORIENTED_EDGE('',*,*,#6139,.F.);
#8854=ORIENTED_EDGE('',*,*,#6140,.T.);
#8855=ORIENTED_EDGE('',*,*,#6136,.T.);
#8856=ORIENTED_EDGE('',*,*,#6141,.F.);
#8857=ORIENTED_EDGE('',*,*,#6142,.F.);
#8858=ORIENTED_EDGE('',*,*,#6143,.T.);
#8859=ORIENTED_EDGE('',*,*,#6139,.T.);
#8860=ORIENTED_EDGE('',*,*,#6144,.F.);
#8861=ORIENTED_EDGE('',*,*,#6145,.F.);
#8862=ORIENTED_EDGE('',*,*,#6146,.T.);
#8863=ORIENTED_EDGE('',*,*,#6142,.T.);
#8864=ORIENTED_EDGE('',*,*,#6147,.F.);
#8865=ORIENTED_EDGE('',*,*,#6148,.F.);
#8866=ORIENTED_EDGE('',*,*,#6149,.T.);
#8867=ORIENTED_EDGE('',*,*,#6145,.T.);
#8868=ORIENTED_EDGE('',*,*,#6150,.F.);
#8869=ORIENTED_EDGE('',*,*,#6151,.F.);
#8870=ORIENTED_EDGE('',*,*,#6104,.F.);
#8871=ORIENTED_EDGE('',*,*,#6152,.F.);
#8872=ORIENTED_EDGE('',*,*,#6153,.F.);
#8873=ORIENTED_EDGE('',*,*,#6154,.F.);
#8874=ORIENTED_EDGE('',*,*,#6155,.T.);
#8875=ORIENTED_EDGE('',*,*,#6156,.F.);
#8876=ORIENTED_EDGE('',*,*,#6155,.F.);
#8877=ORIENTED_EDGE('',*,*,#6152,.T.);
#8878=ORIENTED_EDGE('',*,*,#6103,.F.);
#8879=ORIENTED_EDGE('',*,*,#6107,.F.);
#8880=ORIENTED_EDGE('',*,*,#6110,.F.);
#8881=ORIENTED_EDGE('',*,*,#6113,.F.);
#8882=ORIENTED_EDGE('',*,*,#6116,.F.);
#8883=ORIENTED_EDGE('',*,*,#6119,.F.);
#8884=ORIENTED_EDGE('',*,*,#6122,.F.);
#8885=ORIENTED_EDGE('',*,*,#6125,.F.);
#8886=ORIENTED_EDGE('',*,*,#6128,.F.);
#8887=ORIENTED_EDGE('',*,*,#6131,.F.);
#8888=ORIENTED_EDGE('',*,*,#6134,.F.);
#8889=ORIENTED_EDGE('',*,*,#6137,.F.);
#8890=ORIENTED_EDGE('',*,*,#6140,.F.);
#8891=ORIENTED_EDGE('',*,*,#6143,.F.);
#8892=ORIENTED_EDGE('',*,*,#6146,.F.);
#8893=ORIENTED_EDGE('',*,*,#6149,.F.);
#8894=ORIENTED_EDGE('',*,*,#6157,.F.);
#8895=ORIENTED_EDGE('',*,*,#6158,.F.);
#8896=ORIENTED_EDGE('',*,*,#6054,.F.);
#8897=ORIENTED_EDGE('',*,*,#6058,.F.);
#8898=ORIENTED_EDGE('',*,*,#6061,.F.);
#8899=ORIENTED_EDGE('',*,*,#6064,.F.);
#8900=ORIENTED_EDGE('',*,*,#6067,.F.);
#8901=ORIENTED_EDGE('',*,*,#6070,.F.);
#8902=ORIENTED_EDGE('',*,*,#6073,.F.);
#8903=ORIENTED_EDGE('',*,*,#6076,.F.);
#8904=ORIENTED_EDGE('',*,*,#6079,.F.);
#8905=ORIENTED_EDGE('',*,*,#6082,.F.);
#8906=ORIENTED_EDGE('',*,*,#6085,.F.);
#8907=ORIENTED_EDGE('',*,*,#6088,.F.);
#8908=ORIENTED_EDGE('',*,*,#6091,.F.);
#8909=ORIENTED_EDGE('',*,*,#6094,.F.);
#8910=ORIENTED_EDGE('',*,*,#6097,.F.);
#8911=ORIENTED_EDGE('',*,*,#6100,.F.);
#8912=ORIENTED_EDGE('',*,*,#6159,.F.);
#8913=ORIENTED_EDGE('',*,*,#6148,.T.);
#8914=ORIENTED_EDGE('',*,*,#6160,.F.);
#8915=ORIENTED_EDGE('',*,*,#6161,.F.);
#8916=ORIENTED_EDGE('',*,*,#6157,.T.);
#8917=ORIENTED_EDGE('',*,*,#6151,.T.);
#8918=ORIENTED_EDGE('',*,*,#6154,.T.);
#8919=ORIENTED_EDGE('',*,*,#6162,.F.);
#8920=ORIENTED_EDGE('',*,*,#6101,.F.);
#8921=ORIENTED_EDGE('',*,*,#6098,.F.);
#8922=ORIENTED_EDGE('',*,*,#6095,.F.);
#8923=ORIENTED_EDGE('',*,*,#6092,.F.);
#8924=ORIENTED_EDGE('',*,*,#6089,.F.);
#8925=ORIENTED_EDGE('',*,*,#6086,.F.);
#8926=ORIENTED_EDGE('',*,*,#6083,.F.);
#8927=ORIENTED_EDGE('',*,*,#6080,.F.);
#8928=ORIENTED_EDGE('',*,*,#6077,.F.);
#8929=ORIENTED_EDGE('',*,*,#6074,.F.);
#8930=ORIENTED_EDGE('',*,*,#6071,.F.);
#8931=ORIENTED_EDGE('',*,*,#6068,.F.);
#8932=ORIENTED_EDGE('',*,*,#6065,.F.);
#8933=ORIENTED_EDGE('',*,*,#6062,.F.);
#8934=ORIENTED_EDGE('',*,*,#6059,.F.);
#8935=ORIENTED_EDGE('',*,*,#6056,.F.);
#8936=ORIENTED_EDGE('',*,*,#6163,.F.);
#8937=ORIENTED_EDGE('',*,*,#6160,.T.);
#8938=ORIENTED_EDGE('',*,*,#6150,.T.);
#8939=ORIENTED_EDGE('',*,*,#6147,.T.);
#8940=ORIENTED_EDGE('',*,*,#6144,.T.);
#8941=ORIENTED_EDGE('',*,*,#6141,.T.);
#8942=ORIENTED_EDGE('',*,*,#6138,.T.);
#8943=ORIENTED_EDGE('',*,*,#6135,.T.);
#8944=ORIENTED_EDGE('',*,*,#6132,.T.);
#8945=ORIENTED_EDGE('',*,*,#6129,.T.);
#8946=ORIENTED_EDGE('',*,*,#6126,.T.);
#8947=ORIENTED_EDGE('',*,*,#6123,.T.);
#8948=ORIENTED_EDGE('',*,*,#6120,.T.);
#8949=ORIENTED_EDGE('',*,*,#6117,.T.);
#8950=ORIENTED_EDGE('',*,*,#6114,.T.);
#8951=ORIENTED_EDGE('',*,*,#6111,.T.);
#8952=ORIENTED_EDGE('',*,*,#6108,.T.);
#8953=ORIENTED_EDGE('',*,*,#6105,.T.);
#8954=ORIENTED_EDGE('',*,*,#6099,.T.);
#8955=ORIENTED_EDGE('',*,*,#6162,.T.);
#8956=ORIENTED_EDGE('',*,*,#6153,.T.);
#8957=ORIENTED_EDGE('',*,*,#6159,.T.);
#8958=ORIENTED_EDGE('',*,*,#6164,.F.);
#8959=ORIENTED_EDGE('',*,*,#6165,.T.);
#8960=ORIENTED_EDGE('',*,*,#6166,.T.);
#8961=ORIENTED_EDGE('',*,*,#6167,.F.);
#8962=ORIENTED_EDGE('',*,*,#6168,.F.);
#8963=ORIENTED_EDGE('',*,*,#6169,.T.);
#8964=ORIENTED_EDGE('',*,*,#6170,.T.);
#8965=ORIENTED_EDGE('',*,*,#6165,.F.);
#8966=ORIENTED_EDGE('',*,*,#6171,.F.);
#8967=ORIENTED_EDGE('',*,*,#6172,.T.);
#8968=ORIENTED_EDGE('',*,*,#6173,.T.);
#8969=ORIENTED_EDGE('',*,*,#6169,.F.);
#8970=ORIENTED_EDGE('',*,*,#6174,.F.);
#8971=ORIENTED_EDGE('',*,*,#6175,.T.);
#8972=ORIENTED_EDGE('',*,*,#6176,.T.);
#8973=ORIENTED_EDGE('',*,*,#6172,.F.);
#8974=ORIENTED_EDGE('',*,*,#6177,.F.);
#8975=ORIENTED_EDGE('',*,*,#6178,.T.);
#8976=ORIENTED_EDGE('',*,*,#6179,.T.);
#8977=ORIENTED_EDGE('',*,*,#6175,.F.);
#8978=ORIENTED_EDGE('',*,*,#6180,.F.);
#8979=ORIENTED_EDGE('',*,*,#6167,.T.);
#8980=ORIENTED_EDGE('',*,*,#6181,.T.);
#8981=ORIENTED_EDGE('',*,*,#6178,.F.);
#8982=ORIENTED_EDGE('',*,*,#6181,.F.);
#8983=ORIENTED_EDGE('',*,*,#6166,.F.);
#8984=ORIENTED_EDGE('',*,*,#6170,.F.);
#8985=ORIENTED_EDGE('',*,*,#6173,.F.);
#8986=ORIENTED_EDGE('',*,*,#6176,.F.);
#8987=ORIENTED_EDGE('',*,*,#6179,.F.);
#8988=ORIENTED_EDGE('',*,*,#6182,.T.);
#8989=ORIENTED_EDGE('',*,*,#6158,.T.);
#8990=ORIENTED_EDGE('',*,*,#6161,.T.);
#8991=ORIENTED_EDGE('',*,*,#6163,.T.);
#8992=ORIENTED_EDGE('',*,*,#6055,.F.);
#8993=ORIENTED_EDGE('',*,*,#6182,.F.);
#8994=ORIENTED_EDGE('',*,*,#6183,.T.);
#8995=ORIENTED_EDGE('',*,*,#6184,.T.);
#8996=ORIENTED_EDGE('',*,*,#6183,.F.);
#8997=ORIENTED_EDGE('',*,*,#6184,.F.);
#8998=ORIENTED_EDGE('',*,*,#6164,.T.);
#8999=ORIENTED_EDGE('',*,*,#6180,.T.);
#9000=ORIENTED_EDGE('',*,*,#6177,.T.);
#9001=ORIENTED_EDGE('',*,*,#6174,.T.);
#9002=ORIENTED_EDGE('',*,*,#6171,.T.);
#9003=ORIENTED_EDGE('',*,*,#6168,.T.);
#9004=ORIENTED_EDGE('',*,*,#6156,.T.);
#9005=ORIENTED_EDGE('',*,*,#6185,.F.);
#9006=ORIENTED_EDGE('',*,*,#6186,.T.);
#9007=ORIENTED_EDGE('',*,*,#6187,.T.);
#9008=ORIENTED_EDGE('',*,*,#6188,.T.);
#9009=ORIENTED_EDGE('',*,*,#6189,.F.);
#9010=ORIENTED_EDGE('',*,*,#6190,.T.);
#9011=ORIENTED_EDGE('',*,*,#6185,.T.);
#9012=ORIENTED_EDGE('',*,*,#6191,.T.);
#9013=ORIENTED_EDGE('',*,*,#6192,.F.);
#9014=ORIENTED_EDGE('',*,*,#6193,.T.);
#9015=ORIENTED_EDGE('',*,*,#6189,.T.);
#9016=ORIENTED_EDGE('',*,*,#6194,.T.);
#9017=ORIENTED_EDGE('',*,*,#6195,.F.);
#9018=ORIENTED_EDGE('',*,*,#6196,.T.);
#9019=ORIENTED_EDGE('',*,*,#6192,.T.);
#9020=ORIENTED_EDGE('',*,*,#6197,.T.);
#9021=ORIENTED_EDGE('',*,*,#6198,.F.);
#9022=ORIENTED_EDGE('',*,*,#6199,.T.);
#9023=ORIENTED_EDGE('',*,*,#6195,.T.);
#9024=ORIENTED_EDGE('',*,*,#6200,.T.);
#9025=ORIENTED_EDGE('',*,*,#6201,.F.);
#9026=ORIENTED_EDGE('',*,*,#6202,.T.);
#9027=ORIENTED_EDGE('',*,*,#6198,.T.);
#9028=ORIENTED_EDGE('',*,*,#6203,.T.);
#9029=ORIENTED_EDGE('',*,*,#6204,.F.);
#9030=ORIENTED_EDGE('',*,*,#6205,.T.);
#9031=ORIENTED_EDGE('',*,*,#6201,.T.);
#9032=ORIENTED_EDGE('',*,*,#6206,.T.);
#9033=ORIENTED_EDGE('',*,*,#6207,.F.);
#9034=ORIENTED_EDGE('',*,*,#6208,.T.);
#9035=ORIENTED_EDGE('',*,*,#6204,.T.);
#9036=ORIENTED_EDGE('',*,*,#6209,.T.);
#9037=ORIENTED_EDGE('',*,*,#6210,.F.);
#9038=ORIENTED_EDGE('',*,*,#6211,.T.);
#9039=ORIENTED_EDGE('',*,*,#6207,.T.);
#9040=ORIENTED_EDGE('',*,*,#6212,.T.);
#9041=ORIENTED_EDGE('',*,*,#6213,.F.);
#9042=ORIENTED_EDGE('',*,*,#6214,.T.);
#9043=ORIENTED_EDGE('',*,*,#6210,.T.);
#9044=ORIENTED_EDGE('',*,*,#6215,.T.);
#9045=ORIENTED_EDGE('',*,*,#6216,.F.);
#9046=ORIENTED_EDGE('',*,*,#6217,.T.);
#9047=ORIENTED_EDGE('',*,*,#6213,.T.);
#9048=ORIENTED_EDGE('',*,*,#6218,.T.);
#9049=ORIENTED_EDGE('',*,*,#6219,.F.);
#9050=ORIENTED_EDGE('',*,*,#6220,.T.);
#9051=ORIENTED_EDGE('',*,*,#6221,.T.);
#9052=ORIENTED_EDGE('',*,*,#6222,.F.);
#9053=ORIENTED_EDGE('',*,*,#6223,.F.);
#9054=ORIENTED_EDGE('',*,*,#6224,.T.);
#9055=ORIENTED_EDGE('',*,*,#6219,.T.);
#9056=ORIENTED_EDGE('',*,*,#6225,.F.);
#9057=ORIENTED_EDGE('',*,*,#6226,.F.);
#9058=ORIENTED_EDGE('',*,*,#6227,.T.);
#9059=ORIENTED_EDGE('',*,*,#6223,.T.);
#9060=ORIENTED_EDGE('',*,*,#6228,.F.);
#9061=ORIENTED_EDGE('',*,*,#6229,.F.);
#9062=ORIENTED_EDGE('',*,*,#6230,.T.);
#9063=ORIENTED_EDGE('',*,*,#6226,.T.);
#9064=ORIENTED_EDGE('',*,*,#6231,.F.);
#9065=ORIENTED_EDGE('',*,*,#6232,.F.);
#9066=ORIENTED_EDGE('',*,*,#6233,.T.);
#9067=ORIENTED_EDGE('',*,*,#6229,.T.);
#9068=ORIENTED_EDGE('',*,*,#6234,.F.);
#9069=ORIENTED_EDGE('',*,*,#6235,.F.);
#9070=ORIENTED_EDGE('',*,*,#6236,.T.);
#9071=ORIENTED_EDGE('',*,*,#6232,.T.);
#9072=ORIENTED_EDGE('',*,*,#6237,.F.);
#9073=ORIENTED_EDGE('',*,*,#6238,.F.);
#9074=ORIENTED_EDGE('',*,*,#6239,.T.);
#9075=ORIENTED_EDGE('',*,*,#6235,.T.);
#9076=ORIENTED_EDGE('',*,*,#6240,.F.);
#9077=ORIENTED_EDGE('',*,*,#6241,.F.);
#9078=ORIENTED_EDGE('',*,*,#6242,.T.);
#9079=ORIENTED_EDGE('',*,*,#6238,.T.);
#9080=ORIENTED_EDGE('',*,*,#6243,.F.);
#9081=ORIENTED_EDGE('',*,*,#6244,.F.);
#9082=ORIENTED_EDGE('',*,*,#6245,.T.);
#9083=ORIENTED_EDGE('',*,*,#6241,.T.);
#9084=ORIENTED_EDGE('',*,*,#6246,.F.);
#9085=ORIENTED_EDGE('',*,*,#6247,.F.);
#9086=ORIENTED_EDGE('',*,*,#6248,.T.);
#9087=ORIENTED_EDGE('',*,*,#6244,.T.);
#9088=ORIENTED_EDGE('',*,*,#6249,.F.);
#9089=ORIENTED_EDGE('',*,*,#6250,.F.);
#9090=ORIENTED_EDGE('',*,*,#6251,.T.);
#9091=ORIENTED_EDGE('',*,*,#6247,.T.);
#9092=ORIENTED_EDGE('',*,*,#6252,.F.);
#9093=ORIENTED_EDGE('',*,*,#6253,.F.);
#9094=ORIENTED_EDGE('',*,*,#6221,.F.);
#9095=ORIENTED_EDGE('',*,*,#6254,.F.);
#9096=ORIENTED_EDGE('',*,*,#6255,.F.);
#9097=ORIENTED_EDGE('',*,*,#6256,.F.);
#9098=ORIENTED_EDGE('',*,*,#6257,.T.);
#9099=ORIENTED_EDGE('',*,*,#6258,.F.);
#9100=ORIENTED_EDGE('',*,*,#6257,.F.);
#9101=ORIENTED_EDGE('',*,*,#6254,.T.);
#9102=ORIENTED_EDGE('',*,*,#6220,.F.);
#9103=ORIENTED_EDGE('',*,*,#6224,.F.);
#9104=ORIENTED_EDGE('',*,*,#6227,.F.);
#9105=ORIENTED_EDGE('',*,*,#6230,.F.);
#9106=ORIENTED_EDGE('',*,*,#6233,.F.);
#9107=ORIENTED_EDGE('',*,*,#6236,.F.);
#9108=ORIENTED_EDGE('',*,*,#6239,.F.);
#9109=ORIENTED_EDGE('',*,*,#6242,.F.);
#9110=ORIENTED_EDGE('',*,*,#6245,.F.);
#9111=ORIENTED_EDGE('',*,*,#6248,.F.);
#9112=ORIENTED_EDGE('',*,*,#6251,.F.);
#9113=ORIENTED_EDGE('',*,*,#6259,.F.);
#9114=ORIENTED_EDGE('',*,*,#6260,.F.);
#9115=ORIENTED_EDGE('',*,*,#6186,.F.);
#9116=ORIENTED_EDGE('',*,*,#6190,.F.);
#9117=ORIENTED_EDGE('',*,*,#6193,.F.);
#9118=ORIENTED_EDGE('',*,*,#6196,.F.);
#9119=ORIENTED_EDGE('',*,*,#6199,.F.);
#9120=ORIENTED_EDGE('',*,*,#6202,.F.);
#9121=ORIENTED_EDGE('',*,*,#6205,.F.);
#9122=ORIENTED_EDGE('',*,*,#6208,.F.);
#9123=ORIENTED_EDGE('',*,*,#6211,.F.);
#9124=ORIENTED_EDGE('',*,*,#6214,.F.);
#9125=ORIENTED_EDGE('',*,*,#6217,.F.);
#9126=ORIENTED_EDGE('',*,*,#6261,.F.);
#9127=ORIENTED_EDGE('',*,*,#6250,.T.);
#9128=ORIENTED_EDGE('',*,*,#6262,.F.);
#9129=ORIENTED_EDGE('',*,*,#6263,.F.);
#9130=ORIENTED_EDGE('',*,*,#6259,.T.);
#9131=ORIENTED_EDGE('',*,*,#6253,.T.);
#9132=ORIENTED_EDGE('',*,*,#6256,.T.);
#9133=ORIENTED_EDGE('',*,*,#6264,.F.);
#9134=ORIENTED_EDGE('',*,*,#6218,.F.);
#9135=ORIENTED_EDGE('',*,*,#6215,.F.);
#9136=ORIENTED_EDGE('',*,*,#6212,.F.);
#9137=ORIENTED_EDGE('',*,*,#6209,.F.);
#9138=ORIENTED_EDGE('',*,*,#6206,.F.);
#9139=ORIENTED_EDGE('',*,*,#6203,.F.);
#9140=ORIENTED_EDGE('',*,*,#6200,.F.);
#9141=ORIENTED_EDGE('',*,*,#6197,.F.);
#9142=ORIENTED_EDGE('',*,*,#6194,.F.);
#9143=ORIENTED_EDGE('',*,*,#6191,.F.);
#9144=ORIENTED_EDGE('',*,*,#6188,.F.);
#9145=ORIENTED_EDGE('',*,*,#6265,.F.);
#9146=ORIENTED_EDGE('',*,*,#6262,.T.);
#9147=ORIENTED_EDGE('',*,*,#6252,.T.);
#9148=ORIENTED_EDGE('',*,*,#6249,.T.);
#9149=ORIENTED_EDGE('',*,*,#6246,.T.);
#9150=ORIENTED_EDGE('',*,*,#6243,.T.);
#9151=ORIENTED_EDGE('',*,*,#6240,.T.);
#9152=ORIENTED_EDGE('',*,*,#6237,.T.);
#9153=ORIENTED_EDGE('',*,*,#6234,.T.);
#9154=ORIENTED_EDGE('',*,*,#6231,.T.);
#9155=ORIENTED_EDGE('',*,*,#6228,.T.);
#9156=ORIENTED_EDGE('',*,*,#6225,.T.);
#9157=ORIENTED_EDGE('',*,*,#6222,.T.);
#9158=ORIENTED_EDGE('',*,*,#6216,.T.);
#9159=ORIENTED_EDGE('',*,*,#6264,.T.);
#9160=ORIENTED_EDGE('',*,*,#6255,.T.);
#9161=ORIENTED_EDGE('',*,*,#6261,.T.);
#9162=ORIENTED_EDGE('',*,*,#6266,.F.);
#9163=ORIENTED_EDGE('',*,*,#6267,.T.);
#9164=ORIENTED_EDGE('',*,*,#6268,.T.);
#9165=ORIENTED_EDGE('',*,*,#6269,.F.);
#9166=ORIENTED_EDGE('',*,*,#6270,.F.);
#9167=ORIENTED_EDGE('',*,*,#6271,.T.);
#9168=ORIENTED_EDGE('',*,*,#6272,.T.);
#9169=ORIENTED_EDGE('',*,*,#6267,.F.);
#9170=ORIENTED_EDGE('',*,*,#6273,.F.);
#9171=ORIENTED_EDGE('',*,*,#6274,.T.);
#9172=ORIENTED_EDGE('',*,*,#6275,.T.);
#9173=ORIENTED_EDGE('',*,*,#6271,.F.);
#9174=ORIENTED_EDGE('',*,*,#6276,.F.);
#9175=ORIENTED_EDGE('',*,*,#6277,.T.);
#9176=ORIENTED_EDGE('',*,*,#6278,.T.);
#9177=ORIENTED_EDGE('',*,*,#6274,.F.);
#9178=ORIENTED_EDGE('',*,*,#6279,.F.);
#9179=ORIENTED_EDGE('',*,*,#6280,.T.);
#9180=ORIENTED_EDGE('',*,*,#6281,.T.);
#9181=ORIENTED_EDGE('',*,*,#6277,.F.);
#9182=ORIENTED_EDGE('',*,*,#6282,.F.);
#9183=ORIENTED_EDGE('',*,*,#6269,.T.);
#9184=ORIENTED_EDGE('',*,*,#6283,.T.);
#9185=ORIENTED_EDGE('',*,*,#6280,.F.);
#9186=ORIENTED_EDGE('',*,*,#6283,.F.);
#9187=ORIENTED_EDGE('',*,*,#6268,.F.);
#9188=ORIENTED_EDGE('',*,*,#6272,.F.);
#9189=ORIENTED_EDGE('',*,*,#6275,.F.);
#9190=ORIENTED_EDGE('',*,*,#6278,.F.);
#9191=ORIENTED_EDGE('',*,*,#6281,.F.);
#9192=ORIENTED_EDGE('',*,*,#6284,.T.);
#9193=ORIENTED_EDGE('',*,*,#6260,.T.);
#9194=ORIENTED_EDGE('',*,*,#6263,.T.);
#9195=ORIENTED_EDGE('',*,*,#6265,.T.);
#9196=ORIENTED_EDGE('',*,*,#6187,.F.);
#9197=ORIENTED_EDGE('',*,*,#6284,.F.);
#9198=ORIENTED_EDGE('',*,*,#6285,.T.);
#9199=ORIENTED_EDGE('',*,*,#6286,.T.);
#9200=ORIENTED_EDGE('',*,*,#6285,.F.);
#9201=ORIENTED_EDGE('',*,*,#6286,.F.);
#9202=ORIENTED_EDGE('',*,*,#6266,.T.);
#9203=ORIENTED_EDGE('',*,*,#6282,.T.);
#9204=ORIENTED_EDGE('',*,*,#6279,.T.);
#9205=ORIENTED_EDGE('',*,*,#6276,.T.);
#9206=ORIENTED_EDGE('',*,*,#6273,.T.);
#9207=ORIENTED_EDGE('',*,*,#6270,.T.);
#9208=ORIENTED_EDGE('',*,*,#6258,.T.);
#9209=ORIENTED_EDGE('',*,*,#6287,.F.);
#9210=ORIENTED_EDGE('',*,*,#6288,.T.);
#9211=ORIENTED_EDGE('',*,*,#6289,.T.);
#9212=ORIENTED_EDGE('',*,*,#6290,.T.);
#9213=ORIENTED_EDGE('',*,*,#6291,.F.);
#9214=ORIENTED_EDGE('',*,*,#6292,.T.);
#9215=ORIENTED_EDGE('',*,*,#6287,.T.);
#9216=ORIENTED_EDGE('',*,*,#6293,.T.);
#9217=ORIENTED_EDGE('',*,*,#6294,.F.);
#9218=ORIENTED_EDGE('',*,*,#6295,.T.);
#9219=ORIENTED_EDGE('',*,*,#6291,.T.);
#9220=ORIENTED_EDGE('',*,*,#6296,.T.);
#9221=ORIENTED_EDGE('',*,*,#6297,.F.);
#9222=ORIENTED_EDGE('',*,*,#6298,.T.);
#9223=ORIENTED_EDGE('',*,*,#6294,.T.);
#9224=ORIENTED_EDGE('',*,*,#6299,.T.);
#9225=ORIENTED_EDGE('',*,*,#6300,.F.);
#9226=ORIENTED_EDGE('',*,*,#6301,.T.);
#9227=ORIENTED_EDGE('',*,*,#6297,.T.);
#9228=ORIENTED_EDGE('',*,*,#6302,.T.);
#9229=ORIENTED_EDGE('',*,*,#6303,.F.);
#9230=ORIENTED_EDGE('',*,*,#6304,.T.);
#9231=ORIENTED_EDGE('',*,*,#6300,.T.);
#9232=ORIENTED_EDGE('',*,*,#6305,.T.);
#9233=ORIENTED_EDGE('',*,*,#6306,.F.);
#9234=ORIENTED_EDGE('',*,*,#6307,.T.);
#9235=ORIENTED_EDGE('',*,*,#6303,.T.);
#9236=ORIENTED_EDGE('',*,*,#6308,.T.);
#9237=ORIENTED_EDGE('',*,*,#6309,.F.);
#9238=ORIENTED_EDGE('',*,*,#6310,.T.);
#9239=ORIENTED_EDGE('',*,*,#6306,.T.);
#9240=ORIENTED_EDGE('',*,*,#6311,.T.);
#9241=ORIENTED_EDGE('',*,*,#6312,.F.);
#9242=ORIENTED_EDGE('',*,*,#6313,.T.);
#9243=ORIENTED_EDGE('',*,*,#6309,.T.);
#9244=ORIENTED_EDGE('',*,*,#6314,.T.);
#9245=ORIENTED_EDGE('',*,*,#6315,.F.);
#9246=ORIENTED_EDGE('',*,*,#6316,.T.);
#9247=ORIENTED_EDGE('',*,*,#6312,.T.);
#9248=ORIENTED_EDGE('',*,*,#6317,.T.);
#9249=ORIENTED_EDGE('',*,*,#6318,.F.);
#9250=ORIENTED_EDGE('',*,*,#6319,.T.);
#9251=ORIENTED_EDGE('',*,*,#6320,.F.);
#9252=ORIENTED_EDGE('',*,*,#6321,.F.);
#9253=ORIENTED_EDGE('',*,*,#6322,.F.);
#9254=ORIENTED_EDGE('',*,*,#6323,.T.);
#9255=ORIENTED_EDGE('',*,*,#6318,.T.);
#9256=ORIENTED_EDGE('',*,*,#6324,.F.);
#9257=ORIENTED_EDGE('',*,*,#6325,.F.);
#9258=ORIENTED_EDGE('',*,*,#6326,.T.);
#9259=ORIENTED_EDGE('',*,*,#6322,.T.);
#9260=ORIENTED_EDGE('',*,*,#6327,.F.);
#9261=ORIENTED_EDGE('',*,*,#6328,.F.);
#9262=ORIENTED_EDGE('',*,*,#6329,.T.);
#9263=ORIENTED_EDGE('',*,*,#6325,.T.);
#9264=ORIENTED_EDGE('',*,*,#6330,.F.);
#9265=ORIENTED_EDGE('',*,*,#6331,.F.);
#9266=ORIENTED_EDGE('',*,*,#6332,.T.);
#9267=ORIENTED_EDGE('',*,*,#6328,.T.);
#9268=ORIENTED_EDGE('',*,*,#6333,.F.);
#9269=ORIENTED_EDGE('',*,*,#6334,.F.);
#9270=ORIENTED_EDGE('',*,*,#6335,.T.);
#9271=ORIENTED_EDGE('',*,*,#6331,.T.);
#9272=ORIENTED_EDGE('',*,*,#6336,.F.);
#9273=ORIENTED_EDGE('',*,*,#6337,.F.);
#9274=ORIENTED_EDGE('',*,*,#6338,.T.);
#9275=ORIENTED_EDGE('',*,*,#6334,.T.);
#9276=ORIENTED_EDGE('',*,*,#6339,.F.);
#9277=ORIENTED_EDGE('',*,*,#6340,.F.);
#9278=ORIENTED_EDGE('',*,*,#6341,.T.);
#9279=ORIENTED_EDGE('',*,*,#6337,.T.);
#9280=ORIENTED_EDGE('',*,*,#6342,.F.);
#9281=ORIENTED_EDGE('',*,*,#6343,.F.);
#9282=ORIENTED_EDGE('',*,*,#6344,.T.);
#9283=ORIENTED_EDGE('',*,*,#6340,.T.);
#9284=ORIENTED_EDGE('',*,*,#6345,.F.);
#9285=ORIENTED_EDGE('',*,*,#6346,.F.);
#9286=ORIENTED_EDGE('',*,*,#6347,.F.);
#9287=ORIENTED_EDGE('',*,*,#6317,.F.);
#9288=ORIENTED_EDGE('',*,*,#6314,.F.);
#9289=ORIENTED_EDGE('',*,*,#6311,.F.);
#9290=ORIENTED_EDGE('',*,*,#6308,.F.);
#9291=ORIENTED_EDGE('',*,*,#6305,.F.);
#9292=ORIENTED_EDGE('',*,*,#6302,.F.);
#9293=ORIENTED_EDGE('',*,*,#6299,.F.);
#9294=ORIENTED_EDGE('',*,*,#6296,.F.);
#9295=ORIENTED_EDGE('',*,*,#6293,.F.);
#9296=ORIENTED_EDGE('',*,*,#6290,.F.);
#9297=ORIENTED_EDGE('',*,*,#6348,.F.);
#9298=ORIENTED_EDGE('',*,*,#6349,.T.);
#9299=ORIENTED_EDGE('',*,*,#6345,.T.);
#9300=ORIENTED_EDGE('',*,*,#6342,.T.);
#9301=ORIENTED_EDGE('',*,*,#6339,.T.);
#9302=ORIENTED_EDGE('',*,*,#6336,.T.);
#9303=ORIENTED_EDGE('',*,*,#6333,.T.);
#9304=ORIENTED_EDGE('',*,*,#6330,.T.);
#9305=ORIENTED_EDGE('',*,*,#6327,.T.);
#9306=ORIENTED_EDGE('',*,*,#6324,.T.);
#9307=ORIENTED_EDGE('',*,*,#6321,.T.);
#9308=ORIENTED_EDGE('',*,*,#6343,.T.);
#9309=ORIENTED_EDGE('',*,*,#6349,.F.);
#9310=ORIENTED_EDGE('',*,*,#6350,.F.);
#9311=ORIENTED_EDGE('',*,*,#6351,.T.);
#9312=ORIENTED_EDGE('',*,*,#6352,.F.);
#9313=ORIENTED_EDGE('',*,*,#6319,.F.);
#9314=ORIENTED_EDGE('',*,*,#6323,.F.);
#9315=ORIENTED_EDGE('',*,*,#6326,.F.);
#9316=ORIENTED_EDGE('',*,*,#6329,.F.);
#9317=ORIENTED_EDGE('',*,*,#6332,.F.);
#9318=ORIENTED_EDGE('',*,*,#6335,.F.);
#9319=ORIENTED_EDGE('',*,*,#6338,.F.);
#9320=ORIENTED_EDGE('',*,*,#6341,.F.);
#9321=ORIENTED_EDGE('',*,*,#6344,.F.);
#9322=ORIENTED_EDGE('',*,*,#6351,.F.);
#9323=ORIENTED_EDGE('',*,*,#6353,.F.);
#9324=ORIENTED_EDGE('',*,*,#6288,.F.);
#9325=ORIENTED_EDGE('',*,*,#6292,.F.);
#9326=ORIENTED_EDGE('',*,*,#6295,.F.);
#9327=ORIENTED_EDGE('',*,*,#6298,.F.);
#9328=ORIENTED_EDGE('',*,*,#6301,.F.);
#9329=ORIENTED_EDGE('',*,*,#6304,.F.);
#9330=ORIENTED_EDGE('',*,*,#6307,.F.);
#9331=ORIENTED_EDGE('',*,*,#6310,.F.);
#9332=ORIENTED_EDGE('',*,*,#6313,.F.);
#9333=ORIENTED_EDGE('',*,*,#6316,.F.);
#9334=ORIENTED_EDGE('',*,*,#6354,.F.);
#9335=ORIENTED_EDGE('',*,*,#6315,.T.);
#9336=ORIENTED_EDGE('',*,*,#6347,.T.);
#9337=ORIENTED_EDGE('',*,*,#6355,.F.);
#9338=ORIENTED_EDGE('',*,*,#6354,.T.);
#9339=ORIENTED_EDGE('',*,*,#6356,.T.);
#9340=ORIENTED_EDGE('',*,*,#6357,.F.);
#9341=ORIENTED_EDGE('',*,*,#6358,.F.);
#9342=ORIENTED_EDGE('',*,*,#6359,.F.);
#9343=ORIENTED_EDGE('',*,*,#6356,.F.);
#9344=ORIENTED_EDGE('',*,*,#6360,.T.);
#9345=ORIENTED_EDGE('',*,*,#6358,.T.);
#9346=ORIENTED_EDGE('',*,*,#6360,.F.);
#9347=ORIENTED_EDGE('',*,*,#6359,.T.);
#9348=ORIENTED_EDGE('',*,*,#6361,.T.);
#9349=ORIENTED_EDGE('',*,*,#6362,.T.);
#9350=ORIENTED_EDGE('',*,*,#6361,.F.);
#9351=ORIENTED_EDGE('',*,*,#6363,.T.);
#9352=ORIENTED_EDGE('',*,*,#6362,.F.);
#9353=ORIENTED_EDGE('',*,*,#6364,.F.);
#9354=ORIENTED_EDGE('',*,*,#6365,.F.);
#9355=ORIENTED_EDGE('',*,*,#6363,.F.);
#9356=ORIENTED_EDGE('',*,*,#6366,.T.);
#9357=ORIENTED_EDGE('',*,*,#6364,.T.);
#9358=ORIENTED_EDGE('',*,*,#6366,.F.);
#9359=ORIENTED_EDGE('',*,*,#6365,.T.);
#9360=ORIENTED_EDGE('',*,*,#6367,.T.);
#9361=ORIENTED_EDGE('',*,*,#6368,.T.);
#9362=ORIENTED_EDGE('',*,*,#6367,.F.);
#9363=ORIENTED_EDGE('',*,*,#6369,.T.);
#9364=ORIENTED_EDGE('',*,*,#6368,.F.);
#9365=ORIENTED_EDGE('',*,*,#6370,.F.);
#9366=ORIENTED_EDGE('',*,*,#6371,.F.);
#9367=ORIENTED_EDGE('',*,*,#6369,.F.);
#9368=ORIENTED_EDGE('',*,*,#6372,.T.);
#9369=ORIENTED_EDGE('',*,*,#6370,.T.);
#9370=ORIENTED_EDGE('',*,*,#6372,.F.);
#9371=ORIENTED_EDGE('',*,*,#6371,.T.);
#9372=ORIENTED_EDGE('',*,*,#6373,.T.);
#9373=ORIENTED_EDGE('',*,*,#6374,.T.);
#9374=ORIENTED_EDGE('',*,*,#6373,.F.);
#9375=ORIENTED_EDGE('',*,*,#6375,.F.);
#9376=ORIENTED_EDGE('',*,*,#6376,.T.);
#9377=ORIENTED_EDGE('',*,*,#6357,.T.);
#9378=ORIENTED_EDGE('',*,*,#6376,.F.);
#9379=ORIENTED_EDGE('',*,*,#6374,.F.);
#9380=ORIENTED_EDGE('',*,*,#6377,.F.);
#9381=ORIENTED_EDGE('',*,*,#6378,.T.);
#9382=ORIENTED_EDGE('',*,*,#6353,.T.);
#9383=ORIENTED_EDGE('',*,*,#6350,.T.);
#9384=ORIENTED_EDGE('',*,*,#6348,.T.);
#9385=ORIENTED_EDGE('',*,*,#6289,.F.);
#9386=ORIENTED_EDGE('',*,*,#6378,.F.);
#9387=ORIENTED_EDGE('',*,*,#6379,.T.);
#9388=ORIENTED_EDGE('',*,*,#6380,.T.);
#9389=ORIENTED_EDGE('',*,*,#6379,.F.);
#9390=ORIENTED_EDGE('',*,*,#6380,.F.);
#9391=ORIENTED_EDGE('',*,*,#6375,.T.);
#9392=ORIENTED_EDGE('',*,*,#6381,.F.);
#9393=ORIENTED_EDGE('',*,*,#6382,.T.);
#9394=ORIENTED_EDGE('',*,*,#6377,.T.);
#9395=ORIENTED_EDGE('',*,*,#6382,.F.);
#9396=ORIENTED_EDGE('',*,*,#6352,.T.);
#9397=ORIENTED_EDGE('',*,*,#6355,.T.);
#9398=ORIENTED_EDGE('',*,*,#6346,.T.);
#9399=ORIENTED_EDGE('',*,*,#6320,.T.);
#9400=ORIENTED_EDGE('',*,*,#6381,.T.);
#9401=ORIENTED_EDGE('',*,*,#6383,.F.);
#9402=ORIENTED_EDGE('',*,*,#6384,.T.);
#9403=ORIENTED_EDGE('',*,*,#6385,.T.);
#9404=ORIENTED_EDGE('',*,*,#6384,.F.);
#9405=ORIENTED_EDGE('',*,*,#6386,.F.);
#9406=ORIENTED_EDGE('',*,*,#6387,.T.);
#9407=ORIENTED_EDGE('',*,*,#6388,.T.);
#9408=ORIENTED_EDGE('',*,*,#6387,.F.);
#9409=ORIENTED_EDGE('',*,*,#6386,.T.);
#9410=ORIENTED_EDGE('',*,*,#6383,.T.);
#9411=ORIENTED_EDGE('',*,*,#6388,.F.);
#9412=ORIENTED_EDGE('',*,*,#6385,.F.);
#9413=CYLINDRICAL_SURFACE('',#10506,1.666);
#9414=CYLINDRICAL_SURFACE('',#10509,1.666);
#9415=CYLINDRICAL_SURFACE('',#10510,1.666);
#9416=CYLINDRICAL_SURFACE('',#10511,1.666);
#9417=CYLINDRICAL_SURFACE('',#10512,1.666);
#9418=CYLINDRICAL_SURFACE('',#10513,1.666);
#9419=CYLINDRICAL_SURFACE('',#10514,1.666);
#9420=CYLINDRICAL_SURFACE('',#10515,1.666);
#9421=CYLINDRICAL_SURFACE('',#10516,1.666);
#9422=CYLINDRICAL_SURFACE('',#10517,1.666);
#9423=CYLINDRICAL_SURFACE('',#10518,1.666);
#9424=CYLINDRICAL_SURFACE('',#10519,1.666);
#9425=CYLINDRICAL_SURFACE('',#10520,1.666);
#9426=CYLINDRICAL_SURFACE('',#10521,1.666);
#9427=CYLINDRICAL_SURFACE('',#10522,1.666);
#9428=CYLINDRICAL_SURFACE('',#10524,2.05475000000001);
#9429=CYLINDRICAL_SURFACE('',#10526,2.05475000000001);
#9430=CYLINDRICAL_SURFACE('',#10527,2.05475000000001);
#9431=CYLINDRICAL_SURFACE('',#10528,2.05475000000001);
#9432=CYLINDRICAL_SURFACE('',#10529,2.05475000000001);
#9433=CYLINDRICAL_SURFACE('',#10530,2.05475000000001);
#9434=CYLINDRICAL_SURFACE('',#10531,2.05475000000001);
#9435=CYLINDRICAL_SURFACE('',#10532,2.05475000000001);
#9436=CYLINDRICAL_SURFACE('',#10533,2.05475000000001);
#9437=CYLINDRICAL_SURFACE('',#10534,2.05475000000001);
#9438=CYLINDRICAL_SURFACE('',#10535,2.05475000000001);
#9439=CYLINDRICAL_SURFACE('',#10536,2.05475000000001);
#9440=CYLINDRICAL_SURFACE('',#10537,2.05475000000001);
#9441=CYLINDRICAL_SURFACE('',#10538,2.05475000000001);
#9442=CYLINDRICAL_SURFACE('',#10539,2.05475000000001);
#9443=CYLINDRICAL_SURFACE('',#10540,2.05475000000001);
#9444=CYLINDRICAL_SURFACE('',#10542,1.666);
#9445=CYLINDRICAL_SURFACE('',#10545,1.666);
#9446=CYLINDRICAL_SURFACE('',#10546,1.666);
#9447=CYLINDRICAL_SURFACE('',#10547,1.666);
#9448=CYLINDRICAL_SURFACE('',#10548,1.666);
#9449=CYLINDRICAL_SURFACE('',#10549,1.666);
#9450=CYLINDRICAL_SURFACE('',#10550,1.666);
#9451=CYLINDRICAL_SURFACE('',#10551,1.666);
#9452=CYLINDRICAL_SURFACE('',#10552,1.666);
#9453=CYLINDRICAL_SURFACE('',#10553,1.666);
#9454=CYLINDRICAL_SURFACE('',#10554,1.666);
#9455=CYLINDRICAL_SURFACE('',#10555,1.666);
#9456=CYLINDRICAL_SURFACE('',#10556,1.666);
#9457=CYLINDRICAL_SURFACE('',#10557,1.666);
#9458=CYLINDRICAL_SURFACE('',#10558,1.666);
#9459=CYLINDRICAL_SURFACE('',#10560,2.05475);
#9460=CYLINDRICAL_SURFACE('',#10562,2.05475);
#9461=CYLINDRICAL_SURFACE('',#10563,2.05475);
#9462=CYLINDRICAL_SURFACE('',#10564,2.05475);
#9463=CYLINDRICAL_SURFACE('',#10565,2.05475);
#9464=CYLINDRICAL_SURFACE('',#10566,2.05475);
#9465=CYLINDRICAL_SURFACE('',#10567,2.05475);
#9466=CYLINDRICAL_SURFACE('',#10568,2.05475);
#9467=CYLINDRICAL_SURFACE('',#10569,2.05475);
#9468=CYLINDRICAL_SURFACE('',#10570,2.05475);
#9469=CYLINDRICAL_SURFACE('',#10571,2.05475);
#9470=CYLINDRICAL_SURFACE('',#10572,2.05475);
#9471=CYLINDRICAL_SURFACE('',#10573,2.05475);
#9472=CYLINDRICAL_SURFACE('',#10574,2.05475);
#9473=CYLINDRICAL_SURFACE('',#10575,2.05475);
#9474=CYLINDRICAL_SURFACE('',#10576,2.05475);
#9475=CYLINDRICAL_SURFACE('',#10578,1.666);
#9476=CYLINDRICAL_SURFACE('',#10581,1.666);
#9477=CYLINDRICAL_SURFACE('',#10582,1.666);
#9478=CYLINDRICAL_SURFACE('',#10583,1.666);
#9479=CYLINDRICAL_SURFACE('',#10584,1.666);
#9480=CYLINDRICAL_SURFACE('',#10585,1.666);
#9481=CYLINDRICAL_SURFACE('',#10586,1.666);
#9482=CYLINDRICAL_SURFACE('',#10587,1.666);
#9483=CYLINDRICAL_SURFACE('',#10588,1.666);
#9484=CYLINDRICAL_SURFACE('',#10589,1.666);
#9485=CYLINDRICAL_SURFACE('',#10590,1.666);
#9486=CYLINDRICAL_SURFACE('',#10591,1.666);
#9487=CYLINDRICAL_SURFACE('',#10592,1.666);
#9488=CYLINDRICAL_SURFACE('',#10593,1.666);
#9489=CYLINDRICAL_SURFACE('',#10594,1.666);
#9490=CYLINDRICAL_SURFACE('',#10596,2.05475000000001);
#9491=CYLINDRICAL_SURFACE('',#10598,2.05475000000001);
#9492=CYLINDRICAL_SURFACE('',#10599,2.05475000000001);
#9493=CYLINDRICAL_SURFACE('',#10600,2.05475000000001);
#9494=CYLINDRICAL_SURFACE('',#10601,2.05475000000001);
#9495=CYLINDRICAL_SURFACE('',#10602,2.05475000000001);
#9496=CYLINDRICAL_SURFACE('',#10603,2.05475000000001);
#9497=CYLINDRICAL_SURFACE('',#10604,2.05475000000001);
#9498=CYLINDRICAL_SURFACE('',#10605,2.05475000000001);
#9499=CYLINDRICAL_SURFACE('',#10606,2.05475000000001);
#9500=CYLINDRICAL_SURFACE('',#10607,2.05475000000001);
#9501=CYLINDRICAL_SURFACE('',#10608,2.05475000000001);
#9502=CYLINDRICAL_SURFACE('',#10609,2.05475000000001);
#9503=CYLINDRICAL_SURFACE('',#10610,2.05475000000001);
#9504=CYLINDRICAL_SURFACE('',#10611,2.05475000000001);
#9505=CYLINDRICAL_SURFACE('',#10612,2.05475000000001);
#9506=CYLINDRICAL_SURFACE('',#10614,1.666);
#9507=CYLINDRICAL_SURFACE('',#10617,1.666);
#9508=CYLINDRICAL_SURFACE('',#10618,1.666);
#9509=CYLINDRICAL_SURFACE('',#10619,1.666);
#9510=CYLINDRICAL_SURFACE('',#10620,1.666);
#9511=CYLINDRICAL_SURFACE('',#10621,1.666);
#9512=CYLINDRICAL_SURFACE('',#10622,1.666);
#9513=CYLINDRICAL_SURFACE('',#10623,1.666);
#9514=CYLINDRICAL_SURFACE('',#10624,1.666);
#9515=CYLINDRICAL_SURFACE('',#10625,1.666);
#9516=CYLINDRICAL_SURFACE('',#10626,1.666);
#9517=CYLINDRICAL_SURFACE('',#10627,1.666);
#9518=CYLINDRICAL_SURFACE('',#10628,1.666);
#9519=CYLINDRICAL_SURFACE('',#10629,1.666);
#9520=CYLINDRICAL_SURFACE('',#10630,1.666);
#9521=CYLINDRICAL_SURFACE('',#10632,2.05475);
#9522=CYLINDRICAL_SURFACE('',#10634,2.05475);
#9523=CYLINDRICAL_SURFACE('',#10635,2.05475);
#9524=CYLINDRICAL_SURFACE('',#10636,2.05475);
#9525=CYLINDRICAL_SURFACE('',#10637,2.05475);
#9526=CYLINDRICAL_SURFACE('',#10638,2.05475);
#9527=CYLINDRICAL_SURFACE('',#10639,2.05475);
#9528=CYLINDRICAL_SURFACE('',#10640,2.05475);
#9529=CYLINDRICAL_SURFACE('',#10641,2.05475);
#9530=CYLINDRICAL_SURFACE('',#10642,2.05475);
#9531=CYLINDRICAL_SURFACE('',#10643,2.05475);
#9532=CYLINDRICAL_SURFACE('',#10644,2.05475);
#9533=CYLINDRICAL_SURFACE('',#10645,2.05475);
#9534=CYLINDRICAL_SURFACE('',#10646,2.05475);
#9535=CYLINDRICAL_SURFACE('',#10647,2.05475);
#9536=CYLINDRICAL_SURFACE('',#10648,2.05475);
#9537=CYLINDRICAL_SURFACE('',#10650,2.5175);
#9538=CYLINDRICAL_SURFACE('',#10653,2.5175);
#9539=CYLINDRICAL_SURFACE('',#10654,2.5175);
#9540=CYLINDRICAL_SURFACE('',#10655,2.5175);
#9541=CYLINDRICAL_SURFACE('',#10656,2.5175);
#9542=CYLINDRICAL_SURFACE('',#10657,2.5175);
#9543=CYLINDRICAL_SURFACE('',#10658,2.5175);
#9544=CYLINDRICAL_SURFACE('',#10659,2.5175);
#9545=CYLINDRICAL_SURFACE('',#10660,2.5175);
#9546=CYLINDRICAL_SURFACE('',#10661,2.5175);
#9547=CYLINDRICAL_SURFACE('',#10662,2.5175);
#9548=CYLINDRICAL_SURFACE('',#10663,2.5175);
#9549=CYLINDRICAL_SURFACE('',#10664,2.5175);
#9550=CYLINDRICAL_SURFACE('',#10665,2.5175);
#9551=CYLINDRICAL_SURFACE('',#10666,2.5175);
#9552=CYLINDRICAL_SURFACE('',#10668,2.5175);
#9553=CYLINDRICAL_SURFACE('',#10671,2.5175);
#9554=CYLINDRICAL_SURFACE('',#10672,2.5175);
#9555=CYLINDRICAL_SURFACE('',#10673,2.5175);
#9556=CYLINDRICAL_SURFACE('',#10674,2.5175);
#9557=CYLINDRICAL_SURFACE('',#10675,2.5175);
#9558=CYLINDRICAL_SURFACE('',#10676,2.5175);
#9559=CYLINDRICAL_SURFACE('',#10677,2.5175);
#9560=CYLINDRICAL_SURFACE('',#10678,2.5175);
#9561=CYLINDRICAL_SURFACE('',#10679,2.5175);
#9562=CYLINDRICAL_SURFACE('',#10680,2.5175);
#9563=CYLINDRICAL_SURFACE('',#10681,2.5175);
#9564=CYLINDRICAL_SURFACE('',#10682,2.5175);
#9565=CYLINDRICAL_SURFACE('',#10683,2.5175);
#9566=CYLINDRICAL_SURFACE('',#10684,2.5175);
#9567=CYLINDRICAL_SURFACE('',#10686,3.0735);
#9568=CYLINDRICAL_SURFACE('',#10688,3.0735);
#9569=CYLINDRICAL_SURFACE('',#10689,3.0735);
#9570=CYLINDRICAL_SURFACE('',#10690,3.0735);
#9571=CYLINDRICAL_SURFACE('',#10691,3.0735);
#9572=CYLINDRICAL_SURFACE('',#10692,3.0735);
#9573=CYLINDRICAL_SURFACE('',#10693,3.0735);
#9574=CYLINDRICAL_SURFACE('',#10694,3.0735);
#9575=CYLINDRICAL_SURFACE('',#10695,3.0735);
#9576=CYLINDRICAL_SURFACE('',#10696,3.0735);
#9577=CYLINDRICAL_SURFACE('',#10697,3.0735);
#9578=CYLINDRICAL_SURFACE('',#10698,3.0735);
#9579=CYLINDRICAL_SURFACE('',#10699,3.0735);
#9580=CYLINDRICAL_SURFACE('',#10700,3.0735);
#9581=CYLINDRICAL_SURFACE('',#10701,3.0735);
#9582=CYLINDRICAL_SURFACE('',#10703,3.0735);
#9583=CYLINDRICAL_SURFACE('',#10705,3.0735);
#9584=CYLINDRICAL_SURFACE('',#10706,3.0735);
#9585=CYLINDRICAL_SURFACE('',#10707,3.0735);
#9586=CYLINDRICAL_SURFACE('',#10708,3.0735);
#9587=CYLINDRICAL_SURFACE('',#10709,3.0735);
#9588=CYLINDRICAL_SURFACE('',#10710,3.0735);
#9589=CYLINDRICAL_SURFACE('',#10711,3.0735);
#9590=CYLINDRICAL_SURFACE('',#10712,3.0735);
#9591=CYLINDRICAL_SURFACE('',#10713,3.0735);
#9592=CYLINDRICAL_SURFACE('',#10714,3.0735);
#9593=CYLINDRICAL_SURFACE('',#10715,3.0735);
#9594=CYLINDRICAL_SURFACE('',#10716,3.0735);
#9595=CYLINDRICAL_SURFACE('',#10717,3.0735);
#9596=CYLINDRICAL_SURFACE('',#10718,3.07350000000001);
#9597=CYLINDRICAL_SURFACE('',#10720,2.5175);
#9598=CYLINDRICAL_SURFACE('',#10724,2.5175);
#9599=CYLINDRICAL_SURFACE('',#10725,2.5175);
#9600=CYLINDRICAL_SURFACE('',#10726,2.5175);
#9601=CYLINDRICAL_SURFACE('',#10727,2.5175);
#9602=CYLINDRICAL_SURFACE('',#10728,2.5175);
#9603=CYLINDRICAL_SURFACE('',#10729,2.5175);
#9604=CYLINDRICAL_SURFACE('',#10730,2.5175);
#9605=CYLINDRICAL_SURFACE('',#10731,2.5175);
#9606=CYLINDRICAL_SURFACE('',#10732,2.5175);
#9607=CYLINDRICAL_SURFACE('',#10733,2.5175);
#9608=CYLINDRICAL_SURFACE('',#10734,2.5175);
#9609=CYLINDRICAL_SURFACE('',#10735,2.5175);
#9610=CYLINDRICAL_SURFACE('',#10736,2.5175);
#9611=CYLINDRICAL_SURFACE('',#10737,2.5175);
#9612=CYLINDRICAL_SURFACE('',#10739,3.0735);
#9613=CYLINDRICAL_SURFACE('',#10741,3.0735);
#9614=CYLINDRICAL_SURFACE('',#10742,3.0735);
#9615=CYLINDRICAL_SURFACE('',#10743,3.0735);
#9616=CYLINDRICAL_SURFACE('',#10744,3.0735);
#9617=CYLINDRICAL_SURFACE('',#10745,3.0735);
#9618=CYLINDRICAL_SURFACE('',#10746,3.0735);
#9619=CYLINDRICAL_SURFACE('',#10747,3.0735);
#9620=CYLINDRICAL_SURFACE('',#10748,3.0735);
#9621=CYLINDRICAL_SURFACE('',#10749,3.0735);
#9622=CYLINDRICAL_SURFACE('',#10750,3.0735);
#9623=CYLINDRICAL_SURFACE('',#10751,3.0735);
#9624=CYLINDRICAL_SURFACE('',#10752,3.0735);
#9625=CYLINDRICAL_SURFACE('',#10753,3.0735);
#9626=CYLINDRICAL_SURFACE('',#10754,3.0735);
#9627=CYLINDRICAL_SURFACE('',#10756,2.5175);
#9628=CYLINDRICAL_SURFACE('',#10760,2.5175);
#9629=CYLINDRICAL_SURFACE('',#10761,2.5175);
#9630=CYLINDRICAL_SURFACE('',#10762,2.5175);
#9631=CYLINDRICAL_SURFACE('',#10763,2.5175);
#9632=CYLINDRICAL_SURFACE('',#10764,2.5175);
#9633=CYLINDRICAL_SURFACE('',#10765,2.5175);
#9634=CYLINDRICAL_SURFACE('',#10766,2.5175);
#9635=CYLINDRICAL_SURFACE('',#10767,2.5175);
#9636=CYLINDRICAL_SURFACE('',#10768,2.5175);
#9637=CYLINDRICAL_SURFACE('',#10769,2.5175);
#9638=CYLINDRICAL_SURFACE('',#10770,2.5175);
#9639=CYLINDRICAL_SURFACE('',#10771,2.5175);
#9640=CYLINDRICAL_SURFACE('',#10772,2.5175);
#9641=CYLINDRICAL_SURFACE('',#10773,2.5175);
#9642=CYLINDRICAL_SURFACE('',#10775,3.0735);
#9643=CYLINDRICAL_SURFACE('',#10777,3.0735);
#9644=CYLINDRICAL_SURFACE('',#10778,3.0735);
#9645=CYLINDRICAL_SURFACE('',#10779,3.0735);
#9646=CYLINDRICAL_SURFACE('',#10780,3.0735);
#9647=CYLINDRICAL_SURFACE('',#10781,3.0735);
#9648=CYLINDRICAL_SURFACE('',#10782,3.0735);
#9649=CYLINDRICAL_SURFACE('',#10783,3.0735);
#9650=CYLINDRICAL_SURFACE('',#10784,3.0735);
#9651=CYLINDRICAL_SURFACE('',#10785,3.0735);
#9652=CYLINDRICAL_SURFACE('',#10786,3.0735);
#9653=CYLINDRICAL_SURFACE('',#10787,3.0735);
#9654=CYLINDRICAL_SURFACE('',#10788,3.0735);
#9655=CYLINDRICAL_SURFACE('',#10789,3.0735);
#9656=CYLINDRICAL_SURFACE('',#10790,3.0735);
#9657=CYLINDRICAL_SURFACE('',#10792,7.263);
#9658=CYLINDRICAL_SURFACE('',#10794,7.263);
#9659=CYLINDRICAL_SURFACE('',#10795,7.263);
#9660=CYLINDRICAL_SURFACE('',#10796,7.263);
#9661=CYLINDRICAL_SURFACE('',#10797,7.263);
#9662=CYLINDRICAL_SURFACE('',#10798,7.263);
#9663=CYLINDRICAL_SURFACE('',#10799,7.263);
#9664=CYLINDRICAL_SURFACE('',#10800,7.263);
#9665=CYLINDRICAL_SURFACE('',#10802,8.1015);
#9666=CYLINDRICAL_SURFACE('',#10804,8.1015);
#9667=CYLINDRICAL_SURFACE('',#10805,8.1015);
#9668=CYLINDRICAL_SURFACE('',#10806,8.1015);
#9669=CYLINDRICAL_SURFACE('',#10807,8.1015);
#9670=CYLINDRICAL_SURFACE('',#10808,8.1015);
#9671=CYLINDRICAL_SURFACE('',#10809,8.1015);
#9672=CYLINDRICAL_SURFACE('',#10810,8.1015);
#9673=CYLINDRICAL_SURFACE('',#10812,8.1015);
#9674=CYLINDRICAL_SURFACE('',#10815,7.263);
#9675=CYLINDRICAL_SURFACE('',#10816,12.);
#9676=CYLINDRICAL_SURFACE('',#10820,3.0735);
#9677=CYLINDRICAL_SURFACE('',#10821,2.5175);
#9678=CYLINDRICAL_SURFACE('',#10823,3.0735);
#9679=CYLINDRICAL_SURFACE('',#10824,2.5175);
#9680=CYLINDRICAL_SURFACE('',#10829,3.0735);
#9681=CYLINDRICAL_SURFACE('',#10830,2.5175);
#9682=CYLINDRICAL_SURFACE('',#10835,3.0735);
#9683=CYLINDRICAL_SURFACE('',#10836,2.5175);
#9684=CYLINDRICAL_SURFACE('',#10837,2.5175);
#9685=CYLINDRICAL_SURFACE('',#10840,2.5175);
#9686=CYLINDRICAL_SURFACE('',#10842,2.05475);
#9687=CYLINDRICAL_SURFACE('',#10843,1.666);
#9688=CYLINDRICAL_SURFACE('',#10845,2.05475000000001);
#9689=CYLINDRICAL_SURFACE('',#10846,1.666);
#9690=CYLINDRICAL_SURFACE('',#10848,2.05475);
#9691=CYLINDRICAL_SURFACE('',#10849,1.666);
#9692=CYLINDRICAL_SURFACE('',#10851,2.05475000000001);
#9693=CYLINDRICAL_SURFACE('',#10852,1.666);
#9694=CYLINDRICAL_SURFACE('',#10857,5.);
#9695=CYLINDRICAL_SURFACE('',#10860,5.);
#9696=CYLINDRICAL_SURFACE('',#10863,5.);
#9697=CYLINDRICAL_SURFACE('',#10866,5.);
#9698=CYLINDRICAL_SURFACE('',#10869,5.);
#9699=CYLINDRICAL_SURFACE('',#10872,5.);
#9700=CYLINDRICAL_SURFACE('',#10875,5.);
#9701=CYLINDRICAL_SURFACE('',#10878,5.);
#9702=CYLINDRICAL_SURFACE('',#10881,5.);
#9703=CYLINDRICAL_SURFACE('',#10884,5.);
#9704=CYLINDRICAL_SURFACE('',#10887,5.);
#9705=CYLINDRICAL_SURFACE('',#10890,5.);
#9706=CYLINDRICAL_SURFACE('',#10893,5.);
#9707=CYLINDRICAL_SURFACE('',#10896,5.);
#9708=CYLINDRICAL_SURFACE('',#10899,5.);
#9709=CYLINDRICAL_SURFACE('',#10902,5.);
#9710=CYLINDRICAL_SURFACE('',#10905,5.);
#9711=CYLINDRICAL_SURFACE('',#10908,5.);
#9712=CYLINDRICAL_SURFACE('',#10922,2.5);
#9713=CYLINDRICAL_SURFACE('',#10925,2.5);
#9714=CYLINDRICAL_SURFACE('',#10928,2.5);
#9715=CYLINDRICAL_SURFACE('',#10931,2.5);
#9716=CYLINDRICAL_SURFACE('',#10941,2.5);
#9717=CYLINDRICAL_SURFACE('',#10944,2.5);
#9718=CYLINDRICAL_SURFACE('',#10947,2.5);
#9719=CYLINDRICAL_SURFACE('',#10950,2.5);
#9720=CYLINDRICAL_SURFACE('',#10964,4.);
#9721=CYLINDRICAL_SURFACE('',#10967,5.);
#9722=CYLINDRICAL_SURFACE('',#10973,5.);
#9723=CYLINDRICAL_SURFACE('',#10976,5.);
#9724=CYLINDRICAL_SURFACE('',#10979,5.);
#9725=CYLINDRICAL_SURFACE('',#10982,5.);
#9726=CYLINDRICAL_SURFACE('',#10985,5.);
#9727=CYLINDRICAL_SURFACE('',#10988,5.);
#9728=CYLINDRICAL_SURFACE('',#10991,5.);
#9729=CYLINDRICAL_SURFACE('',#10994,5.);
#9730=CYLINDRICAL_SURFACE('',#10997,5.);
#9731=CYLINDRICAL_SURFACE('',#11000,5.);
#9732=CYLINDRICAL_SURFACE('',#11003,5.);
#9733=CYLINDRICAL_SURFACE('',#11006,5.);
#9734=CYLINDRICAL_SURFACE('',#11009,5.);
#9735=CYLINDRICAL_SURFACE('',#11012,5.);
#9736=CYLINDRICAL_SURFACE('',#11015,5.);
#9737=CYLINDRICAL_SURFACE('',#11018,5.);
#9738=CYLINDRICAL_SURFACE('',#11021,5.);
#9739=CYLINDRICAL_SURFACE('',#11024,5.);
#9740=CYLINDRICAL_SURFACE('',#11034,13.);
#9741=CYLINDRICAL_SURFACE('',#11037,4.5);
#9742=CYLINDRICAL_SURFACE('',#11040,4.5);
#9743=CYLINDRICAL_SURFACE('',#11043,3.5);
#9744=CYLINDRICAL_SURFACE('',#11046,3.5);
#9745=CYLINDRICAL_SURFACE('',#11049,3.5);
#9746=CYLINDRICAL_SURFACE('',#11052,3.5);
#9747=CYLINDRICAL_SURFACE('',#11062,1.954);
#9748=CYLINDRICAL_SURFACE('',#11064,1.954);
#9749=CYLINDRICAL_SURFACE('',#11065,1.954);
#9750=CYLINDRICAL_SURFACE('',#11066,1.954);
#9751=CYLINDRICAL_SURFACE('',#11067,1.954);
#9752=CYLINDRICAL_SURFACE('',#11068,1.954);
#9753=CYLINDRICAL_SURFACE('',#11069,1.954);
#9754=CYLINDRICAL_SURFACE('',#11070,1.954);
#9755=CYLINDRICAL_SURFACE('',#11071,1.954);
#9756=CYLINDRICAL_SURFACE('',#11072,1.954);
#9757=CYLINDRICAL_SURFACE('',#11073,1.954);
#9758=CYLINDRICAL_SURFACE('',#11074,1.954);
#9759=CYLINDRICAL_SURFACE('',#11075,1.954);
#9760=CYLINDRICAL_SURFACE('',#11076,1.954);
#9761=CYLINDRICAL_SURFACE('',#11077,1.954);
#9762=CYLINDRICAL_SURFACE('',#11078,1.954);
#9763=CYLINDRICAL_SURFACE('',#11079,1.5555);
#9764=CYLINDRICAL_SURFACE('',#11081,1.5555);
#9765=CYLINDRICAL_SURFACE('',#11082,1.5555);
#9766=CYLINDRICAL_SURFACE('',#11083,1.5555);
#9767=CYLINDRICAL_SURFACE('',#11084,1.5555);
#9768=CYLINDRICAL_SURFACE('',#11085,1.5555);
#9769=CYLINDRICAL_SURFACE('',#11086,1.5555);
#9770=CYLINDRICAL_SURFACE('',#11087,1.5555);
#9771=CYLINDRICAL_SURFACE('',#11088,1.5555);
#9772=CYLINDRICAL_SURFACE('',#11089,1.5555);
#9773=CYLINDRICAL_SURFACE('',#11090,1.5555);
#9774=CYLINDRICAL_SURFACE('',#11091,1.5555);
#9775=CYLINDRICAL_SURFACE('',#11092,1.5555);
#9776=CYLINDRICAL_SURFACE('',#11093,1.5555);
#9777=CYLINDRICAL_SURFACE('',#11094,1.5555);
#9778=CYLINDRICAL_SURFACE('',#11095,1.5555);
#9779=CYLINDRICAL_SURFACE('',#11099,1.5555);
#9780=CYLINDRICAL_SURFACE('',#11101,1.954);
#9781=CYLINDRICAL_SURFACE('',#11111,3.5);
#9782=CYLINDRICAL_SURFACE('',#11116,2.942);
#9783=CYLINDRICAL_SURFACE('',#11118,2.942);
#9784=CYLINDRICAL_SURFACE('',#11119,2.942);
#9785=CYLINDRICAL_SURFACE('',#11120,2.942);
#9786=CYLINDRICAL_SURFACE('',#11121,2.942);
#9787=CYLINDRICAL_SURFACE('',#11122,2.942);
#9788=CYLINDRICAL_SURFACE('',#11123,2.942);
#9789=CYLINDRICAL_SURFACE('',#11124,2.942);
#9790=CYLINDRICAL_SURFACE('',#11125,2.942);
#9791=CYLINDRICAL_SURFACE('',#11126,2.942);
#9792=CYLINDRICAL_SURFACE('',#11127,2.942);
#9793=CYLINDRICAL_SURFACE('',#11128,2.37175);
#9794=CYLINDRICAL_SURFACE('',#11130,2.37175);
#9795=CYLINDRICAL_SURFACE('',#11131,2.37175);
#9796=CYLINDRICAL_SURFACE('',#11132,2.37175);
#9797=CYLINDRICAL_SURFACE('',#11133,2.37175);
#9798=CYLINDRICAL_SURFACE('',#11134,2.37175);
#9799=CYLINDRICAL_SURFACE('',#11135,2.37175);
#9800=CYLINDRICAL_SURFACE('',#11136,2.37175);
#9801=CYLINDRICAL_SURFACE('',#11137,2.37175);
#9802=CYLINDRICAL_SURFACE('',#11138,2.37175);
#9803=CYLINDRICAL_SURFACE('',#11139,2.37175);
#9804=CYLINDRICAL_SURFACE('',#11143,2.37175);
#9805=CYLINDRICAL_SURFACE('',#11145,2.942);
#9806=CYLINDRICAL_SURFACE('',#11155,5.);
#9807=CYLINDRICAL_SURFACE('',#11160,7.925);
#9808=CYLINDRICAL_SURFACE('',#11162,7.925);
#9809=CYLINDRICAL_SURFACE('',#11163,7.925);
#9810=CYLINDRICAL_SURFACE('',#11164,7.925);
#9811=CYLINDRICAL_SURFACE('',#11165,7.925);
#9812=CYLINDRICAL_SURFACE('',#11166,7.925);
#9813=CYLINDRICAL_SURFACE('',#11167,7.925);
#9814=CYLINDRICAL_SURFACE('',#11168,7.925);
#9815=CYLINDRICAL_SURFACE('',#11169,7.925);
#9816=CYLINDRICAL_SURFACE('',#11170,7.925);
#9817=CYLINDRICAL_SURFACE('',#11171,7.0685);
#9818=CYLINDRICAL_SURFACE('',#11173,7.0685);
#9819=CYLINDRICAL_SURFACE('',#11174,7.0685);
#9820=CYLINDRICAL_SURFACE('',#11175,7.0685);
#9821=CYLINDRICAL_SURFACE('',#11176,7.0685);
#9822=CYLINDRICAL_SURFACE('',#11177,7.0685);
#9823=CYLINDRICAL_SURFACE('',#11178,7.0685);
#9824=CYLINDRICAL_SURFACE('',#11179,7.0685);
#9825=CYLINDRICAL_SURFACE('',#11180,7.0685);
#9826=CYLINDRICAL_SURFACE('',#11181,7.0685);
#9827=CYLINDRICAL_SURFACE('',#11183,7.925);
#9828=CYLINDRICAL_SURFACE('',#11191,7.);
#9829=CYLINDRICAL_SURFACE('',#11192,6.);
#9830=CYLINDRICAL_SURFACE('',#11199,7.);
#9831=CYLINDRICAL_SURFACE('',#11200,6.);
#9832=CYLINDRICAL_SURFACE('',#11207,7.);
#9833=CYLINDRICAL_SURFACE('',#11208,6.);
#9834=CYLINDRICAL_SURFACE('',#11210,6.);
#9835=CYLINDRICAL_SURFACE('',#11216,12.);
#9836=CYLINDRICAL_SURFACE('',#11219,4.);
#9837=CYLINDRICAL_SURFACE('',#11223,8.5);
#9838=CYLINDRICAL_SURFACE('',#11226,12.);
#9839=ADVANCED_FACE('',(#603),#9413,.F.);
#9840=ADVANCED_FACE('',(#604),#9414,.F.);
#9841=ADVANCED_FACE('',(#605),#9415,.F.);
#9842=ADVANCED_FACE('',(#606),#9416,.F.);
#9843=ADVANCED_FACE('',(#607),#9417,.F.);
#9844=ADVANCED_FACE('',(#608),#9418,.F.);
#9845=ADVANCED_FACE('',(#609),#9419,.F.);
#9846=ADVANCED_FACE('',(#610),#9420,.F.);
#9847=ADVANCED_FACE('',(#611),#9421,.F.);
#9848=ADVANCED_FACE('',(#612),#9422,.F.);
#9849=ADVANCED_FACE('',(#613),#9423,.F.);
#9850=ADVANCED_FACE('',(#614),#9424,.F.);
#9851=ADVANCED_FACE('',(#615),#9425,.F.);
#9852=ADVANCED_FACE('',(#616),#9426,.F.);
#9853=ADVANCED_FACE('',(#617),#9427,.F.);
#9854=ADVANCED_FACE('',(#618),#9428,.F.);
#9855=ADVANCED_FACE('',(#619),#9429,.F.);
#9856=ADVANCED_FACE('',(#620),#9430,.F.);
#9857=ADVANCED_FACE('',(#621),#9431,.F.);
#9858=ADVANCED_FACE('',(#622),#9432,.F.);
#9859=ADVANCED_FACE('',(#623),#9433,.F.);
#9860=ADVANCED_FACE('',(#624),#9434,.F.);
#9861=ADVANCED_FACE('',(#625),#9435,.F.);
#9862=ADVANCED_FACE('',(#626),#9436,.F.);
#9863=ADVANCED_FACE('',(#627),#9437,.F.);
#9864=ADVANCED_FACE('',(#628),#9438,.F.);
#9865=ADVANCED_FACE('',(#629),#9439,.F.);
#9866=ADVANCED_FACE('',(#630),#9440,.F.);
#9867=ADVANCED_FACE('',(#631),#9441,.F.);
#9868=ADVANCED_FACE('',(#632),#9442,.F.);
#9869=ADVANCED_FACE('',(#633),#9443,.F.);
#9870=ADVANCED_FACE('',(#634),#9444,.F.);
#9871=ADVANCED_FACE('',(#635),#9445,.F.);
#9872=ADVANCED_FACE('',(#636),#9446,.F.);
#9873=ADVANCED_FACE('',(#637),#9447,.F.);
#9874=ADVANCED_FACE('',(#638),#9448,.F.);
#9875=ADVANCED_FACE('',(#639),#9449,.F.);
#9876=ADVANCED_FACE('',(#640),#9450,.F.);
#9877=ADVANCED_FACE('',(#641),#9451,.F.);
#9878=ADVANCED_FACE('',(#642),#9452,.F.);
#9879=ADVANCED_FACE('',(#643),#9453,.F.);
#9880=ADVANCED_FACE('',(#644),#9454,.F.);
#9881=ADVANCED_FACE('',(#645),#9455,.F.);
#9882=ADVANCED_FACE('',(#646),#9456,.F.);
#9883=ADVANCED_FACE('',(#647),#9457,.F.);
#9884=ADVANCED_FACE('',(#648),#9458,.F.);
#9885=ADVANCED_FACE('',(#649),#9459,.F.);
#9886=ADVANCED_FACE('',(#650),#9460,.F.);
#9887=ADVANCED_FACE('',(#651),#9461,.F.);
#9888=ADVANCED_FACE('',(#652),#9462,.F.);
#9889=ADVANCED_FACE('',(#653),#9463,.F.);
#9890=ADVANCED_FACE('',(#654),#9464,.F.);
#9891=ADVANCED_FACE('',(#655),#9465,.F.);
#9892=ADVANCED_FACE('',(#656),#9466,.F.);
#9893=ADVANCED_FACE('',(#657),#9467,.F.);
#9894=ADVANCED_FACE('',(#658),#9468,.F.);
#9895=ADVANCED_FACE('',(#659),#9469,.F.);
#9896=ADVANCED_FACE('',(#660),#9470,.F.);
#9897=ADVANCED_FACE('',(#661),#9471,.F.);
#9898=ADVANCED_FACE('',(#662),#9472,.F.);
#9899=ADVANCED_FACE('',(#663),#9473,.F.);
#9900=ADVANCED_FACE('',(#664),#9474,.F.);
#9901=ADVANCED_FACE('',(#665),#9475,.F.);
#9902=ADVANCED_FACE('',(#666),#9476,.F.);
#9903=ADVANCED_FACE('',(#667),#9477,.F.);
#9904=ADVANCED_FACE('',(#668),#9478,.F.);
#9905=ADVANCED_FACE('',(#669),#9479,.F.);
#9906=ADVANCED_FACE('',(#670),#9480,.F.);
#9907=ADVANCED_FACE('',(#671),#9481,.F.);
#9908=ADVANCED_FACE('',(#672),#9482,.F.);
#9909=ADVANCED_FACE('',(#673),#9483,.F.);
#9910=ADVANCED_FACE('',(#674),#9484,.F.);
#9911=ADVANCED_FACE('',(#675),#9485,.F.);
#9912=ADVANCED_FACE('',(#676),#9486,.F.);
#9913=ADVANCED_FACE('',(#677),#9487,.F.);
#9914=ADVANCED_FACE('',(#678),#9488,.F.);
#9915=ADVANCED_FACE('',(#679),#9489,.F.);
#9916=ADVANCED_FACE('',(#680),#9490,.F.);
#9917=ADVANCED_FACE('',(#681),#9491,.F.);
#9918=ADVANCED_FACE('',(#682),#9492,.F.);
#9919=ADVANCED_FACE('',(#683),#9493,.F.);
#9920=ADVANCED_FACE('',(#684),#9494,.F.);
#9921=ADVANCED_FACE('',(#685),#9495,.F.);
#9922=ADVANCED_FACE('',(#686),#9496,.F.);
#9923=ADVANCED_FACE('',(#687),#9497,.F.);
#9924=ADVANCED_FACE('',(#688),#9498,.F.);
#9925=ADVANCED_FACE('',(#689),#9499,.F.);
#9926=ADVANCED_FACE('',(#690),#9500,.F.);
#9927=ADVANCED_FACE('',(#691),#9501,.F.);
#9928=ADVANCED_FACE('',(#692),#9502,.F.);
#9929=ADVANCED_FACE('',(#693),#9503,.F.);
#9930=ADVANCED_FACE('',(#694),#9504,.F.);
#9931=ADVANCED_FACE('',(#695),#9505,.F.);
#9932=ADVANCED_FACE('',(#696),#9506,.F.);
#9933=ADVANCED_FACE('',(#697),#9507,.F.);
#9934=ADVANCED_FACE('',(#698),#9508,.F.);
#9935=ADVANCED_FACE('',(#699),#9509,.F.);
#9936=ADVANCED_FACE('',(#700),#9510,.F.);
#9937=ADVANCED_FACE('',(#701),#9511,.F.);
#9938=ADVANCED_FACE('',(#702),#9512,.F.);
#9939=ADVANCED_FACE('',(#703),#9513,.F.);
#9940=ADVANCED_FACE('',(#704),#9514,.F.);
#9941=ADVANCED_FACE('',(#705),#9515,.F.);
#9942=ADVANCED_FACE('',(#706),#9516,.F.);
#9943=ADVANCED_FACE('',(#707),#9517,.F.);
#9944=ADVANCED_FACE('',(#708),#9518,.F.);
#9945=ADVANCED_FACE('',(#709),#9519,.F.);
#9946=ADVANCED_FACE('',(#710),#9520,.F.);
#9947=ADVANCED_FACE('',(#711),#9521,.F.);
#9948=ADVANCED_FACE('',(#712),#9522,.F.);
#9949=ADVANCED_FACE('',(#713),#9523,.F.);
#9950=ADVANCED_FACE('',(#714),#9524,.F.);
#9951=ADVANCED_FACE('',(#715),#9525,.F.);
#9952=ADVANCED_FACE('',(#716),#9526,.F.);
#9953=ADVANCED_FACE('',(#717),#9527,.F.);
#9954=ADVANCED_FACE('',(#718),#9528,.F.);
#9955=ADVANCED_FACE('',(#719),#9529,.F.);
#9956=ADVANCED_FACE('',(#720),#9530,.F.);
#9957=ADVANCED_FACE('',(#721),#9531,.F.);
#9958=ADVANCED_FACE('',(#722),#9532,.F.);
#9959=ADVANCED_FACE('',(#723),#9533,.F.);
#9960=ADVANCED_FACE('',(#724),#9534,.F.);
#9961=ADVANCED_FACE('',(#725),#9535,.F.);
#9962=ADVANCED_FACE('',(#726),#9536,.F.);
#9963=ADVANCED_FACE('',(#727),#9537,.F.);
#9964=ADVANCED_FACE('',(#728),#9538,.F.);
#9965=ADVANCED_FACE('',(#729),#9539,.F.);
#9966=ADVANCED_FACE('',(#730),#9540,.F.);
#9967=ADVANCED_FACE('',(#731),#9541,.F.);
#9968=ADVANCED_FACE('',(#732),#9542,.F.);
#9969=ADVANCED_FACE('',(#733),#9543,.F.);
#9970=ADVANCED_FACE('',(#734),#9544,.F.);
#9971=ADVANCED_FACE('',(#735),#9545,.F.);
#9972=ADVANCED_FACE('',(#736),#9546,.F.);
#9973=ADVANCED_FACE('',(#737),#9547,.F.);
#9974=ADVANCED_FACE('',(#738),#9548,.F.);
#9975=ADVANCED_FACE('',(#739),#9549,.F.);
#9976=ADVANCED_FACE('',(#740),#9550,.F.);
#9977=ADVANCED_FACE('',(#741),#9551,.F.);
#9978=ADVANCED_FACE('',(#742),#9552,.F.);
#9979=ADVANCED_FACE('',(#743),#9553,.F.);
#9980=ADVANCED_FACE('',(#744),#9554,.F.);
#9981=ADVANCED_FACE('',(#745),#9555,.F.);
#9982=ADVANCED_FACE('',(#746),#9556,.F.);
#9983=ADVANCED_FACE('',(#747),#9557,.F.);
#9984=ADVANCED_FACE('',(#748),#9558,.F.);
#9985=ADVANCED_FACE('',(#749),#9559,.F.);
#9986=ADVANCED_FACE('',(#750),#9560,.F.);
#9987=ADVANCED_FACE('',(#751),#9561,.F.);
#9988=ADVANCED_FACE('',(#752),#9562,.F.);
#9989=ADVANCED_FACE('',(#753),#9563,.F.);
#9990=ADVANCED_FACE('',(#754),#9564,.F.);
#9991=ADVANCED_FACE('',(#755),#9565,.F.);
#9992=ADVANCED_FACE('',(#756),#9566,.F.);
#9993=ADVANCED_FACE('',(#757),#9567,.F.);
#9994=ADVANCED_FACE('',(#758),#9568,.F.);
#9995=ADVANCED_FACE('',(#759),#9569,.F.);
#9996=ADVANCED_FACE('',(#760),#9570,.F.);
#9997=ADVANCED_FACE('',(#761),#9571,.F.);
#9998=ADVANCED_FACE('',(#762),#9572,.F.);
#9999=ADVANCED_FACE('',(#763),#9573,.F.);
#10000=ADVANCED_FACE('',(#764),#9574,.F.);
#10001=ADVANCED_FACE('',(#765),#9575,.F.);
#10002=ADVANCED_FACE('',(#766),#9576,.F.);
#10003=ADVANCED_FACE('',(#767),#9577,.F.);
#10004=ADVANCED_FACE('',(#768),#9578,.F.);
#10005=ADVANCED_FACE('',(#769),#9579,.F.);
#10006=ADVANCED_FACE('',(#770),#9580,.F.);
#10007=ADVANCED_FACE('',(#771),#9581,.F.);
#10008=ADVANCED_FACE('',(#772),#9582,.F.);
#10009=ADVANCED_FACE('',(#773),#9583,.F.);
#10010=ADVANCED_FACE('',(#774),#9584,.F.);
#10011=ADVANCED_FACE('',(#775),#9585,.F.);
#10012=ADVANCED_FACE('',(#776),#9586,.F.);
#10013=ADVANCED_FACE('',(#777),#9587,.F.);
#10014=ADVANCED_FACE('',(#778),#9588,.F.);
#10015=ADVANCED_FACE('',(#779),#9589,.F.);
#10016=ADVANCED_FACE('',(#780),#9590,.F.);
#10017=ADVANCED_FACE('',(#781),#9591,.F.);
#10018=ADVANCED_FACE('',(#782),#9592,.F.);
#10019=ADVANCED_FACE('',(#783),#9593,.F.);
#10020=ADVANCED_FACE('',(#784),#9594,.F.);
#10021=ADVANCED_FACE('',(#785),#9595,.F.);
#10022=ADVANCED_FACE('',(#786),#9596,.F.);
#10023=ADVANCED_FACE('',(#787),#9597,.F.);
#10024=ADVANCED_FACE('',(#788),#9598,.F.);
#10025=ADVANCED_FACE('',(#789),#9599,.F.);
#10026=ADVANCED_FACE('',(#790),#9600,.F.);
#10027=ADVANCED_FACE('',(#791),#9601,.F.);
#10028=ADVANCED_FACE('',(#792),#9602,.F.);
#10029=ADVANCED_FACE('',(#793),#9603,.F.);
#10030=ADVANCED_FACE('',(#794),#9604,.F.);
#10031=ADVANCED_FACE('',(#795),#9605,.F.);
#10032=ADVANCED_FACE('',(#796),#9606,.F.);
#10033=ADVANCED_FACE('',(#797),#9607,.F.);
#10034=ADVANCED_FACE('',(#798),#9608,.F.);
#10035=ADVANCED_FACE('',(#799),#9609,.F.);
#10036=ADVANCED_FACE('',(#800),#9610,.F.);
#10037=ADVANCED_FACE('',(#801),#9611,.F.);
#10038=ADVANCED_FACE('',(#802),#9612,.F.);
#10039=ADVANCED_FACE('',(#803),#9613,.F.);
#10040=ADVANCED_FACE('',(#804),#9614,.F.);
#10041=ADVANCED_FACE('',(#805),#9615,.F.);
#10042=ADVANCED_FACE('',(#806),#9616,.F.);
#10043=ADVANCED_FACE('',(#807),#9617,.F.);
#10044=ADVANCED_FACE('',(#808),#9618,.F.);
#10045=ADVANCED_FACE('',(#809),#9619,.F.);
#10046=ADVANCED_FACE('',(#810),#9620,.F.);
#10047=ADVANCED_FACE('',(#811),#9621,.F.);
#10048=ADVANCED_FACE('',(#812),#9622,.F.);
#10049=ADVANCED_FACE('',(#813),#9623,.F.);
#10050=ADVANCED_FACE('',(#814),#9624,.F.);
#10051=ADVANCED_FACE('',(#815),#9625,.F.);
#10052=ADVANCED_FACE('',(#816),#9626,.F.);
#10053=ADVANCED_FACE('',(#817),#9627,.F.);
#10054=ADVANCED_FACE('',(#818),#9628,.F.);
#10055=ADVANCED_FACE('',(#819),#9629,.F.);
#10056=ADVANCED_FACE('',(#820),#9630,.F.);
#10057=ADVANCED_FACE('',(#821),#9631,.F.);
#10058=ADVANCED_FACE('',(#822),#9632,.F.);
#10059=ADVANCED_FACE('',(#823),#9633,.F.);
#10060=ADVANCED_FACE('',(#824),#9634,.F.);
#10061=ADVANCED_FACE('',(#825),#9635,.F.);
#10062=ADVANCED_FACE('',(#826),#9636,.F.);
#10063=ADVANCED_FACE('',(#827),#9637,.F.);
#10064=ADVANCED_FACE('',(#828),#9638,.F.);
#10065=ADVANCED_FACE('',(#829),#9639,.F.);
#10066=ADVANCED_FACE('',(#830),#9640,.F.);
#10067=ADVANCED_FACE('',(#831),#9641,.F.);
#10068=ADVANCED_FACE('',(#832),#9642,.F.);
#10069=ADVANCED_FACE('',(#833),#9643,.F.);
#10070=ADVANCED_FACE('',(#834),#9644,.F.);
#10071=ADVANCED_FACE('',(#835),#9645,.F.);
#10072=ADVANCED_FACE('',(#836),#9646,.F.);
#10073=ADVANCED_FACE('',(#837),#9647,.F.);
#10074=ADVANCED_FACE('',(#838),#9648,.F.);
#10075=ADVANCED_FACE('',(#839),#9649,.F.);
#10076=ADVANCED_FACE('',(#840),#9650,.F.);
#10077=ADVANCED_FACE('',(#841),#9651,.F.);
#10078=ADVANCED_FACE('',(#842),#9652,.F.);
#10079=ADVANCED_FACE('',(#843),#9653,.F.);
#10080=ADVANCED_FACE('',(#844),#9654,.F.);
#10081=ADVANCED_FACE('',(#845),#9655,.F.);
#10082=ADVANCED_FACE('',(#846),#9656,.F.);
#10083=ADVANCED_FACE('',(#847),#9657,.F.);
#10084=ADVANCED_FACE('',(#848),#9658,.F.);
#10085=ADVANCED_FACE('',(#849),#9659,.F.);
#10086=ADVANCED_FACE('',(#850),#9660,.F.);
#10087=ADVANCED_FACE('',(#851),#9661,.F.);
#10088=ADVANCED_FACE('',(#852),#9662,.F.);
#10089=ADVANCED_FACE('',(#853),#9663,.F.);
#10090=ADVANCED_FACE('',(#854),#9664,.F.);
#10091=ADVANCED_FACE('',(#855),#9665,.F.);
#10092=ADVANCED_FACE('',(#856),#9666,.F.);
#10093=ADVANCED_FACE('',(#857),#9667,.F.);
#10094=ADVANCED_FACE('',(#858),#9668,.F.);
#10095=ADVANCED_FACE('',(#859),#9669,.F.);
#10096=ADVANCED_FACE('',(#860),#9670,.F.);
#10097=ADVANCED_FACE('',(#861),#9671,.F.);
#10098=ADVANCED_FACE('',(#862),#9672,.F.);
#10099=ADVANCED_FACE('',(#863),#9673,.F.);
#10100=ADVANCED_FACE('',(#864),#579,.F.);
#10101=ADVANCED_FACE('',(#865),#580,.F.);
#10102=ADVANCED_FACE('',(#866,#353),#487,.F.);
#10103=ADVANCED_FACE('',(#867),#9674,.F.);
#10104=ADVANCED_FACE('',(#868),#9675,.T.);
#10105=ADVANCED_FACE('',(#869,#354,#355,#356,#357,#358),#488,.F.);
#10106=ADVANCED_FACE('',(#870),#489,.F.);
#10107=ADVANCED_FACE('',(#871),#9676,.F.);
#10108=ADVANCED_FACE('',(#872),#581,.F.);
#10109=ADVANCED_FACE('',(#873),#582,.F.);
#10110=ADVANCED_FACE('',(#874),#9677,.F.);
#10111=ADVANCED_FACE('',(#875),#490,.F.);
#10112=ADVANCED_FACE('',(#876),#9678,.F.);
#10113=ADVANCED_FACE('',(#877),#583,.F.);
#10114=ADVANCED_FACE('',(#878),#584,.F.);
#10115=ADVANCED_FACE('',(#879),#9679,.F.);
#10116=ADVANCED_FACE('',(#880),#491,.F.);
#10117=ADVANCED_FACE('',(#881),#492,.F.);
#10118=ADVANCED_FACE('',(#882),#493,.F.);
#10119=ADVANCED_FACE('',(#883),#9680,.F.);
#10120=ADVANCED_FACE('',(#884),#585,.F.);
#10121=ADVANCED_FACE('',(#885),#586,.F.);
#10122=ADVANCED_FACE('',(#886),#9681,.F.);
#10123=ADVANCED_FACE('',(#887),#494,.F.);
#10124=ADVANCED_FACE('',(#888),#495,.F.);
#10125=ADVANCED_FACE('',(#889),#496,.F.);
#10126=ADVANCED_FACE('',(#890),#9682,.F.);
#10127=ADVANCED_FACE('',(#891),#587,.F.);
#10128=ADVANCED_FACE('',(#892),#588,.F.);
#10129=ADVANCED_FACE('',(#893),#9683,.F.);
#10130=ADVANCED_FACE('',(#894),#9684,.F.);
#10131=ADVANCED_FACE('',(#895),#497,.F.);
#10132=ADVANCED_FACE('',(#896),#498,.F.);
#10133=ADVANCED_FACE('',(#897),#9685,.F.);
#10134=ADVANCED_FACE('',(#898),#499,.T.);
#10135=ADVANCED_FACE('',(#899),#9686,.F.);
#10136=ADVANCED_FACE('',(#900),#589,.F.);
#10137=ADVANCED_FACE('',(#901),#590,.F.);
#10138=ADVANCED_FACE('',(#902),#9687,.F.);
#10139=ADVANCED_FACE('',(#903),#500,.T.);
#10140=ADVANCED_FACE('',(#904),#9688,.F.);
#10141=ADVANCED_FACE('',(#905),#591,.F.);
#10142=ADVANCED_FACE('',(#906),#592,.F.);
#10143=ADVANCED_FACE('',(#907),#9689,.F.);
#10144=ADVANCED_FACE('',(#908),#501,.T.);
#10145=ADVANCED_FACE('',(#909),#9690,.F.);
#10146=ADVANCED_FACE('',(#910),#593,.F.);
#10147=ADVANCED_FACE('',(#911),#594,.F.);
#10148=ADVANCED_FACE('',(#912),#9691,.F.);
#10149=ADVANCED_FACE('',(#913),#502,.T.);
#10150=ADVANCED_FACE('',(#914),#9692,.F.);
#10151=ADVANCED_FACE('',(#915),#595,.F.);
#10152=ADVANCED_FACE('',(#916),#596,.F.);
#10153=ADVANCED_FACE('',(#917),#9693,.F.);
#10154=ADVANCED_FACE('',(#918),#503,.F.);
#10155=ADVANCED_FACE('',(#919),#504,.F.);
#10156=ADVANCED_FACE('',(#920),#505,.F.);
#10157=ADVANCED_FACE('',(#921),#506,.F.);
#10158=ADVANCED_FACE('',(#922),#9694,.F.);
#10159=ADVANCED_FACE('',(#923),#9695,.F.);
#10160=ADVANCED_FACE('',(#924),#9696,.F.);
#10161=ADVANCED_FACE('',(#925),#9697,.F.);
#10162=ADVANCED_FACE('',(#926),#9698,.F.);
#10163=ADVANCED_FACE('',(#927),#9699,.F.);
#10164=ADVANCED_FACE('',(#928),#9700,.F.);
#10165=ADVANCED_FACE('',(#929),#9701,.F.);
#10166=ADVANCED_FACE('',(#930),#9702,.F.);
#10167=ADVANCED_FACE('',(#931),#9703,.F.);
#10168=ADVANCED_FACE('',(#932),#9704,.F.);
#10169=ADVANCED_FACE('',(#933),#9705,.F.);
#10170=ADVANCED_FACE('',(#934),#9706,.F.);
#10171=ADVANCED_FACE('',(#935),#9707,.F.);
#10172=ADVANCED_FACE('',(#936),#9708,.F.);
#10173=ADVANCED_FACE('',(#937),#9709,.F.);
#10174=ADVANCED_FACE('',(#938),#9710,.F.);
#10175=ADVANCED_FACE('',(#939),#9711,.F.);
#10176=ADVANCED_FACE('',(#940),#507,.F.);
#10177=ADVANCED_FACE('',(#941,#359,#360,#361,#362,#363,#364,#365,#366,#367,
#368,#369,#370,#371,#372,#373,#374,#375,#376),#508,.F.);
#10178=ADVANCED_FACE('',(#942),#509,.F.);
#10179=ADVANCED_FACE('',(#943),#510,.F.);
#10180=ADVANCED_FACE('',(#944,#377),#511,.F.);
#10181=ADVANCED_FACE('',(#945),#512,.T.);
#10182=ADVANCED_FACE('',(#946,#378,#379,#380,#381,#382,#383,#384,#385,#386,
#387,#388,#389,#390,#391,#392,#393,#394,#395),#513,.T.);
#10183=ADVANCED_FACE('',(#947),#514,.T.);
#10184=ADVANCED_FACE('',(#948),#515,.T.);
#10185=ADVANCED_FACE('',(#949,#396,#397,#398,#399,#400),#516,.T.);
#10186=ADVANCED_FACE('',(#950),#9712,.F.);
#10187=ADVANCED_FACE('',(#951),#9713,.F.);
#10188=ADVANCED_FACE('',(#952),#9714,.F.);
#10189=ADVANCED_FACE('',(#953),#9715,.F.);
#10190=ADVANCED_FACE('',(#954),#517,.T.);
#10191=ADVANCED_FACE('',(#955),#518,.T.);
#10192=ADVANCED_FACE('',(#956),#519,.T.);
#10193=ADVANCED_FACE('',(#957),#520,.T.);
#10194=ADVANCED_FACE('',(#958,#401,#402,#403,#404),#521,.T.);
#10195=ADVANCED_FACE('',(#959,#405,#406,#407,#408),#522,.F.);
#10196=ADVANCED_FACE('',(#960),#9716,.F.);
#10197=ADVANCED_FACE('',(#961),#9717,.F.);
#10198=ADVANCED_FACE('',(#962),#9718,.F.);
#10199=ADVANCED_FACE('',(#963),#9719,.F.);
#10200=ADVANCED_FACE('',(#964),#523,.F.);
#10201=ADVANCED_FACE('',(#965),#524,.F.);
#10202=ADVANCED_FACE('',(#966),#525,.F.);
#10203=ADVANCED_FACE('',(#967),#526,.F.);
#10204=ADVANCED_FACE('',(#968),#527,.T.);
#10205=ADVANCED_FACE('',(#969),#528,.T.);
#10206=ADVANCED_FACE('',(#970),#529,.T.);
#10207=ADVANCED_FACE('',(#971),#530,.T.);
#10208=ADVANCED_FACE('',(#972,#409,#410,#411,#412,#413),#531,.T.);
#10209=ADVANCED_FACE('',(#973,#414,#415,#416,#417,#418),#532,.F.);
#10210=ADVANCED_FACE('',(#974),#9720,.F.);
#10211=ADVANCED_FACE('',(#975),#9721,.T.);
#10212=ADVANCED_FACE('',(#976,#419),#533,.T.);
#10213=ADVANCED_FACE('',(#977,#420),#534,.F.);
#10214=ADVANCED_FACE('',(#978),#9722,.F.);
#10215=ADVANCED_FACE('',(#979),#9723,.F.);
#10216=ADVANCED_FACE('',(#980),#9724,.F.);
#10217=ADVANCED_FACE('',(#981),#9725,.F.);
#10218=ADVANCED_FACE('',(#982),#9726,.F.);
#10219=ADVANCED_FACE('',(#983),#9727,.F.);
#10220=ADVANCED_FACE('',(#984),#9728,.F.);
#10221=ADVANCED_FACE('',(#985),#9729,.F.);
#10222=ADVANCED_FACE('',(#986),#9730,.F.);
#10223=ADVANCED_FACE('',(#987),#9731,.F.);
#10224=ADVANCED_FACE('',(#988),#9732,.F.);
#10225=ADVANCED_FACE('',(#989),#9733,.F.);
#10226=ADVANCED_FACE('',(#990),#9734,.F.);
#10227=ADVANCED_FACE('',(#991),#9735,.F.);
#10228=ADVANCED_FACE('',(#992),#9736,.F.);
#10229=ADVANCED_FACE('',(#993),#9737,.F.);
#10230=ADVANCED_FACE('',(#994),#9738,.F.);
#10231=ADVANCED_FACE('',(#995),#9739,.F.);
#10232=ADVANCED_FACE('',(#996),#535,.T.);
#10233=ADVANCED_FACE('',(#997),#536,.T.);
#10234=ADVANCED_FACE('',(#998),#537,.T.);
#10235=ADVANCED_FACE('',(#999),#538,.T.);
#10236=ADVANCED_FACE('',(#1000,#421,#422,#423,#424,#425,#426,#427,#428,
#429,#430,#431,#432,#433,#434,#435,#436,#437,#438),#539,.T.);
#10237=ADVANCED_FACE('',(#1001,#439,#440,#441,#442,#443,#444,#445,#446,
#447,#448,#449,#450,#451,#452,#453,#454,#455,#456),#540,.F.);
#10238=ADVANCED_FACE('',(#1002),#9740,.F.);
#10239=ADVANCED_FACE('',(#1003),#9741,.F.);
#10240=ADVANCED_FACE('',(#1004),#9742,.F.);
#10241=ADVANCED_FACE('',(#1005),#9743,.F.);
#10242=ADVANCED_FACE('',(#1006),#9744,.F.);
#10243=ADVANCED_FACE('',(#1007),#9745,.F.);
#10244=ADVANCED_FACE('',(#1008),#9746,.F.);
#10245=ADVANCED_FACE('',(#1009),#541,.T.);
#10246=ADVANCED_FACE('',(#1010),#542,.T.);
#10247=ADVANCED_FACE('',(#1011),#543,.T.);
#10248=ADVANCED_FACE('',(#1012),#544,.T.);
#10249=ADVANCED_FACE('',(#1013,#457,#458,#459,#460,#461,#462,#463),#545,
 .T.);
#10250=ADVANCED_FACE('',(#1014,#464,#465,#466,#467,#468,#469,#470),#546,
 .F.);
#10251=ADVANCED_FACE('',(#1015),#9747,.T.);
#10252=ADVANCED_FACE('',(#1016),#9748,.T.);
#10253=ADVANCED_FACE('',(#1017),#9749,.T.);
#10254=ADVANCED_FACE('',(#1018),#9750,.T.);
#10255=ADVANCED_FACE('',(#1019),#9751,.T.);
#10256=ADVANCED_FACE('',(#1020),#9752,.T.);
#10257=ADVANCED_FACE('',(#1021),#9753,.T.);
#10258=ADVANCED_FACE('',(#1022),#9754,.T.);
#10259=ADVANCED_FACE('',(#1023),#9755,.T.);
#10260=ADVANCED_FACE('',(#1024),#9756,.T.);
#10261=ADVANCED_FACE('',(#1025),#9757,.T.);
#10262=ADVANCED_FACE('',(#1026),#9758,.T.);
#10263=ADVANCED_FACE('',(#1027),#9759,.T.);
#10264=ADVANCED_FACE('',(#1028),#9760,.T.);
#10265=ADVANCED_FACE('',(#1029),#9761,.T.);
#10266=ADVANCED_FACE('',(#1030),#9762,.T.);
#10267=ADVANCED_FACE('',(#1031),#9763,.T.);
#10268=ADVANCED_FACE('',(#1032),#9764,.T.);
#10269=ADVANCED_FACE('',(#1033),#9765,.T.);
#10270=ADVANCED_FACE('',(#1034),#9766,.T.);
#10271=ADVANCED_FACE('',(#1035),#9767,.T.);
#10272=ADVANCED_FACE('',(#1036),#9768,.T.);
#10273=ADVANCED_FACE('',(#1037),#9769,.T.);
#10274=ADVANCED_FACE('',(#1038),#9770,.T.);
#10275=ADVANCED_FACE('',(#1039),#9771,.T.);
#10276=ADVANCED_FACE('',(#1040),#9772,.T.);
#10277=ADVANCED_FACE('',(#1041),#9773,.T.);
#10278=ADVANCED_FACE('',(#1042),#9774,.T.);
#10279=ADVANCED_FACE('',(#1043),#9775,.T.);
#10280=ADVANCED_FACE('',(#1044),#9776,.T.);
#10281=ADVANCED_FACE('',(#1045),#9777,.T.);
#10282=ADVANCED_FACE('',(#1046),#9778,.T.);
#10283=ADVANCED_FACE('',(#1047),#311,.T.);
#10284=ADVANCED_FACE('',(#1048),#597,.F.);
#10285=ADVANCED_FACE('',(#1049),#9779,.T.);
#10286=ADVANCED_FACE('',(#1050),#598,.F.);
#10287=ADVANCED_FACE('',(#1051),#9780,.T.);
#10288=ADVANCED_FACE('',(#1052),#547,.F.);
#10289=ADVANCED_FACE('',(#1053),#548,.F.);
#10290=ADVANCED_FACE('',(#1054),#549,.F.);
#10291=ADVANCED_FACE('',(#1055),#550,.F.);
#10292=ADVANCED_FACE('',(#1056),#551,.F.);
#10293=ADVANCED_FACE('',(#1057),#552,.F.);
#10294=ADVANCED_FACE('',(#1058),#553,.F.);
#10295=ADVANCED_FACE('',(#1059,#471),#554,.T.);
#10296=ADVANCED_FACE('',(#1060),#9781,.T.);
#10297=ADVANCED_FACE('',(#1061,#472),#555,.F.);
#10298=ADVANCED_FACE('',(#1062),#556,.T.);
#10299=ADVANCED_FACE('',(#1063),#9782,.T.);
#10300=ADVANCED_FACE('',(#1064),#9783,.T.);
#10301=ADVANCED_FACE('',(#1065),#9784,.T.);
#10302=ADVANCED_FACE('',(#1066),#9785,.T.);
#10303=ADVANCED_FACE('',(#1067),#9786,.T.);
#10304=ADVANCED_FACE('',(#1068),#9787,.T.);
#10305=ADVANCED_FACE('',(#1069),#9788,.T.);
#10306=ADVANCED_FACE('',(#1070),#9789,.T.);
#10307=ADVANCED_FACE('',(#1071),#9790,.T.);
#10308=ADVANCED_FACE('',(#1072),#9791,.T.);
#10309=ADVANCED_FACE('',(#1073),#9792,.T.);
#10310=ADVANCED_FACE('',(#1074),#9793,.T.);
#10311=ADVANCED_FACE('',(#1075),#9794,.T.);
#10312=ADVANCED_FACE('',(#1076),#9795,.T.);
#10313=ADVANCED_FACE('',(#1077),#9796,.T.);
#10314=ADVANCED_FACE('',(#1078),#9797,.T.);
#10315=ADVANCED_FACE('',(#1079),#9798,.T.);
#10316=ADVANCED_FACE('',(#1080),#9799,.T.);
#10317=ADVANCED_FACE('',(#1081),#9800,.T.);
#10318=ADVANCED_FACE('',(#1082),#9801,.T.);
#10319=ADVANCED_FACE('',(#1083),#9802,.T.);
#10320=ADVANCED_FACE('',(#1084),#9803,.T.);
#10321=ADVANCED_FACE('',(#1085),#312,.T.);
#10322=ADVANCED_FACE('',(#1086),#599,.F.);
#10323=ADVANCED_FACE('',(#1087),#9804,.T.);
#10324=ADVANCED_FACE('',(#1088),#600,.F.);
#10325=ADVANCED_FACE('',(#1089),#9805,.T.);
#10326=ADVANCED_FACE('',(#1090),#557,.F.);
#10327=ADVANCED_FACE('',(#1091),#558,.F.);
#10328=ADVANCED_FACE('',(#1092),#559,.F.);
#10329=ADVANCED_FACE('',(#1093),#560,.F.);
#10330=ADVANCED_FACE('',(#1094),#561,.F.);
#10331=ADVANCED_FACE('',(#1095),#562,.F.);
#10332=ADVANCED_FACE('',(#1096),#563,.F.);
#10333=ADVANCED_FACE('',(#1097,#473),#564,.T.);
#10334=ADVANCED_FACE('',(#1098),#9806,.T.);
#10335=ADVANCED_FACE('',(#1099,#474),#565,.F.);
#10336=ADVANCED_FACE('',(#1100),#566,.T.);
#10337=ADVANCED_FACE('',(#1101),#9807,.T.);
#10338=ADVANCED_FACE('',(#1102),#9808,.T.);
#10339=ADVANCED_FACE('',(#1103),#9809,.T.);
#10340=ADVANCED_FACE('',(#1104),#9810,.T.);
#10341=ADVANCED_FACE('',(#1105),#9811,.T.);
#10342=ADVANCED_FACE('',(#1106),#9812,.T.);
#10343=ADVANCED_FACE('',(#1107),#9813,.T.);
#10344=ADVANCED_FACE('',(#1108),#9814,.T.);
#10345=ADVANCED_FACE('',(#1109),#9815,.T.);
#10346=ADVANCED_FACE('',(#1110),#9816,.T.);
#10347=ADVANCED_FACE('',(#1111),#9817,.T.);
#10348=ADVANCED_FACE('',(#1112),#9818,.T.);
#10349=ADVANCED_FACE('',(#1113),#9819,.T.);
#10350=ADVANCED_FACE('',(#1114),#9820,.T.);
#10351=ADVANCED_FACE('',(#1115),#9821,.T.);
#10352=ADVANCED_FACE('',(#1116),#9822,.T.);
#10353=ADVANCED_FACE('',(#1117),#9823,.T.);
#10354=ADVANCED_FACE('',(#1118),#9824,.T.);
#10355=ADVANCED_FACE('',(#1119),#9825,.T.);
#10356=ADVANCED_FACE('',(#1120),#601,.F.);
#10357=ADVANCED_FACE('',(#1121),#9826,.T.);
#10358=ADVANCED_FACE('',(#1122),#602,.F.);
#10359=ADVANCED_FACE('',(#1123),#9827,.T.);
#10360=ADVANCED_FACE('',(#1124,#475),#567,.T.);
#10361=ADVANCED_FACE('',(#1125,#476),#568,.F.);
#10362=ADVANCED_FACE('',(#1126),#9828,.T.);
#10363=ADVANCED_FACE('',(#1127),#9829,.T.);
#10364=ADVANCED_FACE('',(#1128,#477),#569,.T.);
#10365=ADVANCED_FACE('',(#1129,#478),#570,.F.);
#10366=ADVANCED_FACE('',(#1130),#9830,.T.);
#10367=ADVANCED_FACE('',(#1131),#9831,.T.);
#10368=ADVANCED_FACE('',(#1132,#479),#571,.T.);
#10369=ADVANCED_FACE('',(#1133,#480),#572,.F.);
#10370=ADVANCED_FACE('',(#1134),#9832,.T.);
#10371=ADVANCED_FACE('',(#1135),#9833,.T.);
#10372=ADVANCED_FACE('',(#1136),#9834,.T.);
#10373=ADVANCED_FACE('',(#1137,#481),#573,.F.);
#10374=ADVANCED_FACE('',(#1138,#482),#574,.T.);
#10375=ADVANCED_FACE('',(#1139),#9835,.T.);
#10376=ADVANCED_FACE('',(#1140,#483),#575,.F.);
#10377=ADVANCED_FACE('',(#1141),#9836,.F.);
#10378=ADVANCED_FACE('',(#1142,#484),#576,.T.);
#10379=ADVANCED_FACE('',(#1143),#9837,.F.);
#10380=ADVANCED_FACE('',(#1144),#9838,.T.);
#10381=ADVANCED_FACE('',(#1145,#485),#577,.T.);
#10382=ADVANCED_FACE('',(#1146,#486),#578,.F.);
#10383=CLOSED_SHELL('',(#9839,#9840,#9841,#9842,#9843,#9844,#9845,#9846,
#9847,#9848,#9849,#9850,#9851,#9852,#9853,#9854,#9855,#9856,#9857,#9858,
#9859,#9860,#9861,#9862,#9863,#9864,#9865,#9866,#9867,#9868,#9869,#9870,
#9871,#9872,#9873,#9874,#9875,#9876,#9877,#9878,#9879,#9880,#9881,#9882,
#9883,#9884,#9885,#9886,#9887,#9888,#9889,#9890,#9891,#9892,#9893,#9894,
#9895,#9896,#9897,#9898,#9899,#9900,#9901,#9902,#9903,#9904,#9905,#9906,
#9907,#9908,#9909,#9910,#9911,#9912,#9913,#9914,#9915,#9916,#9917,#9918,
#9919,#9920,#9921,#9922,#9923,#9924,#9925,#9926,#9927,#9928,#9929,#9930,
#9931,#9932,#9933,#9934,#9935,#9936,#9937,#9938,#9939,#9940,#9941,#9942,
#9943,#9944,#9945,#9946,#9947,#9948,#9949,#9950,#9951,#9952,#9953,#9954,
#9955,#9956,#9957,#9958,#9959,#9960,#9961,#9962,#9963,#9964,#9965,#9966,
#9967,#9968,#9969,#9970,#9971,#9972,#9973,#9974,#9975,#9976,#9977,#9978,
#9979,#9980,#9981,#9982,#9983,#9984,#9985,#9986,#9987,#9988,#9989,#9990,
#9991,#9992,#9993,#9994,#9995,#9996,#9997,#9998,#9999,#10000,#10001,#10002,
#10003,#10004,#10005,#10006,#10007,#10008,#10009,#10010,#10011,#10012,#10013,
#10014,#10015,#10016,#10017,#10018,#10019,#10020,#10021,#10022,#10023,#10024,
#10025,#10026,#10027,#10028,#10029,#10030,#10031,#10032,#10033,#10034,#10035,
#10036,#10037,#10038,#10039,#10040,#10041,#10042,#10043,#10044,#10045,#10046,
#10047,#10048,#10049,#10050,#10051,#10052,#10053,#10054,#10055,#10056,#10057,
#10058,#10059,#10060,#10061,#10062,#10063,#10064,#10065,#10066,#10067,#10068,
#10069,#10070,#10071,#10072,#10073,#10074,#10075,#10076,#10077,#10078,#10079,
#10080,#10081,#10082,#10083,#10084,#10085,#10086,#10087,#10088,#10089,#10090,
#10091,#10092,#10093,#10094,#10095,#10096,#10097,#10098,#10099,#10100,#10101,
#10102,#10103,#10104,#10105,#10106,#10107,#10108,#10109,#10110,#10111,#10112,
#10113,#10114,#10115,#10116,#10117,#10118,#10119,#10120,#10121,#10122,#10123,
#10124,#10125,#10126,#10127,#10128,#10129,#10130,#10131,#10132,#10133,#10134,
#10135,#10136,#10137,#10138,#10139,#10140,#10141,#10142,#10143,#10144,#10145,
#10146,#10147,#10148,#10149,#10150,#10151,#10152,#10153,#10154,#10155,#10156,
#10157,#10158,#10159,#10160,#10161,#10162,#10163,#10164,#10165,#10166,#10167,
#10168,#10169,#10170,#10171,#10172,#10173,#10174,#10175,#10176,#10177,#10178,
#10179,#10180,#10181,#10182,#10183,#10184,#10185));
#10384=CLOSED_SHELL('',(#10186,#10187,#10188,#10189,#10190,#10191,#10192,
#10193,#10194,#10195));
#10385=CLOSED_SHELL('',(#10196,#10197,#10198,#10199,#10200,#10201,#10202,
#10203,#10204,#10205,#10206,#10207,#10208,#10209));
#10386=CLOSED_SHELL('',(#10210,#10211,#10212,#10213));
#10387=CLOSED_SHELL('',(#10214,#10215,#10216,#10217,#10218,#10219,#10220,
#10221,#10222,#10223,#10224,#10225,#10226,#10227,#10228,#10229,#10230,#10231,
#10232,#10233,#10234,#10235,#10236,#10237));
#10388=CLOSED_SHELL('',(#10238,#10239,#10240,#10241,#10242,#10243,#10244,
#10245,#10246,#10247,#10248,#10249,#10250));
#10389=CLOSED_SHELL('',(#10251,#10252,#10253,#10254,#10255,#10256,#10257,
#10258,#10259,#10260,#10261,#10262,#10263,#10264,#10265,#10266,#10267,#10268,
#10269,#10270,#10271,#10272,#10273,#10274,#10275,#10276,#10277,#10278,#10279,
#10280,#10281,#10282,#10283,#10284,#10285,#10286,#10287,#10288,#10289,#10290,
#10291,#10292,#10293,#10294,#10295,#10296,#10297,#10298));
#10390=CLOSED_SHELL('',(#10299,#10300,#10301,#10302,#10303,#10304,#10305,
#10306,#10307,#10308,#10309,#10310,#10311,#10312,#10313,#10314,#10315,#10316,
#10317,#10318,#10319,#10320,#10321,#10322,#10323,#10324,#10325,#10326,#10327,
#10328,#10329,#10330,#10331,#10332,#10333,#10334,#10335,#10336));
#10391=CLOSED_SHELL('',(#10337,#10338,#10339,#10340,#10341,#10342,#10343,
#10344,#10345,#10346,#10347,#10348,#10349,#10350,#10351,#10352,#10353,#10354,
#10355,#10356,#10357,#10358,#10359,#10360,#10361,#10362,#10363,#10364,#10365,
#10366,#10367,#10368,#10369,#10370,#10371,#10372,#10373,#10374,#10375,#10376,
#10377,#10378));
#10392=CLOSED_SHELL('',(#10379,#10380,#10381,#10382));
#10393=DERIVED_UNIT_ELEMENT(#10413,1.);
#10394=DERIVED_UNIT_ELEMENT(#42622,-3.);
#10395=DERIVED_UNIT_ELEMENT(#10413,1.);
#10396=DERIVED_UNIT_ELEMENT(#42622,-3.);
#10397=DERIVED_UNIT_ELEMENT(#10413,1.);
#10398=DERIVED_UNIT_ELEMENT(#42622,-3.);
#10399=DERIVED_UNIT_ELEMENT(#10413,1.);
#10400=DERIVED_UNIT_ELEMENT(#42622,-3.);
#10401=DERIVED_UNIT_ELEMENT(#10413,1.);
#10402=DERIVED_UNIT_ELEMENT(#42622,-3.);
#10403=DERIVED_UNIT_ELEMENT(#10413,1.);
#10404=DERIVED_UNIT_ELEMENT(#42622,-3.);
#10405=DERIVED_UNIT_ELEMENT(#10413,1.);
#10406=DERIVED_UNIT_ELEMENT(#42622,-3.);
#10407=DERIVED_UNIT_ELEMENT(#10413,1.);
#10408=DERIVED_UNIT_ELEMENT(#42622,-3.);
#10409=DERIVED_UNIT_ELEMENT(#10413,1.);
#10410=DERIVED_UNIT_ELEMENT(#42622,-3.);
#10411=DERIVED_UNIT_ELEMENT(#10413,1.);
#10412=DERIVED_UNIT_ELEMENT(#42622,-3.);
#10413=(
MASS_UNIT()
NAMED_UNIT(*)
SI_UNIT(.KILO.,.GRAM.)
);
#10414=DERIVED_UNIT((#10393,#10394));
#10415=DERIVED_UNIT((#10395,#10396));
#10416=DERIVED_UNIT((#10397,#10398));
#10417=DERIVED_UNIT((#10399,#10400));
#10418=DERIVED_UNIT((#10401,#10402));
#10419=DERIVED_UNIT((#10403,#10404));
#10420=DERIVED_UNIT((#10405,#10406));
#10421=DERIVED_UNIT((#10407,#10408));
#10422=DERIVED_UNIT((#10409,#10410));
#10423=DERIVED_UNIT((#10411,#10412));
#10424=MEASURE_REPRESENTATION_ITEM('density measure',
POSITIVE_RATIO_MEASURE(7850.),#10414);
#10425=MEASURE_REPRESENTATION_ITEM('density measure',
POSITIVE_RATIO_MEASURE(7850.),#10415);
#10426=MEASURE_REPRESENTATION_ITEM('density measure',
POSITIVE_RATIO_MEASURE(1250.),#10416);
#10427=MEASURE_REPRESENTATION_ITEM('density measure',
POSITIVE_RATIO_MEASURE(8940.),#10417);
#10428=MEASURE_REPRESENTATION_ITEM('density measure',
POSITIVE_RATIO_MEASURE(7850.),#10418);
#10429=MEASURE_REPRESENTATION_ITEM('density measure',
POSITIVE_RATIO_MEASURE(7850.),#10419);
#10430=MEASURE_REPRESENTATION_ITEM('density measure',
POSITIVE_RATIO_MEASURE(7850.),#10420);
#10431=MEASURE_REPRESENTATION_ITEM('density measure',
POSITIVE_RATIO_MEASURE(7850.),#10421);
#10432=MEASURE_REPRESENTATION_ITEM('density measure',
POSITIVE_RATIO_MEASURE(7850.),#10422);
#10433=MEASURE_REPRESENTATION_ITEM('density measure',
POSITIVE_RATIO_MEASURE(1250.),#10423);
#10434=PROPERTY_DEFINITION_REPRESENTATION(#10484,#10454);
#10435=PROPERTY_DEFINITION_REPRESENTATION(#10485,#10455);
#10436=PROPERTY_DEFINITION_REPRESENTATION(#10486,#10456);
#10437=PROPERTY_DEFINITION_REPRESENTATION(#10487,#10457);
#10438=PROPERTY_DEFINITION_REPRESENTATION(#10488,#10458);
#10439=PROPERTY_DEFINITION_REPRESENTATION(#10489,#10459);
#10440=PROPERTY_DEFINITION_REPRESENTATION(#10490,#10460);
#10441=PROPERTY_DEFINITION_REPRESENTATION(#10491,#10461);
#10442=PROPERTY_DEFINITION_REPRESENTATION(#10492,#10462);
#10443=PROPERTY_DEFINITION_REPRESENTATION(#10493,#10463);
#10444=PROPERTY_DEFINITION_REPRESENTATION(#10494,#10464);
#10445=PROPERTY_DEFINITION_REPRESENTATION(#10495,#10465);
#10446=PROPERTY_DEFINITION_REPRESENTATION(#10496,#10466);
#10447=PROPERTY_DEFINITION_REPRESENTATION(#10497,#10467);
#10448=PROPERTY_DEFINITION_REPRESENTATION(#10498,#10468);
#10449=PROPERTY_DEFINITION_REPRESENTATION(#10499,#10469);
#10450=PROPERTY_DEFINITION_REPRESENTATION(#10500,#10470);
#10451=PROPERTY_DEFINITION_REPRESENTATION(#10501,#10471);
#10452=PROPERTY_DEFINITION_REPRESENTATION(#10502,#10472);
#10453=PROPERTY_DEFINITION_REPRESENTATION(#10503,#10473);
#10454=REPRESENTATION('material name',(#10474),#42610);
#10455=REPRESENTATION('density',(#10424),#42610);
#10456=REPRESENTATION('material name',(#10475),#42611);
#10457=REPRESENTATION('density',(#10425),#42611);
#10458=REPRESENTATION('material name',(#10476),#42612);
#10459=REPRESENTATION('density',(#10426),#42612);
#10460=REPRESENTATION('material name',(#10477),#42613);
#10461=REPRESENTATION('density',(#10427),#42613);
#10462=REPRESENTATION('material name',(#10478),#42614);
#10463=REPRESENTATION('density',(#10428),#42614);
#10464=REPRESENTATION('material name',(#10479),#42615);
#10465=REPRESENTATION('density',(#10429),#42615);
#10466=REPRESENTATION('material name',(#10480),#42616);
#10467=REPRESENTATION('density',(#10430),#42616);
#10468=REPRESENTATION('material name',(#10481),#42617);
#10469=REPRESENTATION('density',(#10431),#42617);
#10470=REPRESENTATION('material name',(#10482),#42618);
#10471=REPRESENTATION('density',(#10432),#42618);
#10472=REPRESENTATION('material name',(#10483),#42619);
#10473=REPRESENTATION('density',(#10433),#42619);
#10474=DESCRIPTIVE_REPRESENTATION_ITEM('Steel','Steel');
#10475=DESCRIPTIVE_REPRESENTATION_ITEM('Steel','Steel');
#10476=DESCRIPTIVE_REPRESENTATION_ITEM('Rubber, Silicone',
'Rubber, Silicone');
#10477=DESCRIPTIVE_REPRESENTATION_ITEM('Copper','Copper');
#10478=DESCRIPTIVE_REPRESENTATION_ITEM('Steel','Steel');
#10479=DESCRIPTIVE_REPRESENTATION_ITEM('Steel','Steel');
#10480=DESCRIPTIVE_REPRESENTATION_ITEM('Steel','Steel');
#10481=DESCRIPTIVE_REPRESENTATION_ITEM('Steel','Steel');
#10482=DESCRIPTIVE_REPRESENTATION_ITEM('Steel','Steel');
#10483=DESCRIPTIVE_REPRESENTATION_ITEM('Rubber, Silicone',
'Rubber, Silicone');
#10484=PROPERTY_DEFINITION('material property','material name',#42735);
#10485=PROPERTY_DEFINITION('material property','density of part',#42735);
#10486=PROPERTY_DEFINITION('material property','material name',#42736);
#10487=PROPERTY_DEFINITION('material property','density of part',#42736);
#10488=PROPERTY_DEFINITION('material property','material name',#42737);
#10489=PROPERTY_DEFINITION('material property','density of part',#42737);
#10490=PROPERTY_DEFINITION('material property','material name',#42738);
#10491=PROPERTY_DEFINITION('material property','density of part',#42738);
#10492=PROPERTY_DEFINITION('material property','material name',#42739);
#10493=PROPERTY_DEFINITION('material property','density of part',#42739);
#10494=PROPERTY_DEFINITION('material property','material name',#42740);
#10495=PROPERTY_DEFINITION('material property','density of part',#42740);
#10496=PROPERTY_DEFINITION('material property','material name',#42741);
#10497=PROPERTY_DEFINITION('material property','density of part',#42741);
#10498=PROPERTY_DEFINITION('material property','material name',#42742);
#10499=PROPERTY_DEFINITION('material property','density of part',#42742);
#10500=PROPERTY_DEFINITION('material property','material name',#42743);
#10501=PROPERTY_DEFINITION('material property','density of part',#42743);
#10502=PROPERTY_DEFINITION('material property','material name',#42744);
#10503=PROPERTY_DEFINITION('material property','density of part',#42744);
#10504=AXIS2_PLACEMENT_3D('',#13448,#11306,#11307);
#10505=AXIS2_PLACEMENT_3D('',#13449,#11308,#11309);
#10506=AXIS2_PLACEMENT_3D('',#13450,#11310,#11311);
#10507=AXIS2_PLACEMENT_3D('',#13475,#11313,#11314);
#10508=AXIS2_PLACEMENT_3D('',#13483,#11316,#11317);
#10509=AXIS2_PLACEMENT_3D('',#13506,#11318,#11319);
#10510=AXIS2_PLACEMENT_3D('',#13557,#11321,#11322);
#10511=AXIS2_PLACEMENT_3D('',#13605,#11324,#11325);
#10512=AXIS2_PLACEMENT_3D('',#13656,#11327,#11328);
#10513=AXIS2_PLACEMENT_3D('',#13707,#11330,#11331);
#10514=AXIS2_PLACEMENT_3D('',#13755,#11333,#11334);
#10515=AXIS2_PLACEMENT_3D('',#13803,#11336,#11337);
#10516=AXIS2_PLACEMENT_3D('',#13854,#11339,#11340);
#10517=AXIS2_PLACEMENT_3D('',#13902,#11342,#11343);
#10518=AXIS2_PLACEMENT_3D('',#13950,#11345,#11346);
#10519=AXIS2_PLACEMENT_3D('',#14001,#11348,#11349);
#10520=AXIS2_PLACEMENT_3D('',#14052,#11351,#11352);
#10521=AXIS2_PLACEMENT_3D('',#14100,#11354,#11355);
#10522=AXIS2_PLACEMENT_3D('',#14151,#11357,#11358);
#10523=AXIS2_PLACEMENT_3D('',#14170,#11360,#11361);
#10524=AXIS2_PLACEMENT_3D('',#14190,#11362,#11363);
#10525=AXIS2_PLACEMENT_3D('',#14202,#11365,#11366);
#10526=AXIS2_PLACEMENT_3D('',#14210,#11367,#11368);
#10527=AXIS2_PLACEMENT_3D('',#14234,#11370,#11371);
#10528=AXIS2_PLACEMENT_3D('',#14259,#11373,#11374);
#10529=AXIS2_PLACEMENT_3D('',#14284,#11376,#11377);
#10530=AXIS2_PLACEMENT_3D('',#14308,#11379,#11380);
#10531=AXIS2_PLACEMENT_3D('',#14333,#11382,#11383);
#10532=AXIS2_PLACEMENT_3D('',#14357,#11385,#11386);
#10533=AXIS2_PLACEMENT_3D('',#14382,#11388,#11389);
#10534=AXIS2_PLACEMENT_3D('',#14407,#11391,#11392);
#10535=AXIS2_PLACEMENT_3D('',#14431,#11394,#11395);
#10536=AXIS2_PLACEMENT_3D('',#14456,#11397,#11398);
#10537=AXIS2_PLACEMENT_3D('',#14480,#11400,#11401);
#10538=AXIS2_PLACEMENT_3D('',#14505,#11403,#11404);
#10539=AXIS2_PLACEMENT_3D('',#14530,#11406,#11407);
#10540=AXIS2_PLACEMENT_3D('',#14554,#11409,#11410);
#10541=AXIS2_PLACEMENT_3D('',#14565,#11412,#11413);
#10542=AXIS2_PLACEMENT_3D('',#14571,#11414,#11415);
#10543=AXIS2_PLACEMENT_3D('',#14596,#11417,#11418);
#10544=AXIS2_PLACEMENT_3D('',#14604,#11420,#11421);
#10545=AXIS2_PLACEMENT_3D('',#14627,#11422,#11423);
#10546=AXIS2_PLACEMENT_3D('',#14678,#11425,#11426);
#10547=AXIS2_PLACEMENT_3D('',#14726,#11428,#11429);
#10548=AXIS2_PLACEMENT_3D('',#14777,#11431,#11432);
#10549=AXIS2_PLACEMENT_3D('',#14828,#11434,#11435);
#10550=AXIS2_PLACEMENT_3D('',#14876,#11437,#11438);
#10551=AXIS2_PLACEMENT_3D('',#14924,#11440,#11441);
#10552=AXIS2_PLACEMENT_3D('',#14975,#11443,#11444);
#10553=AXIS2_PLACEMENT_3D('',#15023,#11446,#11447);
#10554=AXIS2_PLACEMENT_3D('',#15071,#11449,#11450);
#10555=AXIS2_PLACEMENT_3D('',#15122,#11452,#11453);
#10556=AXIS2_PLACEMENT_3D('',#15173,#11455,#11456);
#10557=AXIS2_PLACEMENT_3D('',#15221,#11458,#11459);
#10558=AXIS2_PLACEMENT_3D('',#15272,#11461,#11462);
#10559=AXIS2_PLACEMENT_3D('',#15291,#11464,#11465);
#10560=AXIS2_PLACEMENT_3D('',#15311,#11466,#11467);
#10561=AXIS2_PLACEMENT_3D('',#15323,#11469,#11470);
#10562=AXIS2_PLACEMENT_3D('',#15331,#11471,#11472);
#10563=AXIS2_PLACEMENT_3D('',#15355,#11474,#11475);
#10564=AXIS2_PLACEMENT_3D('',#15380,#11477,#11478);
#10565=AXIS2_PLACEMENT_3D('',#15405,#11480,#11481);
#10566=AXIS2_PLACEMENT_3D('',#15429,#11483,#11484);
#10567=AXIS2_PLACEMENT_3D('',#15454,#11486,#11487);
#10568=AXIS2_PLACEMENT_3D('',#15478,#11489,#11490);
#10569=AXIS2_PLACEMENT_3D('',#15503,#11492,#11493);
#10570=AXIS2_PLACEMENT_3D('',#15528,#11495,#11496);
#10571=AXIS2_PLACEMENT_3D('',#15552,#11498,#11499);
#10572=AXIS2_PLACEMENT_3D('',#15577,#11501,#11502);
#10573=AXIS2_PLACEMENT_3D('',#15601,#11504,#11505);
#10574=AXIS2_PLACEMENT_3D('',#15626,#11507,#11508);
#10575=AXIS2_PLACEMENT_3D('',#15651,#11510,#11511);
#10576=AXIS2_PLACEMENT_3D('',#15675,#11513,#11514);
#10577=AXIS2_PLACEMENT_3D('',#15686,#11516,#11517);
#10578=AXIS2_PLACEMENT_3D('',#15692,#11518,#11519);
#10579=AXIS2_PLACEMENT_3D('',#15717,#11521,#11522);
#10580=AXIS2_PLACEMENT_3D('',#15725,#11524,#11525);
#10581=AXIS2_PLACEMENT_3D('',#15748,#11526,#11527);
#10582=AXIS2_PLACEMENT_3D('',#15799,#11529,#11530);
#10583=AXIS2_PLACEMENT_3D('',#15847,#11532,#11533);
#10584=AXIS2_PLACEMENT_3D('',#15898,#11535,#11536);
#10585=AXIS2_PLACEMENT_3D('',#15949,#11538,#11539);
#10586=AXIS2_PLACEMENT_3D('',#15997,#11541,#11542);
#10587=AXIS2_PLACEMENT_3D('',#16045,#11544,#11545);
#10588=AXIS2_PLACEMENT_3D('',#16096,#11547,#11548);
#10589=AXIS2_PLACEMENT_3D('',#16144,#11550,#11551);
#10590=AXIS2_PLACEMENT_3D('',#16192,#11553,#11554);
#10591=AXIS2_PLACEMENT_3D('',#16243,#11556,#11557);
#10592=AXIS2_PLACEMENT_3D('',#16294,#11559,#11560);
#10593=AXIS2_PLACEMENT_3D('',#16342,#11562,#11563);
#10594=AXIS2_PLACEMENT_3D('',#16393,#11565,#11566);
#10595=AXIS2_PLACEMENT_3D('',#16412,#11568,#11569);
#10596=AXIS2_PLACEMENT_3D('',#16432,#11570,#11571);
#10597=AXIS2_PLACEMENT_3D('',#16444,#11573,#11574);
#10598=AXIS2_PLACEMENT_3D('',#16452,#11575,#11576);
#10599=AXIS2_PLACEMENT_3D('',#16476,#11578,#11579);
#10600=AXIS2_PLACEMENT_3D('',#16501,#11581,#11582);
#10601=AXIS2_PLACEMENT_3D('',#16526,#11584,#11585);
#10602=AXIS2_PLACEMENT_3D('',#16550,#11587,#11588);
#10603=AXIS2_PLACEMENT_3D('',#16575,#11590,#11591);
#10604=AXIS2_PLACEMENT_3D('',#16599,#11593,#11594);
#10605=AXIS2_PLACEMENT_3D('',#16624,#11596,#11597);
#10606=AXIS2_PLACEMENT_3D('',#16649,#11599,#11600);
#10607=AXIS2_PLACEMENT_3D('',#16673,#11602,#11603);
#10608=AXIS2_PLACEMENT_3D('',#16698,#11605,#11606);
#10609=AXIS2_PLACEMENT_3D('',#16722,#11608,#11609);
#10610=AXIS2_PLACEMENT_3D('',#16747,#11611,#11612);
#10611=AXIS2_PLACEMENT_3D('',#16772,#11614,#11615);
#10612=AXIS2_PLACEMENT_3D('',#16796,#11617,#11618);
#10613=AXIS2_PLACEMENT_3D('',#16807,#11620,#11621);
#10614=AXIS2_PLACEMENT_3D('',#16813,#11622,#11623);
#10615=AXIS2_PLACEMENT_3D('',#16838,#11625,#11626);
#10616=AXIS2_PLACEMENT_3D('',#16846,#11628,#11629);
#10617=AXIS2_PLACEMENT_3D('',#16869,#11630,#11631);
#10618=AXIS2_PLACEMENT_3D('',#16920,#11633,#11634);
#10619=AXIS2_PLACEMENT_3D('',#16968,#11636,#11637);
#10620=AXIS2_PLACEMENT_3D('',#17019,#11639,#11640);
#10621=AXIS2_PLACEMENT_3D('',#17070,#11642,#11643);
#10622=AXIS2_PLACEMENT_3D('',#17118,#11645,#11646);
#10623=AXIS2_PLACEMENT_3D('',#17166,#11648,#11649);
#10624=AXIS2_PLACEMENT_3D('',#17217,#11651,#11652);
#10625=AXIS2_PLACEMENT_3D('',#17265,#11654,#11655);
#10626=AXIS2_PLACEMENT_3D('',#17313,#11657,#11658);
#10627=AXIS2_PLACEMENT_3D('',#17364,#11660,#11661);
#10628=AXIS2_PLACEMENT_3D('',#17415,#11663,#11664);
#10629=AXIS2_PLACEMENT_3D('',#17463,#11666,#11667);
#10630=AXIS2_PLACEMENT_3D('',#17514,#11669,#11670);
#10631=AXIS2_PLACEMENT_3D('',#17533,#11672,#11673);
#10632=AXIS2_PLACEMENT_3D('',#17553,#11674,#11675);
#10633=AXIS2_PLACEMENT_3D('',#17565,#11677,#11678);
#10634=AXIS2_PLACEMENT_3D('',#17573,#11679,#11680);
#10635=AXIS2_PLACEMENT_3D('',#17597,#11682,#11683);
#10636=AXIS2_PLACEMENT_3D('',#17622,#11685,#11686);
#10637=AXIS2_PLACEMENT_3D('',#17647,#11688,#11689);
#10638=AXIS2_PLACEMENT_3D('',#17671,#11691,#11692);
#10639=AXIS2_PLACEMENT_3D('',#17696,#11694,#11695);
#10640=AXIS2_PLACEMENT_3D('',#17720,#11697,#11698);
#10641=AXIS2_PLACEMENT_3D('',#17745,#11700,#11701);
#10642=AXIS2_PLACEMENT_3D('',#17770,#11703,#11704);
#10643=AXIS2_PLACEMENT_3D('',#17794,#11706,#11707);
#10644=AXIS2_PLACEMENT_3D('',#17819,#11709,#11710);
#10645=AXIS2_PLACEMENT_3D('',#17843,#11712,#11713);
#10646=AXIS2_PLACEMENT_3D('',#17868,#11715,#11716);
#10647=AXIS2_PLACEMENT_3D('',#17893,#11718,#11719);
#10648=AXIS2_PLACEMENT_3D('',#17917,#11721,#11722);
#10649=AXIS2_PLACEMENT_3D('',#17928,#11724,#11725);
#10650=AXIS2_PLACEMENT_3D('',#17934,#11726,#11727);
#10651=AXIS2_PLACEMENT_3D('',#17944,#11729,#11730);
#10652=AXIS2_PLACEMENT_3D('',#17966,#11731,#11732);
#10653=AXIS2_PLACEMENT_3D('',#17977,#11733,#11734);
#10654=AXIS2_PLACEMENT_3D('',#18028,#11736,#11737);
#10655=AXIS2_PLACEMENT_3D('',#18079,#11739,#11740);
#10656=AXIS2_PLACEMENT_3D('',#18127,#11742,#11743);
#10657=AXIS2_PLACEMENT_3D('',#18178,#11745,#11746);
#10658=AXIS2_PLACEMENT_3D('',#18229,#11748,#11749);
#10659=AXIS2_PLACEMENT_3D('',#18277,#11751,#11752);
#10660=AXIS2_PLACEMENT_3D('',#18328,#11754,#11755);
#10661=AXIS2_PLACEMENT_3D('',#18379,#11757,#11758);
#10662=AXIS2_PLACEMENT_3D('',#18427,#11760,#11761);
#10663=AXIS2_PLACEMENT_3D('',#18478,#11763,#11764);
#10664=AXIS2_PLACEMENT_3D('',#18529,#11766,#11767);
#10665=AXIS2_PLACEMENT_3D('',#18577,#11769,#11770);
#10666=AXIS2_PLACEMENT_3D('',#18628,#11772,#11773);
#10667=AXIS2_PLACEMENT_3D('',#18647,#11775,#11776);
#10668=AXIS2_PLACEMENT_3D('',#18667,#11777,#11778);
#10669=AXIS2_PLACEMENT_3D('',#18677,#11780,#11781);
#10670=AXIS2_PLACEMENT_3D('',#18699,#11782,#11783);
#10671=AXIS2_PLACEMENT_3D('',#18710,#11784,#11785);
#10672=AXIS2_PLACEMENT_3D('',#18761,#11787,#11788);
#10673=AXIS2_PLACEMENT_3D('',#18812,#11790,#11791);
#10674=AXIS2_PLACEMENT_3D('',#18860,#11793,#11794);
#10675=AXIS2_PLACEMENT_3D('',#18911,#11796,#11797);
#10676=AXIS2_PLACEMENT_3D('',#18962,#11799,#11800);
#10677=AXIS2_PLACEMENT_3D('',#19010,#11802,#11803);
#10678=AXIS2_PLACEMENT_3D('',#19061,#11805,#11806);
#10679=AXIS2_PLACEMENT_3D('',#19112,#11808,#11809);
#10680=AXIS2_PLACEMENT_3D('',#19160,#11811,#11812);
#10681=AXIS2_PLACEMENT_3D('',#19211,#11814,#11815);
#10682=AXIS2_PLACEMENT_3D('',#19262,#11817,#11818);
#10683=AXIS2_PLACEMENT_3D('',#19310,#11820,#11821);
#10684=AXIS2_PLACEMENT_3D('',#19361,#11823,#11824);
#10685=AXIS2_PLACEMENT_3D('',#19380,#11826,#11827);
#10686=AXIS2_PLACEMENT_3D('',#19400,#11828,#11829);
#10687=AXIS2_PLACEMENT_3D('',#19414,#11831,#11832);
#10688=AXIS2_PLACEMENT_3D('',#19424,#11833,#11834);
#10689=AXIS2_PLACEMENT_3D('',#19448,#11836,#11837);
#10690=AXIS2_PLACEMENT_3D('',#19473,#11839,#11840);
#10691=AXIS2_PLACEMENT_3D('',#19498,#11842,#11843);
#10692=AXIS2_PLACEMENT_3D('',#19522,#11845,#11846);
#10693=AXIS2_PLACEMENT_3D('',#19547,#11848,#11849);
#10694=AXIS2_PLACEMENT_3D('',#19572,#11851,#11852);
#10695=AXIS2_PLACEMENT_3D('',#19596,#11854,#11855);
#10696=AXIS2_PLACEMENT_3D('',#19621,#11857,#11858);
#10697=AXIS2_PLACEMENT_3D('',#19646,#11860,#11861);
#10698=AXIS2_PLACEMENT_3D('',#19670,#11863,#11864);
#10699=AXIS2_PLACEMENT_3D('',#19695,#11866,#11867);
#10700=AXIS2_PLACEMENT_3D('',#19720,#11869,#11870);
#10701=AXIS2_PLACEMENT_3D('',#19744,#11872,#11873);
#10702=AXIS2_PLACEMENT_3D('',#19755,#11875,#11876);
#10703=AXIS2_PLACEMENT_3D('',#19761,#11877,#11878);
#10704=AXIS2_PLACEMENT_3D('',#19775,#11880,#11881);
#10705=AXIS2_PLACEMENT_3D('',#19785,#11882,#11883);
#10706=AXIS2_PLACEMENT_3D('',#19809,#11885,#11886);
#10707=AXIS2_PLACEMENT_3D('',#19834,#11888,#11889);
#10708=AXIS2_PLACEMENT_3D('',#19859,#11891,#11892);
#10709=AXIS2_PLACEMENT_3D('',#19883,#11894,#11895);
#10710=AXIS2_PLACEMENT_3D('',#19908,#11897,#11898);
#10711=AXIS2_PLACEMENT_3D('',#19933,#11900,#11901);
#10712=AXIS2_PLACEMENT_3D('',#19957,#11903,#11904);
#10713=AXIS2_PLACEMENT_3D('',#19982,#11906,#11907);
#10714=AXIS2_PLACEMENT_3D('',#20007,#11909,#11910);
#10715=AXIS2_PLACEMENT_3D('',#20031,#11912,#11913);
#10716=AXIS2_PLACEMENT_3D('',#20056,#11915,#11916);
#10717=AXIS2_PLACEMENT_3D('',#20081,#11918,#11919);
#10718=AXIS2_PLACEMENT_3D('',#20105,#11921,#11922);
#10719=AXIS2_PLACEMENT_3D('',#20116,#11924,#11925);
#10720=AXIS2_PLACEMENT_3D('',#20122,#11926,#11927);
#10721=AXIS2_PLACEMENT_3D('',#20132,#11929,#11930);
#10722=AXIS2_PLACEMENT_3D('',#20135,#11932,#11933);
#10723=AXIS2_PLACEMENT_3D('',#20137,#11934,#11935);
#10724=AXIS2_PLACEMENT_3D('',#20148,#11936,#11937);
#10725=AXIS2_PLACEMENT_3D('',#20199,#11939,#11940);
#10726=AXIS2_PLACEMENT_3D('',#20250,#11942,#11943);
#10727=AXIS2_PLACEMENT_3D('',#20298,#11945,#11946);
#10728=AXIS2_PLACEMENT_3D('',#20349,#11948,#11949);
#10729=AXIS2_PLACEMENT_3D('',#20400,#11951,#11952);
#10730=AXIS2_PLACEMENT_3D('',#20448,#11954,#11955);
#10731=AXIS2_PLACEMENT_3D('',#20499,#11957,#11958);
#10732=AXIS2_PLACEMENT_3D('',#20550,#11960,#11961);
#10733=AXIS2_PLACEMENT_3D('',#20598,#11963,#11964);
#10734=AXIS2_PLACEMENT_3D('',#20649,#11966,#11967);
#10735=AXIS2_PLACEMENT_3D('',#20700,#11969,#11970);
#10736=AXIS2_PLACEMENT_3D('',#20748,#11972,#11973);
#10737=AXIS2_PLACEMENT_3D('',#20799,#11975,#11976);
#10738=AXIS2_PLACEMENT_3D('',#20818,#11978,#11979);
#10739=AXIS2_PLACEMENT_3D('',#20838,#11980,#11981);
#10740=AXIS2_PLACEMENT_3D('',#20852,#11983,#11984);
#10741=AXIS2_PLACEMENT_3D('',#20862,#11985,#11986);
#10742=AXIS2_PLACEMENT_3D('',#20886,#11988,#11989);
#10743=AXIS2_PLACEMENT_3D('',#20911,#11991,#11992);
#10744=AXIS2_PLACEMENT_3D('',#20936,#11994,#11995);
#10745=AXIS2_PLACEMENT_3D('',#20960,#11997,#11998);
#10746=AXIS2_PLACEMENT_3D('',#20985,#12000,#12001);
#10747=AXIS2_PLACEMENT_3D('',#21010,#12003,#12004);
#10748=AXIS2_PLACEMENT_3D('',#21034,#12006,#12007);
#10749=AXIS2_PLACEMENT_3D('',#21059,#12009,#12010);
#10750=AXIS2_PLACEMENT_3D('',#21084,#12012,#12013);
#10751=AXIS2_PLACEMENT_3D('',#21108,#12015,#12016);
#10752=AXIS2_PLACEMENT_3D('',#21133,#12018,#12019);
#10753=AXIS2_PLACEMENT_3D('',#21158,#12021,#12022);
#10754=AXIS2_PLACEMENT_3D('',#21182,#12024,#12025);
#10755=AXIS2_PLACEMENT_3D('',#21193,#12027,#12028);
#10756=AXIS2_PLACEMENT_3D('',#21199,#12029,#12030);
#10757=AXIS2_PLACEMENT_3D('',#21209,#12032,#12033);
#10758=AXIS2_PLACEMENT_3D('',#21212,#12035,#12036);
#10759=AXIS2_PLACEMENT_3D('',#21214,#12037,#12038);
#10760=AXIS2_PLACEMENT_3D('',#21225,#12039,#12040);
#10761=AXIS2_PLACEMENT_3D('',#21276,#12042,#12043);
#10762=AXIS2_PLACEMENT_3D('',#21327,#12045,#12046);
#10763=AXIS2_PLACEMENT_3D('',#21375,#12048,#12049);
#10764=AXIS2_PLACEMENT_3D('',#21426,#12051,#12052);
#10765=AXIS2_PLACEMENT_3D('',#21477,#12054,#12055);
#10766=AXIS2_PLACEMENT_3D('',#21525,#12057,#12058);
#10767=AXIS2_PLACEMENT_3D('',#21576,#12060,#12061);
#10768=AXIS2_PLACEMENT_3D('',#21627,#12063,#12064);
#10769=AXIS2_PLACEMENT_3D('',#21675,#12066,#12067);
#10770=AXIS2_PLACEMENT_3D('',#21726,#12069,#12070);
#10771=AXIS2_PLACEMENT_3D('',#21777,#12072,#12073);
#10772=AXIS2_PLACEMENT_3D('',#21825,#12075,#12076);
#10773=AXIS2_PLACEMENT_3D('',#21876,#12078,#12079);
#10774=AXIS2_PLACEMENT_3D('',#21895,#12081,#12082);
#10775=AXIS2_PLACEMENT_3D('',#21915,#12083,#12084);
#10776=AXIS2_PLACEMENT_3D('',#21929,#12086,#12087);
#10777=AXIS2_PLACEMENT_3D('',#21939,#12088,#12089);
#10778=AXIS2_PLACEMENT_3D('',#21963,#12091,#12092);
#10779=AXIS2_PLACEMENT_3D('',#21988,#12094,#12095);
#10780=AXIS2_PLACEMENT_3D('',#22013,#12097,#12098);
#10781=AXIS2_PLACEMENT_3D('',#22037,#12100,#12101);
#10782=AXIS2_PLACEMENT_3D('',#22062,#12103,#12104);
#10783=AXIS2_PLACEMENT_3D('',#22087,#12106,#12107);
#10784=AXIS2_PLACEMENT_3D('',#22111,#12109,#12110);
#10785=AXIS2_PLACEMENT_3D('',#22136,#12112,#12113);
#10786=AXIS2_PLACEMENT_3D('',#22161,#12115,#12116);
#10787=AXIS2_PLACEMENT_3D('',#22185,#12118,#12119);
#10788=AXIS2_PLACEMENT_3D('',#22210,#12121,#12122);
#10789=AXIS2_PLACEMENT_3D('',#22235,#12124,#12125);
#10790=AXIS2_PLACEMENT_3D('',#22259,#12127,#12128);
#10791=AXIS2_PLACEMENT_3D('',#22270,#12130,#12131);
#10792=AXIS2_PLACEMENT_3D('',#22276,#12132,#12133);
#10793=AXIS2_PLACEMENT_3D('',#22307,#12135,#12136);
#10794=AXIS2_PLACEMENT_3D('',#22345,#12137,#12138);
#10795=AXIS2_PLACEMENT_3D('',#22435,#12140,#12141);
#10796=AXIS2_PLACEMENT_3D('',#22522,#12143,#12144);
#10797=AXIS2_PLACEMENT_3D('',#22612,#12146,#12147);
#10798=AXIS2_PLACEMENT_3D('',#22699,#12149,#12150);
#10799=AXIS2_PLACEMENT_3D('',#22789,#12152,#12153);
#10800=AXIS2_PLACEMENT_3D('',#22876,#12155,#12156);
#10801=AXIS2_PLACEMENT_3D('',#22889,#12158,#12159);
#10802=AXIS2_PLACEMENT_3D('',#22909,#12160,#12161);
#10803=AXIS2_PLACEMENT_3D('',#22928,#12163,#12164);
#10804=AXIS2_PLACEMENT_3D('',#22943,#12165,#12166);
#10805=AXIS2_PLACEMENT_3D('',#22979,#12168,#12169);
#10806=AXIS2_PLACEMENT_3D('',#23017,#12171,#12172);
#10807=AXIS2_PLACEMENT_3D('',#23055,#12174,#12175);
#10808=AXIS2_PLACEMENT_3D('',#23092,#12177,#12178);
#10809=AXIS2_PLACEMENT_3D('',#23129,#12180,#12181);
#10810=AXIS2_PLACEMENT_3D('',#23167,#12183,#12184);
#10811=AXIS2_PLACEMENT_3D('',#23179,#12186,#12187);
#10812=AXIS2_PLACEMENT_3D('',#23187,#12188,#12189);
#10813=AXIS2_PLACEMENT_3D('',#24643,#12190,#12191);
#10814=AXIS2_PLACEMENT_3D('',#24645,#12192,#12193);
#10815=AXIS2_PLACEMENT_3D('',#24646,#12194,#12195);
#10816=AXIS2_PLACEMENT_3D('',#24647,#12196,#12197);
#10817=AXIS2_PLACEMENT_3D('',#24649,#12198,#12199);
#10818=AXIS2_PLACEMENT_3D('',#24651,#12201,#12202);
#10819=AXIS2_PLACEMENT_3D('',#25400,#12207,#12208);
#10820=AXIS2_PLACEMENT_3D('',#25589,#12209,#12210);
#10821=AXIS2_PLACEMENT_3D('',#26458,#12211,#12212);
#10822=AXIS2_PLACEMENT_3D('',#26459,#12213,#12214);
#10823=AXIS2_PLACEMENT_3D('',#26648,#12215,#12216);
#10824=AXIS2_PLACEMENT_3D('',#27517,#12217,#12218);
#10825=AXIS2_PLACEMENT_3D('',#27518,#12219,#12220);
#10826=AXIS2_PLACEMENT_3D('',#27552,#12222,#12223);
#10827=AXIS2_PLACEMENT_3D('',#27684,#12226,#12227);
#10828=AXIS2_PLACEMENT_3D('',#27685,#12228,#12229);
#10829=AXIS2_PLACEMENT_3D('',#27721,#12231,#12232);
#10830=AXIS2_PLACEMENT_3D('',#28590,#12233,#12234);
#10831=AXIS2_PLACEMENT_3D('',#28612,#12235,#12236);
#10832=AXIS2_PLACEMENT_3D('',#28646,#12238,#12239);
#10833=AXIS2_PLACEMENT_3D('',#28778,#12242,#12243);
#10834=AXIS2_PLACEMENT_3D('',#28779,#12244,#12245);
#10835=AXIS2_PLACEMENT_3D('',#28815,#12247,#12248);
#10836=AXIS2_PLACEMENT_3D('',#29684,#12249,#12250);
#10837=AXIS2_PLACEMENT_3D('',#29706,#12251,#12252);
#10838=AXIS2_PLACEMENT_3D('',#29707,#12253,#12254);
#10839=AXIS2_PLACEMENT_3D('',#29708,#12255,#12256);
#10840=AXIS2_PLACEMENT_3D('',#29709,#12257,#12258);
#10841=AXIS2_PLACEMENT_3D('',#29710,#12259,#12260);
#10842=AXIS2_PLACEMENT_3D('',#29884,#12261,#12262);
#10843=AXIS2_PLACEMENT_3D('',#30952,#12263,#12264);
#10844=AXIS2_PLACEMENT_3D('',#30953,#12265,#12266);
#10845=AXIS2_PLACEMENT_3D('',#31127,#12267,#12268);
#10846=AXIS2_PLACEMENT_3D('',#32195,#12269,#12270);
#10847=AXIS2_PLACEMENT_3D('',#32196,#12271,#12272);
#10848=AXIS2_PLACEMENT_3D('',#32370,#12273,#12274);
#10849=AXIS2_PLACEMENT_3D('',#33438,#12275,#12276);
#10850=AXIS2_PLACEMENT_3D('',#33439,#12277,#12278);
#10851=AXIS2_PLACEMENT_3D('',#33613,#12279,#12280);
#10852=AXIS2_PLACEMENT_3D('',#34681,#12281,#12282);
#10853=AXIS2_PLACEMENT_3D('',#34682,#12283,#12284);
#10854=AXIS2_PLACEMENT_3D('',#34683,#12285,#12286);
#10855=AXIS2_PLACEMENT_3D('',#34684,#12287,#12288);
#10856=AXIS2_PLACEMENT_3D('',#34685,#12289,#12290);
#10857=AXIS2_PLACEMENT_3D('',#34686,#12291,#12292);
#10858=AXIS2_PLACEMENT_3D('',#34688,#12293,#12294);
#10859=AXIS2_PLACEMENT_3D('',#34691,#12296,#12297);
#10860=AXIS2_PLACEMENT_3D('',#34692,#12298,#12299);
#10861=AXIS2_PLACEMENT_3D('',#34694,#12300,#12301);
#10862=AXIS2_PLACEMENT_3D('',#34697,#12303,#12304);
#10863=AXIS2_PLACEMENT_3D('',#34698,#12305,#12306);
#10864=AXIS2_PLACEMENT_3D('',#34700,#12307,#12308);
#10865=AXIS2_PLACEMENT_3D('',#34703,#12310,#12311);
#10866=AXIS2_PLACEMENT_3D('',#34704,#12312,#12313);
#10867=AXIS2_PLACEMENT_3D('',#34706,#12314,#12315);
#10868=AXIS2_PLACEMENT_3D('',#34709,#12317,#12318);
#10869=AXIS2_PLACEMENT_3D('',#34710,#12319,#12320);
#10870=AXIS2_PLACEMENT_3D('',#34712,#12321,#12322);
#10871=AXIS2_PLACEMENT_3D('',#34715,#12324,#12325);
#10872=AXIS2_PLACEMENT_3D('',#34716,#12326,#12327);
#10873=AXIS2_PLACEMENT_3D('',#34718,#12328,#12329);
#10874=AXIS2_PLACEMENT_3D('',#34721,#12331,#12332);
#10875=AXIS2_PLACEMENT_3D('',#34722,#12333,#12334);
#10876=AXIS2_PLACEMENT_3D('',#34724,#12335,#12336);
#10877=AXIS2_PLACEMENT_3D('',#34727,#12338,#12339);
#10878=AXIS2_PLACEMENT_3D('',#34728,#12340,#12341);
#10879=AXIS2_PLACEMENT_3D('',#34730,#12342,#12343);
#10880=AXIS2_PLACEMENT_3D('',#34733,#12345,#12346);
#10881=AXIS2_PLACEMENT_3D('',#34734,#12347,#12348);
#10882=AXIS2_PLACEMENT_3D('',#34736,#12349,#12350);
#10883=AXIS2_PLACEMENT_3D('',#34740,#12353,#12354);
#10884=AXIS2_PLACEMENT_3D('',#34741,#12355,#12356);
#10885=AXIS2_PLACEMENT_3D('',#34743,#12357,#12358);
#10886=AXIS2_PLACEMENT_3D('',#34746,#12360,#12361);
#10887=AXIS2_PLACEMENT_3D('',#34747,#12362,#12363);
#10888=AXIS2_PLACEMENT_3D('',#34749,#12364,#12365);
#10889=AXIS2_PLACEMENT_3D('',#34752,#12367,#12368);
#10890=AXIS2_PLACEMENT_3D('',#34753,#12369,#12370);
#10891=AXIS2_PLACEMENT_3D('',#34755,#12371,#12372);
#10892=AXIS2_PLACEMENT_3D('',#34758,#12374,#12375);
#10893=AXIS2_PLACEMENT_3D('',#34759,#12376,#12377);
#10894=AXIS2_PLACEMENT_3D('',#34761,#12378,#12379);
#10895=AXIS2_PLACEMENT_3D('',#34764,#12381,#12382);
#10896=AXIS2_PLACEMENT_3D('',#34765,#12383,#12384);
#10897=AXIS2_PLACEMENT_3D('',#34767,#12385,#12386);
#10898=AXIS2_PLACEMENT_3D('',#34770,#12388,#12389);
#10899=AXIS2_PLACEMENT_3D('',#34771,#12390,#12391);
#10900=AXIS2_PLACEMENT_3D('',#34773,#12392,#12393);
#10901=AXIS2_PLACEMENT_3D('',#34776,#12395,#12396);
#10902=AXIS2_PLACEMENT_3D('',#34777,#12397,#12398);
#10903=AXIS2_PLACEMENT_3D('',#34779,#12399,#12400);
#10904=AXIS2_PLACEMENT_3D('',#34782,#12402,#12403);
#10905=AXIS2_PLACEMENT_3D('',#34783,#12404,#12405);
#10906=AXIS2_PLACEMENT_3D('',#34785,#12406,#12407);
#10907=AXIS2_PLACEMENT_3D('',#34789,#12410,#12411);
#10908=AXIS2_PLACEMENT_3D('',#34790,#12412,#12413);
#10909=AXIS2_PLACEMENT_3D('',#34792,#12414,#12415);
#10910=AXIS2_PLACEMENT_3D('',#34795,#12417,#12418);
#10911=AXIS2_PLACEMENT_3D('',#34796,#12419,#12420);
#10912=AXIS2_PLACEMENT_3D('',#34805,#12425,#12426);
#10913=AXIS2_PLACEMENT_3D('',#34811,#12430,#12431);
#10914=AXIS2_PLACEMENT_3D('',#34817,#12435,#12436);
#10915=AXIS2_PLACEMENT_3D('',#34820,#12439,#12440);
#10916=AXIS2_PLACEMENT_3D('',#34821,#12441,#12442);
#10917=AXIS2_PLACEMENT_3D('',#34827,#12446,#12447);
#10918=AXIS2_PLACEMENT_3D('',#34831,#12450,#12451);
#10919=AXIS2_PLACEMENT_3D('',#34835,#12454,#12455);
#10920=AXIS2_PLACEMENT_3D('',#34837,#12457,#12458);
#10921=AXIS2_PLACEMENT_3D('',#34838,#12459,#12460);
#10922=AXIS2_PLACEMENT_3D('',#34839,#12461,#12462);
#10923=AXIS2_PLACEMENT_3D('',#34841,#12463,#12464);
#10924=AXIS2_PLACEMENT_3D('',#34844,#12466,#12467);
#10925=AXIS2_PLACEMENT_3D('',#34845,#12468,#12469);
#10926=AXIS2_PLACEMENT_3D('',#34847,#12470,#12471);
#10927=AXIS2_PLACEMENT_3D('',#34850,#12473,#12474);
#10928=AXIS2_PLACEMENT_3D('',#34851,#12475,#12476);
#10929=AXIS2_PLACEMENT_3D('',#34853,#12477,#12478);
#10930=AXIS2_PLACEMENT_3D('',#34856,#12480,#12481);
#10931=AXIS2_PLACEMENT_3D('',#34857,#12482,#12483);
#10932=AXIS2_PLACEMENT_3D('',#34859,#12484,#12485);
#10933=AXIS2_PLACEMENT_3D('',#34862,#12487,#12488);
#10934=AXIS2_PLACEMENT_3D('',#34863,#12489,#12490);
#10935=AXIS2_PLACEMENT_3D('',#34872,#12495,#12496);
#10936=AXIS2_PLACEMENT_3D('',#34878,#12500,#12501);
#10937=AXIS2_PLACEMENT_3D('',#34884,#12505,#12506);
#10938=AXIS2_PLACEMENT_3D('',#34887,#12509,#12510);
#10939=AXIS2_PLACEMENT_3D('',#34888,#12511,#12512);
#10940=AXIS2_PLACEMENT_3D('',#34889,#12513,#12514);
#10941=AXIS2_PLACEMENT_3D('',#34890,#12515,#12516);
#10942=AXIS2_PLACEMENT_3D('',#34892,#12517,#12518);
#10943=AXIS2_PLACEMENT_3D('',#34895,#12520,#12521);
#10944=AXIS2_PLACEMENT_3D('',#34896,#12522,#12523);
#10945=AXIS2_PLACEMENT_3D('',#34898,#12524,#12525);
#10946=AXIS2_PLACEMENT_3D('',#34901,#12527,#12528);
#10947=AXIS2_PLACEMENT_3D('',#34902,#12529,#12530);
#10948=AXIS2_PLACEMENT_3D('',#34904,#12531,#12532);
#10949=AXIS2_PLACEMENT_3D('',#34907,#12534,#12535);
#10950=AXIS2_PLACEMENT_3D('',#34908,#12536,#12537);
#10951=AXIS2_PLACEMENT_3D('',#34910,#12538,#12539);
#10952=AXIS2_PLACEMENT_3D('',#34913,#12541,#12542);
#10953=AXIS2_PLACEMENT_3D('',#34914,#12543,#12544);
#10954=AXIS2_PLACEMENT_3D('',#34923,#12549,#12550);
#10955=AXIS2_PLACEMENT_3D('',#34929,#12554,#12555);
#10956=AXIS2_PLACEMENT_3D('',#34935,#12559,#12560);
#10957=AXIS2_PLACEMENT_3D('',#34938,#12563,#12564);
#10958=AXIS2_PLACEMENT_3D('',#34947,#12569,#12570);
#10959=AXIS2_PLACEMENT_3D('',#34953,#12574,#12575);
#10960=AXIS2_PLACEMENT_3D('',#34959,#12579,#12580);
#10961=AXIS2_PLACEMENT_3D('',#34962,#12583,#12584);
#10962=AXIS2_PLACEMENT_3D('',#34963,#12585,#12586);
#10963=AXIS2_PLACEMENT_3D('',#34964,#12587,#12588);
#10964=AXIS2_PLACEMENT_3D('',#34965,#12589,#12590);
#10965=AXIS2_PLACEMENT_3D('',#34967,#12591,#12592);
#10966=AXIS2_PLACEMENT_3D('',#34970,#12594,#12595);
#10967=AXIS2_PLACEMENT_3D('',#34971,#12596,#12597);
#10968=AXIS2_PLACEMENT_3D('',#34973,#12598,#12599);
#10969=AXIS2_PLACEMENT_3D('',#34976,#12601,#12602);
#10970=AXIS2_PLACEMENT_3D('',#34977,#12603,#12604);
#10971=AXIS2_PLACEMENT_3D('',#34978,#12605,#12606);
#10972=AXIS2_PLACEMENT_3D('',#34979,#12607,#12608);
#10973=AXIS2_PLACEMENT_3D('',#34980,#12609,#12610);
#10974=AXIS2_PLACEMENT_3D('',#34982,#12611,#12612);
#10975=AXIS2_PLACEMENT_3D('',#34985,#12614,#12615);
#10976=AXIS2_PLACEMENT_3D('',#34986,#12616,#12617);
#10977=AXIS2_PLACEMENT_3D('',#34988,#12618,#12619);
#10978=AXIS2_PLACEMENT_3D('',#34991,#12621,#12622);
#10979=AXIS2_PLACEMENT_3D('',#34992,#12623,#12624);
#10980=AXIS2_PLACEMENT_3D('',#34994,#12625,#12626);
#10981=AXIS2_PLACEMENT_3D('',#34997,#12628,#12629);
#10982=AXIS2_PLACEMENT_3D('',#34998,#12630,#12631);
#10983=AXIS2_PLACEMENT_3D('',#35000,#12632,#12633);
#10984=AXIS2_PLACEMENT_3D('',#35003,#12635,#12636);
#10985=AXIS2_PLACEMENT_3D('',#35004,#12637,#12638);
#10986=AXIS2_PLACEMENT_3D('',#35006,#12639,#12640);
#10987=AXIS2_PLACEMENT_3D('',#35009,#12642,#12643);
#10988=AXIS2_PLACEMENT_3D('',#35010,#12644,#12645);
#10989=AXIS2_PLACEMENT_3D('',#35012,#12646,#12647);
#10990=AXIS2_PLACEMENT_3D('',#35015,#12649,#12650);
#10991=AXIS2_PLACEMENT_3D('',#35016,#12651,#12652);
#10992=AXIS2_PLACEMENT_3D('',#35018,#12653,#12654);
#10993=AXIS2_PLACEMENT_3D('',#35021,#12656,#12657);
#10994=AXIS2_PLACEMENT_3D('',#35022,#12658,#12659);
#10995=AXIS2_PLACEMENT_3D('',#35024,#12660,#12661);
#10996=AXIS2_PLACEMENT_3D('',#35027,#12663,#12664);
#10997=AXIS2_PLACEMENT_3D('',#35028,#12665,#12666);
#10998=AXIS2_PLACEMENT_3D('',#35030,#12667,#12668);
#10999=AXIS2_PLACEMENT_3D('',#35033,#12670,#12671);
#11000=AXIS2_PLACEMENT_3D('',#35034,#12672,#12673);
#11001=AXIS2_PLACEMENT_3D('',#35036,#12674,#12675);
#11002=AXIS2_PLACEMENT_3D('',#35039,#12677,#12678);
#11003=AXIS2_PLACEMENT_3D('',#35040,#12679,#12680);
#11004=AXIS2_PLACEMENT_3D('',#35042,#12681,#12682);
#11005=AXIS2_PLACEMENT_3D('',#35045,#12684,#12685);
#11006=AXIS2_PLACEMENT_3D('',#35046,#12686,#12687);
#11007=AXIS2_PLACEMENT_3D('',#35048,#12688,#12689);
#11008=AXIS2_PLACEMENT_3D('',#35051,#12691,#12692);
#11009=AXIS2_PLACEMENT_3D('',#35052,#12693,#12694);
#11010=AXIS2_PLACEMENT_3D('',#35054,#12695,#12696);
#11011=AXIS2_PLACEMENT_3D('',#35057,#12698,#12699);
#11012=AXIS2_PLACEMENT_3D('',#35058,#12700,#12701);
#11013=AXIS2_PLACEMENT_3D('',#35060,#12702,#12703);
#11014=AXIS2_PLACEMENT_3D('',#35063,#12705,#12706);
#11015=AXIS2_PLACEMENT_3D('',#35064,#12707,#12708);
#11016=AXIS2_PLACEMENT_3D('',#35066,#12709,#12710);
#11017=AXIS2_PLACEMENT_3D('',#35069,#12712,#12713);
#11018=AXIS2_PLACEMENT_3D('',#35070,#12714,#12715);
#11019=AXIS2_PLACEMENT_3D('',#35072,#12716,#12717);
#11020=AXIS2_PLACEMENT_3D('',#35075,#12719,#12720);
#11021=AXIS2_PLACEMENT_3D('',#35076,#12721,#12722);
#11022=AXIS2_PLACEMENT_3D('',#35078,#12723,#12724);
#11023=AXIS2_PLACEMENT_3D('',#35081,#12726,#12727);
#11024=AXIS2_PLACEMENT_3D('',#35082,#12728,#12729);
#11025=AXIS2_PLACEMENT_3D('',#35084,#12730,#12731);
#11026=AXIS2_PLACEMENT_3D('',#35087,#12733,#12734);
#11027=AXIS2_PLACEMENT_3D('',#35088,#12735,#12736);
#11028=AXIS2_PLACEMENT_3D('',#35097,#12741,#12742);
#11029=AXIS2_PLACEMENT_3D('',#35103,#12746,#12747);
#11030=AXIS2_PLACEMENT_3D('',#35109,#12751,#12752);
#11031=AXIS2_PLACEMENT_3D('',#35112,#12755,#12756);
#11032=AXIS2_PLACEMENT_3D('',#35113,#12757,#12758);
#11033=AXIS2_PLACEMENT_3D('',#35114,#12759,#12760);
#11034=AXIS2_PLACEMENT_3D('',#35115,#12761,#12762);
#11035=AXIS2_PLACEMENT_3D('',#35117,#12763,#12764);
#11036=AXIS2_PLACEMENT_3D('',#35120,#12766,#12767);
#11037=AXIS2_PLACEMENT_3D('',#35121,#12768,#12769);
#11038=AXIS2_PLACEMENT_3D('',#35123,#12770,#12771);
#11039=AXIS2_PLACEMENT_3D('',#35126,#12773,#12774);
#11040=AXIS2_PLACEMENT_3D('',#35127,#12775,#12776);
#11041=AXIS2_PLACEMENT_3D('',#35129,#12777,#12778);
#11042=AXIS2_PLACEMENT_3D('',#35132,#12780,#12781);
#11043=AXIS2_PLACEMENT_3D('',#35133,#12782,#12783);
#11044=AXIS2_PLACEMENT_3D('',#35135,#12784,#12785);
#11045=AXIS2_PLACEMENT_3D('',#35138,#12787,#12788);
#11046=AXIS2_PLACEMENT_3D('',#35139,#12789,#12790);
#11047=AXIS2_PLACEMENT_3D('',#35141,#12791,#12792);
#11048=AXIS2_PLACEMENT_3D('',#35144,#12794,#12795);
#11049=AXIS2_PLACEMENT_3D('',#35145,#12796,#12797);
#11050=AXIS2_PLACEMENT_3D('',#35147,#12798,#12799);
#11051=AXIS2_PLACEMENT_3D('',#35150,#12801,#12802);
#11052=AXIS2_PLACEMENT_3D('',#35151,#12803,#12804);
#11053=AXIS2_PLACEMENT_3D('',#35153,#12805,#12806);
#11054=AXIS2_PLACEMENT_3D('',#35156,#12808,#12809);
#11055=AXIS2_PLACEMENT_3D('',#35157,#12810,#12811);
#11056=AXIS2_PLACEMENT_3D('',#35166,#12816,#12817);
#11057=AXIS2_PLACEMENT_3D('',#35172,#12821,#12822);
#11058=AXIS2_PLACEMENT_3D('',#35178,#12826,#12827);
#11059=AXIS2_PLACEMENT_3D('',#35181,#12830,#12831);
#11060=AXIS2_PLACEMENT_3D('',#35182,#12832,#12833);
#11061=AXIS2_PLACEMENT_3D('',#35183,#12834,#12835);
#11062=AXIS2_PLACEMENT_3D('',#35184,#12836,#12837);
#11063=AXIS2_PLACEMENT_3D('',#35200,#12839,#12840);
#11064=AXIS2_PLACEMENT_3D('',#35208,#12841,#12842);
#11065=AXIS2_PLACEMENT_3D('',#35256,#12844,#12845);
#11066=AXIS2_PLACEMENT_3D('',#35304,#12847,#12848);
#11067=AXIS2_PLACEMENT_3D('',#35358,#12850,#12851);
#11068=AXIS2_PLACEMENT_3D('',#35406,#12853,#12854);
#11069=AXIS2_PLACEMENT_3D('',#35454,#12856,#12857);
#11070=AXIS2_PLACEMENT_3D('',#35502,#12859,#12860);
#11071=AXIS2_PLACEMENT_3D('',#35556,#12862,#12863);
#11072=AXIS2_PLACEMENT_3D('',#35604,#12865,#12866);
#11073=AXIS2_PLACEMENT_3D('',#35652,#12868,#12869);
#11074=AXIS2_PLACEMENT_3D('',#35706,#12871,#12872);
#11075=AXIS2_PLACEMENT_3D('',#35754,#12874,#12875);
#11076=AXIS2_PLACEMENT_3D('',#35802,#12877,#12878);
#11077=AXIS2_PLACEMENT_3D('',#35853,#12880,#12881);
#11078=AXIS2_PLACEMENT_3D('',#35904,#12883,#12884);
#11079=AXIS2_PLACEMENT_3D('',#35952,#12886,#12887);
#11080=AXIS2_PLACEMENT_3D('',#35966,#12889,#12890);
#11081=AXIS2_PLACEMENT_3D('',#35974,#12891,#12892);
#11082=AXIS2_PLACEMENT_3D('',#35998,#12894,#12895);
#11083=AXIS2_PLACEMENT_3D('',#36022,#12897,#12898);
#11084=AXIS2_PLACEMENT_3D('',#36048,#12900,#12901);
#11085=AXIS2_PLACEMENT_3D('',#36072,#12903,#12904);
#11086=AXIS2_PLACEMENT_3D('',#36096,#12906,#12907);
#11087=AXIS2_PLACEMENT_3D('',#36121,#12909,#12910);
#11088=AXIS2_PLACEMENT_3D('',#36146,#12912,#12913);
#11089=AXIS2_PLACEMENT_3D('',#36170,#12915,#12916);
#11090=AXIS2_PLACEMENT_3D('',#36195,#12918,#12919);
#11091=AXIS2_PLACEMENT_3D('',#36220,#12921,#12922);
#11092=AXIS2_PLACEMENT_3D('',#36244,#12924,#12925);
#11093=AXIS2_PLACEMENT_3D('',#36268,#12927,#12928);
#11094=AXIS2_PLACEMENT_3D('',#36293,#12930,#12931);
#11095=AXIS2_PLACEMENT_3D('',#36318,#12933,#12934);
#11096=AXIS2_PLACEMENT_3D('',#36342,#12936,#12937);
#11097=AXIS2_PLACEMENT_3D('',#36531,#12938,#12939);
#11098=AXIS2_PLACEMENT_3D('',#36637,#12941,#12942);
#11099=AXIS2_PLACEMENT_3D('',#37169,#12943,#12944);
#11100=AXIS2_PLACEMENT_3D('',#37180,#12945,#12946);
#11101=AXIS2_PLACEMENT_3D('',#37714,#12947,#12948);
#11102=AXIS2_PLACEMENT_3D('',#37715,#12949,#12950);
#11103=AXIS2_PLACEMENT_3D('',#37724,#12955,#12956);
#11104=AXIS2_PLACEMENT_3D('',#37730,#12960,#12961);
#11105=AXIS2_PLACEMENT_3D('',#37736,#12965,#12966);
#11106=AXIS2_PLACEMENT_3D('',#37742,#12970,#12971);
#11107=AXIS2_PLACEMENT_3D('',#37748,#12975,#12976);
#11108=AXIS2_PLACEMENT_3D('',#37751,#12979,#12980);
#11109=AXIS2_PLACEMENT_3D('',#37752,#12981,#12982);
#11110=AXIS2_PLACEMENT_3D('',#37754,#12983,#12984);
#11111=AXIS2_PLACEMENT_3D('',#37755,#12985,#12986);
#11112=AXIS2_PLACEMENT_3D('',#37758,#12988,#12989);
#11113=AXIS2_PLACEMENT_3D('',#37759,#12990,#12991);
#11114=AXIS2_PLACEMENT_3D('',#37760,#12992,#12993);
#11115=AXIS2_PLACEMENT_3D('',#37761,#12994,#12995);
#11116=AXIS2_PLACEMENT_3D('',#37762,#12996,#12997);
#11117=AXIS2_PLACEMENT_3D('',#37778,#12999,#13000);
#11118=AXIS2_PLACEMENT_3D('',#37786,#13001,#13002);
#11119=AXIS2_PLACEMENT_3D('',#37834,#13004,#13005);
#11120=AXIS2_PLACEMENT_3D('',#37882,#13007,#13008);
#11121=AXIS2_PLACEMENT_3D('',#37936,#13010,#13011);
#11122=AXIS2_PLACEMENT_3D('',#37984,#13013,#13014);
#11123=AXIS2_PLACEMENT_3D('',#38032,#13016,#13017);
#11124=AXIS2_PLACEMENT_3D('',#38086,#13019,#13020);
#11125=AXIS2_PLACEMENT_3D('',#38134,#13022,#13023);
#11126=AXIS2_PLACEMENT_3D('',#38185,#13025,#13026);
#11127=AXIS2_PLACEMENT_3D('',#38236,#13028,#13029);
#11128=AXIS2_PLACEMENT_3D('',#38284,#13031,#13032);
#11129=AXIS2_PLACEMENT_3D('',#38300,#13034,#13035);
#11130=AXIS2_PLACEMENT_3D('',#38309,#13036,#13037);
#11131=AXIS2_PLACEMENT_3D('',#38334,#13039,#13040);
#11132=AXIS2_PLACEMENT_3D('',#38358,#13042,#13043);
#11133=AXIS2_PLACEMENT_3D('',#38384,#13045,#13046);
#11134=AXIS2_PLACEMENT_3D('',#38408,#13048,#13049);
#11135=AXIS2_PLACEMENT_3D('',#38433,#13051,#13052);
#11136=AXIS2_PLACEMENT_3D('',#38458,#13054,#13055);
#11137=AXIS2_PLACEMENT_3D('',#38482,#13057,#13058);
#11138=AXIS2_PLACEMENT_3D('',#38507,#13060,#13061);
#11139=AXIS2_PLACEMENT_3D('',#38532,#13063,#13064);
#11140=AXIS2_PLACEMENT_3D('',#38556,#13066,#13067);
#11141=AXIS2_PLACEMENT_3D('',#38838,#13068,#13069);
#11142=AXIS2_PLACEMENT_3D('',#38872,#13071,#13072);
#11143=AXIS2_PLACEMENT_3D('',#39297,#13073,#13074);
#11144=AXIS2_PLACEMENT_3D('',#39308,#13075,#13076);
#11145=AXIS2_PLACEMENT_3D('',#39735,#13077,#13078);
#11146=AXIS2_PLACEMENT_3D('',#39736,#13079,#13080);
#11147=AXIS2_PLACEMENT_3D('',#39745,#13085,#13086);
#11148=AXIS2_PLACEMENT_3D('',#39751,#13090,#13091);
#11149=AXIS2_PLACEMENT_3D('',#39757,#13095,#13096);
#11150=AXIS2_PLACEMENT_3D('',#39763,#13100,#13101);
#11151=AXIS2_PLACEMENT_3D('',#39769,#13105,#13106);
#11152=AXIS2_PLACEMENT_3D('',#39772,#13109,#13110);
#11153=AXIS2_PLACEMENT_3D('',#39773,#13111,#13112);
#11154=AXIS2_PLACEMENT_3D('',#39775,#13113,#13114);
#11155=AXIS2_PLACEMENT_3D('',#39776,#13115,#13116);
#11156=AXIS2_PLACEMENT_3D('',#39779,#13118,#13119);
#11157=AXIS2_PLACEMENT_3D('',#39780,#13120,#13121);
#11158=AXIS2_PLACEMENT_3D('',#39781,#13122,#13123);
#11159=AXIS2_PLACEMENT_3D('',#39782,#13124,#13125);
#11160=AXIS2_PLACEMENT_3D('',#39783,#13126,#13127);
#11161=AXIS2_PLACEMENT_3D('',#39805,#13129,#13130);
#11162=AXIS2_PLACEMENT_3D('',#39816,#13131,#13132);
#11163=AXIS2_PLACEMENT_3D('',#39900,#13134,#13135);
#11164=AXIS2_PLACEMENT_3D('',#39990,#13137,#13138);
#11165=AXIS2_PLACEMENT_3D('',#40080,#13140,#13141);
#11166=AXIS2_PLACEMENT_3D('',#40164,#13143,#13144);
#11167=AXIS2_PLACEMENT_3D('',#40254,#13146,#13147);
#11168=AXIS2_PLACEMENT_3D('',#40341,#13149,#13150);
#11169=AXIS2_PLACEMENT_3D('',#40428,#13152,#13153);
#11170=AXIS2_PLACEMENT_3D('',#40518,#13155,#13156);
#11171=AXIS2_PLACEMENT_3D('',#40602,#13158,#13159);
#11172=AXIS2_PLACEMENT_3D('',#40620,#13161,#13162);
#11173=AXIS2_PLACEMENT_3D('',#40631,#13163,#13164);
#11174=AXIS2_PLACEMENT_3D('',#40668,#13166,#13167);
#11175=AXIS2_PLACEMENT_3D('',#40706,#13169,#13170);
#11176=AXIS2_PLACEMENT_3D('',#40742,#13172,#13173);
#11177=AXIS2_PLACEMENT_3D('',#40780,#13175,#13176);
#11178=AXIS2_PLACEMENT_3D('',#40817,#13178,#13179);
#11179=AXIS2_PLACEMENT_3D('',#40854,#13181,#13182);
#11180=AXIS2_PLACEMENT_3D('',#40892,#13184,#13185);
#11181=AXIS2_PLACEMENT_3D('',#41688,#13187,#13188);
#11182=AXIS2_PLACEMENT_3D('',#41690,#13189,#13190);
#11183=AXIS2_PLACEMENT_3D('',#42441,#13191,#13192);
#11184=AXIS2_PLACEMENT_3D('',#42442,#13193,#13194);
#11185=AXIS2_PLACEMENT_3D('',#42443,#13195,#13196);
#11186=AXIS2_PLACEMENT_3D('',#42445,#13197,#13198);
#11187=AXIS2_PLACEMENT_3D('',#42447,#13199,#13200);
#11188=AXIS2_PLACEMENT_3D('',#42448,#13201,#13202);
#11189=AXIS2_PLACEMENT_3D('',#42450,#13203,#13204);
#11190=AXIS2_PLACEMENT_3D('',#42452,#13205,#13206);
#11191=AXIS2_PLACEMENT_3D('',#42453,#13207,#13208);
#11192=AXIS2_PLACEMENT_3D('',#42455,#13210,#13211);
#11193=AXIS2_PLACEMENT_3D('',#42458,#13213,#13214);
#11194=AXIS2_PLACEMENT_3D('',#42459,#13215,#13216);
#11195=AXIS2_PLACEMENT_3D('',#42461,#13217,#13218);
#11196=AXIS2_PLACEMENT_3D('',#42462,#13219,#13220);
#11197=AXIS2_PLACEMENT_3D('',#42464,#13221,#13222);
#11198=AXIS2_PLACEMENT_3D('',#42466,#13223,#13224);
#11199=AXIS2_PLACEMENT_3D('',#42467,#13225,#13226);
#11200=AXIS2_PLACEMENT_3D('',#42469,#13228,#13229);
#11201=AXIS2_PLACEMENT_3D('',#42472,#13231,#13232);
#11202=AXIS2_PLACEMENT_3D('',#42473,#13233,#13234);
#11203=AXIS2_PLACEMENT_3D('',#42475,#13235,#13236);
#11204=AXIS2_PLACEMENT_3D('',#42476,#13237,#13238);
#11205=AXIS2_PLACEMENT_3D('',#42478,#13239,#13240);
#11206=AXIS2_PLACEMENT_3D('',#42480,#13241,#13242);
#11207=AXIS2_PLACEMENT_3D('',#42481,#13243,#13244);
#11208=AXIS2_PLACEMENT_3D('',#42483,#13246,#13247);
#11209=AXIS2_PLACEMENT_3D('',#42486,#13249,#13250);
#11210=AXIS2_PLACEMENT_3D('',#42487,#13251,#13252);
#11211=AXIS2_PLACEMENT_3D('',#42489,#13253,#13254);
#11212=AXIS2_PLACEMENT_3D('',#42491,#13256,#13257);
#11213=AXIS2_PLACEMENT_3D('',#42493,#13258,#13259);
#11214=AXIS2_PLACEMENT_3D('',#42494,#13260,#13261);
#11215=AXIS2_PLACEMENT_3D('',#42496,#13262,#13263);
#11216=AXIS2_PLACEMENT_3D('',#42497,#13264,#13265);
#11217=AXIS2_PLACEMENT_3D('',#42500,#13267,#13268);
#11218=AXIS2_PLACEMENT_3D('',#42501,#13269,#13270);
#11219=AXIS2_PLACEMENT_3D('',#42502,#13271,#13272);
#11220=AXIS2_PLACEMENT_3D('',#42504,#13273,#13274);
#11221=AXIS2_PLACEMENT_3D('',#42506,#13276,#13277);
#11222=AXIS2_PLACEMENT_3D('',#42507,#13278,#13279);
#11223=AXIS2_PLACEMENT_3D('',#42508,#13280,#13281);
#11224=AXIS2_PLACEMENT_3D('',#42510,#13282,#13283);
#11225=AXIS2_PLACEMENT_3D('',#42513,#13285,#13286);
#11226=AXIS2_PLACEMENT_3D('',#42514,#13287,#13288);
#11227=AXIS2_PLACEMENT_3D('',#42516,#13289,#13290);
#11228=AXIS2_PLACEMENT_3D('',#42519,#13292,#13293);
#11229=AXIS2_PLACEMENT_3D('',#42520,#13294,#13295);
#11230=AXIS2_PLACEMENT_3D('',#42521,#13296,#13297);
#11231=AXIS2_PLACEMENT_3D('',#42522,#13298,#13299);
#11232=AXIS2_PLACEMENT_3D('',#42523,#13300,#13301);
#11233=AXIS2_PLACEMENT_3D('',#42524,#13302,#13303);
#11234=AXIS2_PLACEMENT_3D('',#42525,#13304,#13305);
#11235=AXIS2_PLACEMENT_3D('',#42526,#13306,#13307);
#11236=AXIS2_PLACEMENT_3D('',#42527,#13308,#13309);
#11237=AXIS2_PLACEMENT_3D('',#42528,#13310,#13311);
#11238=AXIS2_PLACEMENT_3D('',#42529,#13312,#13313);
#11239=AXIS2_PLACEMENT_3D('',#42530,#13314,#13315);
#11240=AXIS2_PLACEMENT_3D('',#42531,#13316,#13317);
#11241=AXIS2_PLACEMENT_3D('',#42532,#13318,#13319);
#11242=AXIS2_PLACEMENT_3D('',#42533,#13320,#13321);
#11243=AXIS2_PLACEMENT_3D('',#42534,#13322,#13323);
#11244=AXIS2_PLACEMENT_3D('',#42535,#13324,#13325);
#11245=AXIS2_PLACEMENT_3D('',#42536,#13326,#13327);
#11246=AXIS2_PLACEMENT_3D('',#42537,#13328,#13329);
#11247=AXIS2_PLACEMENT_3D('',#42538,#13330,#13331);
#11248=AXIS2_PLACEMENT_3D('',#42539,#13332,#13333);
#11249=AXIS2_PLACEMENT_3D('',#42540,#13334,#13335);
#11250=AXIS2_PLACEMENT_3D('',#42541,#13336,#13337);
#11251=AXIS2_PLACEMENT_3D('',#42542,#13338,#13339);
#11252=AXIS2_PLACEMENT_3D('',#42543,#13340,#13341);
#11253=AXIS2_PLACEMENT_3D('',#42544,#13342,#13343);
#11254=AXIS2_PLACEMENT_3D('',#42545,#13344,#13345);
#11255=AXIS2_PLACEMENT_3D('',#42546,#13346,#13347);
#11256=AXIS2_PLACEMENT_3D('',#42547,#13348,#13349);
#11257=AXIS2_PLACEMENT_3D('',#42548,#13350,#13351);
#11258=AXIS2_PLACEMENT_3D('',#42549,#13352,#13353);
#11259=AXIS2_PLACEMENT_3D('',#42550,#13354,#13355);
#11260=AXIS2_PLACEMENT_3D('',#42551,#13356,#13357);
#11261=AXIS2_PLACEMENT_3D('',#42552,#13358,#13359);
#11262=AXIS2_PLACEMENT_3D('',#42553,#13360,#13361);
#11263=AXIS2_PLACEMENT_3D('',#42554,#13362,#13363);
#11264=AXIS2_PLACEMENT_3D('',#42555,#13364,#13365);
#11265=AXIS2_PLACEMENT_3D('',#42556,#13366,#13367);
#11266=AXIS2_PLACEMENT_3D('',#42557,#13368,#13369);
#11267=AXIS2_PLACEMENT_3D('',#42558,#13370,#13371);
#11268=AXIS2_PLACEMENT_3D('',#42559,#13372,#13373);
#11269=AXIS2_PLACEMENT_3D('',#42560,#13374,#13375);
#11270=AXIS2_PLACEMENT_3D('',#42561,#13376,#13377);
#11271=AXIS2_PLACEMENT_3D('',#42562,#13378,#13379);
#11272=AXIS2_PLACEMENT_3D('',#42563,#13380,#13381);
#11273=AXIS2_PLACEMENT_3D('',#42564,#13382,#13383);
#11274=AXIS2_PLACEMENT_3D('',#42565,#13384,#13385);
#11275=AXIS2_PLACEMENT_3D('',#42566,#13386,#13387);
#11276=AXIS2_PLACEMENT_3D('',#42567,#13388,#13389);
#11277=AXIS2_PLACEMENT_3D('',#42568,#13390,#13391);
#11278=AXIS2_PLACEMENT_3D('',#42569,#13392,#13393);
#11279=AXIS2_PLACEMENT_3D('',#42570,#13394,#13395);
#11280=AXIS2_PLACEMENT_3D('',#42571,#13396,#13397);
#11281=AXIS2_PLACEMENT_3D('',#42572,#13398,#13399);
#11282=AXIS2_PLACEMENT_3D('',#42573,#13400,#13401);
#11283=AXIS2_PLACEMENT_3D('',#42574,#13402,#13403);
#11284=AXIS2_PLACEMENT_3D('',#42575,#13404,#13405);
#11285=AXIS2_PLACEMENT_3D('',#42576,#13406,#13407);
#11286=AXIS2_PLACEMENT_3D('',#42577,#13408,#13409);
#11287=AXIS2_PLACEMENT_3D('',#42578,#13410,#13411);
#11288=AXIS2_PLACEMENT_3D('',#42579,#13412,#13413);
#11289=AXIS2_PLACEMENT_3D('',#42580,#13414,#13415);
#11290=AXIS2_PLACEMENT_3D('',#42581,#13416,#13417);
#11291=AXIS2_PLACEMENT_3D('',#42582,#13418,#13419);
#11292=AXIS2_PLACEMENT_3D('',#42583,#13420,#13421);
#11293=AXIS2_PLACEMENT_3D('',#42584,#13422,#13423);
#11294=AXIS2_PLACEMENT_3D('',#42585,#13424,#13425);
#11295=AXIS2_PLACEMENT_3D('',#42586,#13426,#13427);
#11296=AXIS2_PLACEMENT_3D('',#42587,#13428,#13429);
#11297=AXIS2_PLACEMENT_3D('',#42588,#13430,#13431);
#11298=AXIS2_PLACEMENT_3D('',#42589,#13432,#13433);
#11299=AXIS2_PLACEMENT_3D('',#42590,#13434,#13435);
#11300=AXIS2_PLACEMENT_3D('',#42591,#13436,#13437);
#11301=AXIS2_PLACEMENT_3D('',#42592,#13438,#13439);
#11302=AXIS2_PLACEMENT_3D('',#42593,#13440,#13441);
#11303=AXIS2_PLACEMENT_3D('',#42594,#13442,#13443);
#11304=AXIS2_PLACEMENT_3D('',#42595,#13444,#13445);
#11305=AXIS2_PLACEMENT_3D('',#42596,#13446,#13447);
#11306=DIRECTION('axis',(0.,0.,1.));
#11307=DIRECTION('refdir',(1.,0.,0.));
#11308=DIRECTION('axis',(0.,0.,1.));
#11309=DIRECTION('refdir',(1.,0.,0.));
#11310=DIRECTION('center_axis',(0.,0.,-1.));
#11311=DIRECTION('ref_axis',(1.,0.,0.));
#11312=DIRECTION('',(0.,0.,-1.));
#11313=DIRECTION('center_axis',(0.,0.,1.));
#11314=DIRECTION('ref_axis',(1.,0.,0.));
#11315=DIRECTION('',(0.,0.,-1.));
#11316=DIRECTION('center_axis',(0.,0.,1.));
#11317=DIRECTION('ref_axis',(1.,0.,0.));
#11318=DIRECTION('center_axis',(0.,0.,-1.));
#11319=DIRECTION('ref_axis',(1.,0.,0.));
#11320=DIRECTION('',(0.,0.,-1.));
#11321=DIRECTION('center_axis',(0.,0.,-1.));
#11322=DIRECTION('ref_axis',(1.,0.,0.));
#11323=DIRECTION('',(0.,0.,-1.));
#11324=DIRECTION('center_axis',(0.,0.,-1.));
#11325=DIRECTION('ref_axis',(1.,0.,0.));
#11326=DIRECTION('',(0.,0.,-1.));
#11327=DIRECTION('center_axis',(0.,0.,-1.));
#11328=DIRECTION('ref_axis',(1.,0.,0.));
#11329=DIRECTION('',(0.,0.,-1.));
#11330=DIRECTION('center_axis',(0.,0.,-1.));
#11331=DIRECTION('ref_axis',(1.,0.,0.));
#11332=DIRECTION('',(0.,0.,-1.));
#11333=DIRECTION('center_axis',(0.,0.,-1.));
#11334=DIRECTION('ref_axis',(1.,0.,0.));
#11335=DIRECTION('',(0.,0.,-1.));
#11336=DIRECTION('center_axis',(0.,0.,-1.));
#11337=DIRECTION('ref_axis',(1.,0.,0.));
#11338=DIRECTION('',(0.,0.,-1.));
#11339=DIRECTION('center_axis',(0.,0.,-1.));
#11340=DIRECTION('ref_axis',(1.,0.,0.));
#11341=DIRECTION('',(0.,0.,-1.));
#11342=DIRECTION('center_axis',(0.,0.,-1.));
#11343=DIRECTION('ref_axis',(1.,0.,0.));
#11344=DIRECTION('',(0.,0.,-1.));
#11345=DIRECTION('center_axis',(0.,0.,-1.));
#11346=DIRECTION('ref_axis',(1.,0.,0.));
#11347=DIRECTION('',(0.,0.,-1.));
#11348=DIRECTION('center_axis',(0.,0.,-1.));
#11349=DIRECTION('ref_axis',(1.,0.,0.));
#11350=DIRECTION('',(0.,0.,-1.));
#11351=DIRECTION('center_axis',(0.,0.,-1.));
#11352=DIRECTION('ref_axis',(1.,0.,0.));
#11353=DIRECTION('',(0.,0.,-1.));
#11354=DIRECTION('center_axis',(0.,0.,-1.));
#11355=DIRECTION('ref_axis',(1.,0.,0.));
#11356=DIRECTION('',(0.,0.,-1.));
#11357=DIRECTION('center_axis',(0.,0.,-1.));
#11358=DIRECTION('ref_axis',(0.938438521500727,-0.345446293023284,0.));
#11359=DIRECTION('',(0.,0.,-1.));
#11360=DIRECTION('center_axis',(0.,0.,-1.));
#11361=DIRECTION('ref_axis',(1.,0.,0.));
#11362=DIRECTION('center_axis',(0.,0.,-1.));
#11363=DIRECTION('ref_axis',(0.0179642919149216,0.999838629087712,0.));
#11364=DIRECTION('',(1.22464679914735E-16,-9.01413744397708E-30,-1.));
#11365=DIRECTION('center_axis',(0.,0.,1.));
#11366=DIRECTION('ref_axis',(1.,-7.34835534001804E-14,0.));
#11367=DIRECTION('center_axis',(0.,0.,-1.));
#11368=DIRECTION('ref_axis',(1.,-7.34835534001804E-14,0.));
#11369=DIRECTION('',(1.22464679914735E-16,-9.01413744397708E-30,-1.));
#11370=DIRECTION('center_axis',(0.,0.,-1.));
#11371=DIRECTION('ref_axis',(1.,-7.34835534001804E-14,0.));
#11372=DIRECTION('',(1.22464679914735E-16,-9.01413744397708E-30,-1.));
#11373=DIRECTION('center_axis',(0.,0.,-1.));
#11374=DIRECTION('ref_axis',(1.,-7.34835534001804E-14,0.));
#11375=DIRECTION('',(1.22464679914735E-16,-9.01413744397708E-30,-1.));
#11376=DIRECTION('center_axis',(0.,0.,-1.));
#11377=DIRECTION('ref_axis',(1.,-7.34835534001804E-14,0.));
#11378=DIRECTION('',(1.22464679914735E-16,-9.01413744397708E-30,-1.));
#11379=DIRECTION('center_axis',(0.,0.,-1.));
#11380=DIRECTION('ref_axis',(1.,-7.34835534001804E-14,0.));
#11381=DIRECTION('',(1.22464679914735E-16,-9.01413744397708E-30,-1.));
#11382=DIRECTION('center_axis',(0.,0.,-1.));
#11383=DIRECTION('ref_axis',(1.,-7.34835534001804E-14,0.));
#11384=DIRECTION('',(1.22464679914735E-16,-9.01413744397708E-30,-1.));
#11385=DIRECTION('center_axis',(0.,0.,-1.));
#11386=DIRECTION('ref_axis',(1.,-7.34835534001804E-14,0.));
#11387=DIRECTION('',(1.22464679914735E-16,-9.01413744397708E-30,-1.));
#11388=DIRECTION('center_axis',(0.,0.,-1.));
#11389=DIRECTION('ref_axis',(1.,-7.34835534001804E-14,0.));
#11390=DIRECTION('',(1.22464679914735E-16,-9.01413744397708E-30,-1.));
#11391=DIRECTION('center_axis',(0.,0.,-1.));
#11392=DIRECTION('ref_axis',(1.,-7.34835534001804E-14,0.));
#11393=DIRECTION('',(1.22464679914735E-16,-9.01413744397708E-30,-1.));
#11394=DIRECTION('center_axis',(0.,0.,-1.));
#11395=DIRECTION('ref_axis',(1.,-7.34835534001804E-14,0.));
#11396=DIRECTION('',(1.22464679914735E-16,-9.01413744397708E-30,-1.));
#11397=DIRECTION('center_axis',(0.,0.,-1.));
#11398=DIRECTION('ref_axis',(1.,-7.34835534001804E-14,0.));
#11399=DIRECTION('',(1.22464679914735E-16,-9.01413744397708E-30,-1.));
#11400=DIRECTION('center_axis',(0.,0.,-1.));
#11401=DIRECTION('ref_axis',(1.,-7.34835534001804E-14,0.));
#11402=DIRECTION('',(1.22464679914735E-16,-9.01413744397708E-30,-1.));
#11403=DIRECTION('center_axis',(0.,0.,-1.));
#11404=DIRECTION('ref_axis',(1.,-7.34835534001804E-14,0.));
#11405=DIRECTION('',(1.22464679914735E-16,-9.01413744397708E-30,-1.));
#11406=DIRECTION('center_axis',(0.,0.,-1.));
#11407=DIRECTION('ref_axis',(1.,-7.34835534001804E-14,0.));
#11408=DIRECTION('',(1.22464679914735E-16,-9.01413744397708E-30,-1.));
#11409=DIRECTION('center_axis',(0.,0.,-1.));
#11410=DIRECTION('ref_axis',(-0.609341740308203,-0.792907714376755,0.));
#11411=DIRECTION('',(1.22464679914735E-16,-9.01413744397708E-30,-1.));
#11412=DIRECTION('center_axis',(0.,0.,-1.));
#11413=DIRECTION('ref_axis',(1.,-7.34835534001804E-14,0.));
#11414=DIRECTION('center_axis',(0.,0.,-1.));
#11415=DIRECTION('ref_axis',(1.,0.,0.));
#11416=DIRECTION('',(0.,0.,-1.));
#11417=DIRECTION('center_axis',(0.,0.,1.));
#11418=DIRECTION('ref_axis',(1.,0.,0.));
#11419=DIRECTION('',(0.,0.,-1.));
#11420=DIRECTION('center_axis',(0.,0.,1.));
#11421=DIRECTION('ref_axis',(1.,0.,0.));
#11422=DIRECTION('center_axis',(0.,0.,-1.));
#11423=DIRECTION('ref_axis',(1.,0.,0.));
#11424=DIRECTION('',(0.,0.,-1.));
#11425=DIRECTION('center_axis',(0.,0.,-1.));
#11426=DIRECTION('ref_axis',(1.,0.,0.));
#11427=DIRECTION('',(0.,0.,-1.));
#11428=DIRECTION('center_axis',(0.,0.,-1.));
#11429=DIRECTION('ref_axis',(1.,0.,0.));
#11430=DIRECTION('',(0.,0.,-1.));
#11431=DIRECTION('center_axis',(0.,0.,-1.));
#11432=DIRECTION('ref_axis',(1.,0.,0.));
#11433=DIRECTION('',(0.,0.,-1.));
#11434=DIRECTION('center_axis',(0.,0.,-1.));
#11435=DIRECTION('ref_axis',(1.,0.,0.));
#11436=DIRECTION('',(0.,0.,-1.));
#11437=DIRECTION('center_axis',(0.,0.,-1.));
#11438=DIRECTION('ref_axis',(1.,0.,0.));
#11439=DIRECTION('',(0.,0.,-1.));
#11440=DIRECTION('center_axis',(0.,0.,-1.));
#11441=DIRECTION('ref_axis',(1.,0.,0.));
#11442=DIRECTION('',(0.,0.,-1.));
#11443=DIRECTION('center_axis',(0.,0.,-1.));
#11444=DIRECTION('ref_axis',(1.,0.,0.));
#11445=DIRECTION('',(0.,0.,-1.));
#11446=DIRECTION('center_axis',(0.,0.,-1.));
#11447=DIRECTION('ref_axis',(1.,0.,0.));
#11448=DIRECTION('',(0.,0.,-1.));
#11449=DIRECTION('center_axis',(0.,0.,-1.));
#11450=DIRECTION('ref_axis',(1.,0.,0.));
#11451=DIRECTION('',(0.,0.,-1.));
#11452=DIRECTION('center_axis',(0.,0.,-1.));
#11453=DIRECTION('ref_axis',(1.,0.,0.));
#11454=DIRECTION('',(0.,0.,-1.));
#11455=DIRECTION('center_axis',(0.,0.,-1.));
#11456=DIRECTION('ref_axis',(1.,0.,0.));
#11457=DIRECTION('',(0.,0.,-1.));
#11458=DIRECTION('center_axis',(0.,0.,-1.));
#11459=DIRECTION('ref_axis',(1.,0.,0.));
#11460=DIRECTION('',(0.,0.,-1.));
#11461=DIRECTION('center_axis',(0.,0.,-1.));
#11462=DIRECTION('ref_axis',(0.93843850099312,-0.345446348734193,0.));
#11463=DIRECTION('',(0.,0.,-1.));
#11464=DIRECTION('center_axis',(0.,0.,-1.));
#11465=DIRECTION('ref_axis',(1.,0.,0.));
#11466=DIRECTION('center_axis',(0.,0.,-1.));
#11467=DIRECTION('ref_axis',(0.0179642417346127,0.99983862998931,0.));
#11468=DIRECTION('',(1.22464679914735E-16,-7.95541510913586E-30,-1.));
#11469=DIRECTION('center_axis',(0.,0.,1.));
#11470=DIRECTION('ref_axis',(1.,-6.48384294707476E-14,0.));
#11471=DIRECTION('center_axis',(0.,0.,-1.));
#11472=DIRECTION('ref_axis',(1.,-6.48384294707476E-14,0.));
#11473=DIRECTION('',(1.22464679914735E-16,-7.95541510913586E-30,-1.));
#11474=DIRECTION('center_axis',(0.,0.,-1.));
#11475=DIRECTION('ref_axis',(1.,-6.48384294707476E-14,0.));
#11476=DIRECTION('',(1.22464679914735E-16,-7.95541510913586E-30,-1.));
#11477=DIRECTION('center_axis',(0.,0.,-1.));
#11478=DIRECTION('ref_axis',(1.,-6.48384294707476E-14,0.));
#11479=DIRECTION('',(1.22464679914735E-16,-7.95541510913586E-30,-1.));
#11480=DIRECTION('center_axis',(0.,0.,-1.));
#11481=DIRECTION('ref_axis',(1.,-6.48384294707476E-14,0.));
#11482=DIRECTION('',(1.22464679914735E-16,-7.95541510913586E-30,-1.));
#11483=DIRECTION('center_axis',(0.,0.,-1.));
#11484=DIRECTION('ref_axis',(1.,-6.48384294707476E-14,0.));
#11485=DIRECTION('',(1.22464679914735E-16,-7.95541510913586E-30,-1.));
#11486=DIRECTION('center_axis',(0.,0.,-1.));
#11487=DIRECTION('ref_axis',(1.,-6.48384294707476E-14,0.));
#11488=DIRECTION('',(1.22464679914735E-16,-7.95541510913586E-30,-1.));
#11489=DIRECTION('center_axis',(0.,0.,-1.));
#11490=DIRECTION('ref_axis',(1.,-6.48384294707476E-14,0.));
#11491=DIRECTION('',(1.22464679914735E-16,-7.95541510913586E-30,-1.));
#11492=DIRECTION('center_axis',(0.,0.,-1.));
#11493=DIRECTION('ref_axis',(1.,-6.48384294707476E-14,0.));
#11494=DIRECTION('',(1.22464679914735E-16,-7.95541510913586E-30,-1.));
#11495=DIRECTION('center_axis',(0.,0.,-1.));
#11496=DIRECTION('ref_axis',(1.,-6.48384294707476E-14,0.));
#11497=DIRECTION('',(1.22464679914735E-16,-7.95541510913586E-30,-1.));
#11498=DIRECTION('center_axis',(0.,0.,-1.));
#11499=DIRECTION('ref_axis',(1.,-6.48384294707476E-14,0.));
#11500=DIRECTION('',(1.22464679914735E-16,-7.95541510913586E-30,-1.));
#11501=DIRECTION('center_axis',(0.,0.,-1.));
#11502=DIRECTION('ref_axis',(1.,-6.48384294707476E-14,0.));
#11503=DIRECTION('',(1.22464679914735E-16,-7.95541510913586E-30,-1.));
#11504=DIRECTION('center_axis',(0.,0.,-1.));
#11505=DIRECTION('ref_axis',(1.,-6.48384294707476E-14,0.));
#11506=DIRECTION('',(1.22464679914735E-16,-7.95541510913586E-30,-1.));
#11507=DIRECTION('center_axis',(0.,0.,-1.));
#11508=DIRECTION('ref_axis',(1.,-6.48384294707476E-14,0.));
#11509=DIRECTION('',(1.22464679914735E-16,-7.95541510913586E-30,-1.));
#11510=DIRECTION('center_axis',(0.,0.,-1.));
#11511=DIRECTION('ref_axis',(1.,-6.48384294707476E-14,0.));
#11512=DIRECTION('',(1.22464679914735E-16,-7.95541510913586E-30,-1.));
#11513=DIRECTION('center_axis',(0.,0.,-1.));
#11514=DIRECTION('ref_axis',(-0.609341731077546,-0.792907721470424,0.));
#11515=DIRECTION('',(1.22464679914735E-16,-7.95541510913586E-30,-1.));
#11516=DIRECTION('center_axis',(0.,0.,-1.));
#11517=DIRECTION('ref_axis',(1.,-6.48384294707476E-14,0.));
#11518=DIRECTION('center_axis',(0.,0.,-1.));
#11519=DIRECTION('ref_axis',(1.,0.,0.));
#11520=DIRECTION('',(0.,0.,-1.));
#11521=DIRECTION('center_axis',(0.,0.,1.));
#11522=DIRECTION('ref_axis',(1.,0.,0.));
#11523=DIRECTION('',(0.,0.,-1.));
#11524=DIRECTION('center_axis',(0.,0.,1.));
#11525=DIRECTION('ref_axis',(1.,0.,0.));
#11526=DIRECTION('center_axis',(0.,0.,-1.));
#11527=DIRECTION('ref_axis',(1.,0.,0.));
#11528=DIRECTION('',(0.,0.,-1.));
#11529=DIRECTION('center_axis',(0.,0.,-1.));
#11530=DIRECTION('ref_axis',(1.,0.,0.));
#11531=DIRECTION('',(0.,0.,-1.));
#11532=DIRECTION('center_axis',(0.,0.,-1.));
#11533=DIRECTION('ref_axis',(1.,0.,0.));
#11534=DIRECTION('',(0.,0.,-1.));
#11535=DIRECTION('center_axis',(0.,0.,-1.));
#11536=DIRECTION('ref_axis',(1.,0.,0.));
#11537=DIRECTION('',(0.,0.,-1.));
#11538=DIRECTION('center_axis',(0.,0.,-1.));
#11539=DIRECTION('ref_axis',(1.,0.,0.));
#11540=DIRECTION('',(0.,0.,-1.));
#11541=DIRECTION('center_axis',(0.,0.,-1.));
#11542=DIRECTION('ref_axis',(1.,0.,0.));
#11543=DIRECTION('',(0.,0.,-1.));
#11544=DIRECTION('center_axis',(0.,0.,-1.));
#11545=DIRECTION('ref_axis',(1.,0.,0.));
#11546=DIRECTION('',(0.,0.,-1.));
#11547=DIRECTION('center_axis',(0.,0.,-1.));
#11548=DIRECTION('ref_axis',(1.,0.,0.));
#11549=DIRECTION('',(0.,0.,-1.));
#11550=DIRECTION('center_axis',(0.,0.,-1.));
#11551=DIRECTION('ref_axis',(1.,0.,0.));
#11552=DIRECTION('',(0.,0.,-1.));
#11553=DIRECTION('center_axis',(0.,0.,-1.));
#11554=DIRECTION('ref_axis',(1.,0.,0.));
#11555=DIRECTION('',(0.,0.,-1.));
#11556=DIRECTION('center_axis',(0.,0.,-1.));
#11557=DIRECTION('ref_axis',(1.,0.,0.));
#11558=DIRECTION('',(0.,0.,-1.));
#11559=DIRECTION('center_axis',(0.,0.,-1.));
#11560=DIRECTION('ref_axis',(1.,0.,0.));
#11561=DIRECTION('',(0.,0.,-1.));
#11562=DIRECTION('center_axis',(0.,0.,-1.));
#11563=DIRECTION('ref_axis',(1.,0.,0.));
#11564=DIRECTION('',(0.,0.,-1.));
#11565=DIRECTION('center_axis',(0.,0.,-1.));
#11566=DIRECTION('ref_axis',(0.938438517397114,-0.345446304171149,0.));
#11567=DIRECTION('',(0.,0.,-1.));
#11568=DIRECTION('center_axis',(0.,0.,-1.));
#11569=DIRECTION('ref_axis',(1.,0.,0.));
#11570=DIRECTION('center_axis',(0.,0.,-1.));
#11571=DIRECTION('ref_axis',(0.0179642700006831,0.999838629481449,0.));
#11572=DIRECTION('',(1.22464679914735E-16,-1.00728597788183E-29,-1.));
#11573=DIRECTION('center_axis',(0.,0.,1.));
#11574=DIRECTION('ref_axis',(1.,-8.21286773296134E-14,0.));
#11575=DIRECTION('center_axis',(0.,0.,-1.));
#11576=DIRECTION('ref_axis',(1.,-8.21286773296134E-14,0.));
#11577=DIRECTION('',(1.22464679914735E-16,-1.00728597788183E-29,-1.));
#11578=DIRECTION('center_axis',(0.,0.,-1.));
#11579=DIRECTION('ref_axis',(1.,-8.21286773296134E-14,0.));
#11580=DIRECTION('',(1.22464679914735E-16,-1.00728597788183E-29,-1.));
#11581=DIRECTION('center_axis',(0.,0.,-1.));
#11582=DIRECTION('ref_axis',(1.,-8.21286773296134E-14,0.));
#11583=DIRECTION('',(1.22464679914735E-16,-1.00728597788183E-29,-1.));
#11584=DIRECTION('center_axis',(0.,0.,-1.));
#11585=DIRECTION('ref_axis',(1.,-8.21286773296134E-14,0.));
#11586=DIRECTION('',(1.22464679914735E-16,-1.00728597788183E-29,-1.));
#11587=DIRECTION('center_axis',(0.,0.,-1.));
#11588=DIRECTION('ref_axis',(1.,-8.21286773296134E-14,0.));
#11589=DIRECTION('',(1.22464679914735E-16,-1.00728597788183E-29,-1.));
#11590=DIRECTION('center_axis',(0.,0.,-1.));
#11591=DIRECTION('ref_axis',(1.,-8.21286773296134E-14,0.));
#11592=DIRECTION('',(1.22464679914735E-16,-1.00728597788183E-29,-1.));
#11593=DIRECTION('center_axis',(0.,0.,-1.));
#11594=DIRECTION('ref_axis',(1.,-8.21286773296134E-14,0.));
#11595=DIRECTION('',(1.22464679914735E-16,-1.00728597788183E-29,-1.));
#11596=DIRECTION('center_axis',(0.,0.,-1.));
#11597=DIRECTION('ref_axis',(1.,-8.21286773296134E-14,0.));
#11598=DIRECTION('',(1.22464679914735E-16,-1.00728597788183E-29,-1.));
#11599=DIRECTION('center_axis',(0.,0.,-1.));
#11600=DIRECTION('ref_axis',(1.,-8.21286773296134E-14,0.));
#11601=DIRECTION('',(1.22464679914735E-16,-1.00728597788183E-29,-1.));
#11602=DIRECTION('center_axis',(0.,0.,-1.));
#11603=DIRECTION('ref_axis',(1.,-8.21286773296134E-14,0.));
#11604=DIRECTION('',(1.22464679914735E-16,-1.00728597788183E-29,-1.));
#11605=DIRECTION('center_axis',(0.,0.,-1.));
#11606=DIRECTION('ref_axis',(1.,-8.21286773296134E-14,0.));
#11607=DIRECTION('',(1.22464679914735E-16,-1.00728597788183E-29,-1.));
#11608=DIRECTION('center_axis',(0.,0.,-1.));
#11609=DIRECTION('ref_axis',(1.,-8.21286773296134E-14,0.));
#11610=DIRECTION('',(1.22464679914735E-16,-1.00728597788183E-29,-1.));
#11611=DIRECTION('center_axis',(0.,0.,-1.));
#11612=DIRECTION('ref_axis',(1.,-8.21286773296134E-14,0.));
#11613=DIRECTION('',(1.22464679914735E-16,-1.00728597788183E-29,-1.));
#11614=DIRECTION('center_axis',(0.,0.,-1.));
#11615=DIRECTION('ref_axis',(1.,-8.21286773296134E-14,0.));
#11616=DIRECTION('',(1.22464679914735E-16,-1.00728597788183E-29,-1.));
#11617=DIRECTION('center_axis',(0.,0.,-1.));
#11618=DIRECTION('ref_axis',(-0.609341750416278,-0.792907706608799,0.));
#11619=DIRECTION('',(1.22464679914735E-16,-1.00728597788183E-29,-1.));
#11620=DIRECTION('center_axis',(0.,0.,-1.));
#11621=DIRECTION('ref_axis',(1.,-8.21286773296134E-14,0.));
#11622=DIRECTION('center_axis',(0.,0.,-1.));
#11623=DIRECTION('ref_axis',(1.,0.,0.));
#11624=DIRECTION('',(0.,0.,-1.));
#11625=DIRECTION('center_axis',(0.,0.,1.));
#11626=DIRECTION('ref_axis',(1.,0.,0.));
#11627=DIRECTION('',(0.,0.,-1.));
#11628=DIRECTION('center_axis',(0.,0.,1.));
#11629=DIRECTION('ref_axis',(1.,0.,0.));
#11630=DIRECTION('center_axis',(0.,0.,-1.));
#11631=DIRECTION('ref_axis',(1.,0.,0.));
#11632=DIRECTION('',(0.,0.,-1.));
#11633=DIRECTION('center_axis',(0.,0.,-1.));
#11634=DIRECTION('ref_axis',(1.,0.,0.));
#11635=DIRECTION('',(0.,0.,-1.));
#11636=DIRECTION('center_axis',(0.,0.,-1.));
#11637=DIRECTION('ref_axis',(1.,0.,0.));
#11638=DIRECTION('',(0.,0.,-1.));
#11639=DIRECTION('center_axis',(0.,0.,-1.));
#11640=DIRECTION('ref_axis',(1.,0.,0.));
#11641=DIRECTION('',(0.,0.,-1.));
#11642=DIRECTION('center_axis',(0.,0.,-1.));
#11643=DIRECTION('ref_axis',(1.,0.,0.));
#11644=DIRECTION('',(0.,0.,-1.));
#11645=DIRECTION('center_axis',(0.,0.,-1.));
#11646=DIRECTION('ref_axis',(1.,0.,0.));
#11647=DIRECTION('',(0.,0.,-1.));
#11648=DIRECTION('center_axis',(0.,0.,-1.));
#11649=DIRECTION('ref_axis',(1.,0.,0.));
#11650=DIRECTION('',(0.,0.,-1.));
#11651=DIRECTION('center_axis',(0.,0.,-1.));
#11652=DIRECTION('ref_axis',(1.,0.,0.));
#11653=DIRECTION('',(0.,0.,-1.));
#11654=DIRECTION('center_axis',(0.,0.,-1.));
#11655=DIRECTION('ref_axis',(1.,0.,0.));
#11656=DIRECTION('',(0.,0.,-1.));
#11657=DIRECTION('center_axis',(0.,0.,-1.));
#11658=DIRECTION('ref_axis',(1.,0.,0.));
#11659=DIRECTION('',(0.,0.,-1.));
#11660=DIRECTION('center_axis',(0.,0.,-1.));
#11661=DIRECTION('ref_axis',(1.,0.,0.));
#11662=DIRECTION('',(0.,0.,-1.));
#11663=DIRECTION('center_axis',(0.,0.,-1.));
#11664=DIRECTION('ref_axis',(1.,0.,0.));
#11665=DIRECTION('',(0.,0.,-1.));
#11666=DIRECTION('center_axis',(0.,0.,-1.));
#11667=DIRECTION('ref_axis',(1.,0.,0.));
#11668=DIRECTION('',(0.,0.,-1.));
#11669=DIRECTION('center_axis',(0.,0.,-1.));
#11670=DIRECTION('ref_axis',(0.93843850644045,-0.345446333935992,0.));
#11671=DIRECTION('',(0.,0.,-1.));
#11672=DIRECTION('center_axis',(0.,0.,-1.));
#11673=DIRECTION('ref_axis',(1.,0.,0.));
#11674=DIRECTION('center_axis',(0.,0.,-1.));
#11675=DIRECTION('ref_axis',(0.0179642658157032,0.999838629556641,0.));
#11676=DIRECTION('',(1.22464679914735E-16,-1.00728597788183E-29,-1.));
#11677=DIRECTION('center_axis',(0.,0.,1.));
#11678=DIRECTION('ref_axis',(1.,-8.21286773296138E-14,0.));
#11679=DIRECTION('center_axis',(0.,0.,-1.));
#11680=DIRECTION('ref_axis',(1.,-8.21286773296138E-14,0.));
#11681=DIRECTION('',(1.22464679914735E-16,-1.00728597788183E-29,-1.));
#11682=DIRECTION('center_axis',(0.,0.,-1.));
#11683=DIRECTION('ref_axis',(1.,-8.21286773296138E-14,0.));
#11684=DIRECTION('',(1.22464679914735E-16,-1.00728597788183E-29,-1.));
#11685=DIRECTION('center_axis',(0.,0.,-1.));
#11686=DIRECTION('ref_axis',(1.,-8.21286773296138E-14,0.));
#11687=DIRECTION('',(1.22464679914735E-16,-1.00728597788183E-29,-1.));
#11688=DIRECTION('center_axis',(0.,0.,-1.));
#11689=DIRECTION('ref_axis',(1.,-8.21286773296138E-14,0.));
#11690=DIRECTION('',(1.22464679914735E-16,-1.00728597788183E-29,-1.));
#11691=DIRECTION('center_axis',(0.,0.,-1.));
#11692=DIRECTION('ref_axis',(1.,-8.21286773296138E-14,0.));
#11693=DIRECTION('',(1.22464679914735E-16,-1.00728597788183E-29,-1.));
#11694=DIRECTION('center_axis',(0.,0.,-1.));
#11695=DIRECTION('ref_axis',(1.,-8.21286773296138E-14,0.));
#11696=DIRECTION('',(1.22464679914735E-16,-1.00728597788183E-29,-1.));
#11697=DIRECTION('center_axis',(0.,0.,-1.));
#11698=DIRECTION('ref_axis',(1.,-8.21286773296138E-14,0.));
#11699=DIRECTION('',(1.22464679914735E-16,-1.00728597788183E-29,-1.));
#11700=DIRECTION('center_axis',(0.,0.,-1.));
#11701=DIRECTION('ref_axis',(1.,-8.21286773296138E-14,0.));
#11702=DIRECTION('',(1.22464679914735E-16,-1.00728597788183E-29,-1.));
#11703=DIRECTION('center_axis',(0.,0.,-1.));
#11704=DIRECTION('ref_axis',(1.,-8.21286773296138E-14,0.));
#11705=DIRECTION('',(1.22464679914735E-16,-1.00728597788183E-29,-1.));
#11706=DIRECTION('center_axis',(0.,0.,-1.));
#11707=DIRECTION('ref_axis',(1.,-8.21286773296138E-14,0.));
#11708=DIRECTION('',(1.22464679914735E-16,-1.00728597788183E-29,-1.));
#11709=DIRECTION('center_axis',(0.,0.,-1.));
#11710=DIRECTION('ref_axis',(1.,-8.21286773296138E-14,0.));
#11711=DIRECTION('',(1.22464679914735E-16,-1.00728597788183E-29,-1.));
#11712=DIRECTION('center_axis',(0.,0.,-1.));
#11713=DIRECTION('ref_axis',(1.,-8.21286773296138E-14,0.));
#11714=DIRECTION('',(1.22464679914735E-16,-1.00728597788183E-29,-1.));
#11715=DIRECTION('center_axis',(0.,0.,-1.));
#11716=DIRECTION('ref_axis',(1.,-8.21286773296138E-14,0.));
#11717=DIRECTION('',(1.22464679914735E-16,-1.00728597788183E-29,-1.));
#11718=DIRECTION('center_axis',(0.,0.,-1.));
#11719=DIRECTION('ref_axis',(1.,-8.21286773296138E-14,0.));
#11720=DIRECTION('',(1.22464679914735E-16,-1.00728597788183E-29,-1.));
#11721=DIRECTION('center_axis',(0.,0.,-1.));
#11722=DIRECTION('ref_axis',(-0.609341722721044,-0.792907727892313,0.));
#11723=DIRECTION('',(1.22464679914735E-16,-1.00728597788183E-29,-1.));
#11724=DIRECTION('center_axis',(0.,0.,-1.));
#11725=DIRECTION('ref_axis',(1.,-8.21286773296138E-14,0.));
#11726=DIRECTION('center_axis',(0.,0.,1.));
#11727=DIRECTION('ref_axis',(0.000672283037009468,0.999999774017734,0.));
#11728=DIRECTION('',(0.,0.,1.));
#11729=DIRECTION('center_axis',(0.,0.,-1.));
#11730=DIRECTION('ref_axis',(-1.,0.,0.));
#11731=DIRECTION('center_axis',(0.,0.,-1.));
#11732=DIRECTION('ref_axis',(-1.,0.,0.));
#11733=DIRECTION('center_axis',(0.,0.,1.));
#11734=DIRECTION('ref_axis',(-1.,0.,0.));
#11735=DIRECTION('',(0.,0.,1.));
#11736=DIRECTION('center_axis',(0.,0.,1.));
#11737=DIRECTION('ref_axis',(-1.,0.,0.));
#11738=DIRECTION('',(0.,0.,1.));
#11739=DIRECTION('center_axis',(0.,0.,1.));
#11740=DIRECTION('ref_axis',(-1.,0.,0.));
#11741=DIRECTION('',(0.,0.,1.));
#11742=DIRECTION('center_axis',(0.,0.,1.));
#11743=DIRECTION('ref_axis',(-1.,0.,0.));
#11744=DIRECTION('',(0.,0.,1.));
#11745=DIRECTION('center_axis',(0.,0.,1.));
#11746=DIRECTION('ref_axis',(-1.,0.,0.));
#11747=DIRECTION('',(0.,0.,1.));
#11748=DIRECTION('center_axis',(0.,0.,1.));
#11749=DIRECTION('ref_axis',(-1.,0.,0.));
#11750=DIRECTION('',(0.,0.,1.));
#11751=DIRECTION('center_axis',(0.,0.,1.));
#11752=DIRECTION('ref_axis',(-1.,0.,0.));
#11753=DIRECTION('',(0.,0.,1.));
#11754=DIRECTION('center_axis',(0.,0.,1.));
#11755=DIRECTION('ref_axis',(-1.,0.,0.));
#11756=DIRECTION('',(0.,0.,1.));
#11757=DIRECTION('center_axis',(0.,0.,1.));
#11758=DIRECTION('ref_axis',(-1.,0.,0.));
#11759=DIRECTION('',(0.,0.,1.));
#11760=DIRECTION('center_axis',(0.,0.,1.));
#11761=DIRECTION('ref_axis',(-1.,0.,0.));
#11762=DIRECTION('',(0.,0.,1.));
#11763=DIRECTION('center_axis',(0.,0.,1.));
#11764=DIRECTION('ref_axis',(-1.,0.,0.));
#11765=DIRECTION('',(0.,0.,1.));
#11766=DIRECTION('center_axis',(0.,0.,1.));
#11767=DIRECTION('ref_axis',(-1.,0.,0.));
#11768=DIRECTION('',(0.,0.,1.));
#11769=DIRECTION('center_axis',(0.,0.,1.));
#11770=DIRECTION('ref_axis',(-1.,0.,0.));
#11771=DIRECTION('',(0.,0.,1.));
#11772=DIRECTION('center_axis',(0.,0.,1.));
#11773=DIRECTION('ref_axis',(-0.938007161567557,-0.346615875066297,0.));
#11774=DIRECTION('',(0.,0.,1.));
#11775=DIRECTION('center_axis',(0.,0.,-1.));
#11776=DIRECTION('ref_axis',(-1.,0.,0.));
#11777=DIRECTION('center_axis',(0.,0.,1.));
#11778=DIRECTION('ref_axis',(0.000672370108301728,0.999999773959193,0.));
#11779=DIRECTION('',(0.,0.,1.));
#11780=DIRECTION('center_axis',(0.,0.,-1.));
#11781=DIRECTION('ref_axis',(-1.,0.,0.));
#11782=DIRECTION('center_axis',(0.,0.,-1.));
#11783=DIRECTION('ref_axis',(-1.,0.,0.));
#11784=DIRECTION('center_axis',(0.,0.,1.));
#11785=DIRECTION('ref_axis',(-1.,0.,0.));
#11786=DIRECTION('',(0.,0.,1.));
#11787=DIRECTION('center_axis',(0.,0.,1.));
#11788=DIRECTION('ref_axis',(-1.,0.,0.));
#11789=DIRECTION('',(0.,0.,1.));
#11790=DIRECTION('center_axis',(0.,0.,1.));
#11791=DIRECTION('ref_axis',(-1.,0.,0.));
#11792=DIRECTION('',(0.,0.,1.));
#11793=DIRECTION('center_axis',(0.,0.,1.));
#11794=DIRECTION('ref_axis',(-1.,0.,0.));
#11795=DIRECTION('',(0.,0.,1.));
#11796=DIRECTION('center_axis',(0.,0.,1.));
#11797=DIRECTION('ref_axis',(-1.,0.,0.));
#11798=DIRECTION('',(0.,0.,1.));
#11799=DIRECTION('center_axis',(0.,0.,1.));
#11800=DIRECTION('ref_axis',(-1.,0.,0.));
#11801=DIRECTION('',(0.,0.,1.));
#11802=DIRECTION('center_axis',(0.,0.,1.));
#11803=DIRECTION('ref_axis',(-1.,0.,0.));
#11804=DIRECTION('',(0.,0.,1.));
#11805=DIRECTION('center_axis',(0.,0.,1.));
#11806=DIRECTION('ref_axis',(-1.,0.,0.));
#11807=DIRECTION('',(0.,0.,1.));
#11808=DIRECTION('center_axis',(0.,0.,1.));
#11809=DIRECTION('ref_axis',(-1.,0.,0.));
#11810=DIRECTION('',(0.,0.,1.));
#11811=DIRECTION('center_axis',(0.,0.,1.));
#11812=DIRECTION('ref_axis',(-1.,0.,0.));
#11813=DIRECTION('',(0.,0.,1.));
#11814=DIRECTION('center_axis',(0.,0.,1.));
#11815=DIRECTION('ref_axis',(-1.,0.,0.));
#11816=DIRECTION('',(0.,0.,1.));
#11817=DIRECTION('center_axis',(0.,0.,1.));
#11818=DIRECTION('ref_axis',(-1.,0.,0.));
#11819=DIRECTION('',(0.,0.,1.));
#11820=DIRECTION('center_axis',(0.,0.,1.));
#11821=DIRECTION('ref_axis',(-1.,0.,0.));
#11822=DIRECTION('',(0.,0.,1.));
#11823=DIRECTION('center_axis',(0.,0.,1.));
#11824=DIRECTION('ref_axis',(-0.938007170856739,-0.346615849928038,0.));
#11825=DIRECTION('',(0.,0.,1.));
#11826=DIRECTION('center_axis',(0.,0.,-1.));
#11827=DIRECTION('ref_axis',(-1.,0.,0.));
#11828=DIRECTION('center_axis',(0.,0.,1.));
#11829=DIRECTION('ref_axis',(-1.,-7.80244585388103E-14,0.));
#11830=DIRECTION('',(-1.22464679914735E-16,-9.57023793830256E-30,1.));
#11831=DIRECTION('center_axis',(0.,0.,-1.));
#11832=DIRECTION('ref_axis',(-1.,-7.80244585388103E-14,0.));
#11833=DIRECTION('center_axis',(0.,0.,1.));
#11834=DIRECTION('ref_axis',(-1.,-7.80244585388103E-14,0.));
#11835=DIRECTION('',(-1.22464679914735E-16,-9.57023793830256E-30,1.));
#11836=DIRECTION('center_axis',(0.,0.,1.));
#11837=DIRECTION('ref_axis',(-1.,-7.80244585388103E-14,0.));
#11838=DIRECTION('',(-1.22464679914735E-16,-9.57023793830256E-30,1.));
#11839=DIRECTION('center_axis',(0.,0.,1.));
#11840=DIRECTION('ref_axis',(-1.,-7.80244585388103E-14,0.));
#11841=DIRECTION('',(-1.22464679914735E-16,-9.57023793830256E-30,1.));
#11842=DIRECTION('center_axis',(0.,0.,1.));
#11843=DIRECTION('ref_axis',(-1.,-7.80244585388103E-14,0.));
#11844=DIRECTION('',(-1.22464679914735E-16,-9.57023793830256E-30,1.));
#11845=DIRECTION('center_axis',(0.,0.,1.));
#11846=DIRECTION('ref_axis',(-1.,-7.80244585388103E-14,0.));
#11847=DIRECTION('',(-1.22464679914735E-16,-9.57023793830256E-30,1.));
#11848=DIRECTION('center_axis',(0.,0.,1.));
#11849=DIRECTION('ref_axis',(-1.,-7.80244585388103E-14,0.));
#11850=DIRECTION('',(-1.22464679914735E-16,-9.57023793830256E-30,1.));
#11851=DIRECTION('center_axis',(0.,0.,1.));
#11852=DIRECTION('ref_axis',(-1.,-7.80244585388103E-14,0.));
#11853=DIRECTION('',(-1.22464679914735E-16,-9.57023793830256E-30,1.));
#11854=DIRECTION('center_axis',(0.,0.,1.));
#11855=DIRECTION('ref_axis',(-1.,-7.80244585388103E-14,0.));
#11856=DIRECTION('',(-1.22464679914735E-16,-9.57023793830256E-30,1.));
#11857=DIRECTION('center_axis',(0.,0.,1.));
#11858=DIRECTION('ref_axis',(-1.,-7.80244585388103E-14,0.));
#11859=DIRECTION('',(-1.22464679914735E-16,-9.57023793830256E-30,1.));
#11860=DIRECTION('center_axis',(0.,0.,1.));
#11861=DIRECTION('ref_axis',(-1.,-7.80244585388103E-14,0.));
#11862=DIRECTION('',(-1.22464679914735E-16,-9.57023793830256E-30,1.));
#11863=DIRECTION('center_axis',(0.,0.,1.));
#11864=DIRECTION('ref_axis',(-1.,-7.80244585388103E-14,0.));
#11865=DIRECTION('',(-1.22464679914735E-16,-9.57023793830256E-30,1.));
#11866=DIRECTION('center_axis',(0.,0.,1.));
#11867=DIRECTION('ref_axis',(-1.,-7.80244585388103E-14,0.));
#11868=DIRECTION('',(-1.22464679914735E-16,-9.57023793830256E-30,1.));
#11869=DIRECTION('center_axis',(0.,0.,1.));
#11870=DIRECTION('ref_axis',(-1.,-7.80244585388103E-14,0.));
#11871=DIRECTION('',(-1.22464679914735E-16,-9.57023793830256E-30,1.));
#11872=DIRECTION('center_axis',(0.,0.,1.));
#11873=DIRECTION('ref_axis',(0.609168748886822,-0.793040626563144,0.));
#11874=DIRECTION('',(-1.22464679914735E-16,-9.57023793830256E-30,1.));
#11875=DIRECTION('center_axis',(0.,0.,1.));
#11876=DIRECTION('ref_axis',(-1.,-7.80244585388103E-14,0.));
#11877=DIRECTION('center_axis',(0.,0.,1.));
#11878=DIRECTION('ref_axis',(-1.,-7.80244585388103E-14,0.));
#11879=DIRECTION('',(-1.22464679914735E-16,-9.57023793830256E-30,1.));
#11880=DIRECTION('center_axis',(0.,0.,-1.));
#11881=DIRECTION('ref_axis',(-1.,-7.80244585388103E-14,0.));
#11882=DIRECTION('center_axis',(0.,0.,1.));
#11883=DIRECTION('ref_axis',(-1.,-7.80244585388103E-14,0.));
#11884=DIRECTION('',(-1.22464679914735E-16,-9.57023793830256E-30,1.));
#11885=DIRECTION('center_axis',(0.,0.,1.));
#11886=DIRECTION('ref_axis',(-1.,-7.80244585388103E-14,0.));
#11887=DIRECTION('',(-1.22464679914735E-16,-9.57023793830256E-30,1.));
#11888=DIRECTION('center_axis',(0.,0.,1.));
#11889=DIRECTION('ref_axis',(-1.,-7.80244585388103E-14,0.));
#11890=DIRECTION('',(-1.22464679914735E-16,-9.57023793830256E-30,1.));
#11891=DIRECTION('center_axis',(0.,0.,1.));
#11892=DIRECTION('ref_axis',(-1.,-7.80244585388103E-14,0.));
#11893=DIRECTION('',(-1.22464679914735E-16,-9.57023793830256E-30,1.));
#11894=DIRECTION('center_axis',(0.,0.,1.));
#11895=DIRECTION('ref_axis',(-1.,-7.80244585388103E-14,0.));
#11896=DIRECTION('',(-1.22464679914735E-16,-9.57023793830256E-30,1.));
#11897=DIRECTION('center_axis',(0.,0.,1.));
#11898=DIRECTION('ref_axis',(-1.,-7.80244585388103E-14,0.));
#11899=DIRECTION('',(-1.22464679914735E-16,-9.57023793830256E-30,1.));
#11900=DIRECTION('center_axis',(0.,0.,1.));
#11901=DIRECTION('ref_axis',(-1.,-7.80244585388103E-14,0.));
#11902=DIRECTION('',(-1.22464679914735E-16,-9.57023793830256E-30,1.));
#11903=DIRECTION('center_axis',(0.,0.,1.));
#11904=DIRECTION('ref_axis',(-1.,-7.80244585388103E-14,0.));
#11905=DIRECTION('',(-1.22464679914735E-16,-9.57023793830256E-30,1.));
#11906=DIRECTION('center_axis',(0.,0.,1.));
#11907=DIRECTION('ref_axis',(-1.,-7.80244585388103E-14,0.));
#11908=DIRECTION('',(-1.22464679914735E-16,-9.57023793830256E-30,1.));
#11909=DIRECTION('center_axis',(0.,0.,1.));
#11910=DIRECTION('ref_axis',(-1.,-7.80244585388103E-14,0.));
#11911=DIRECTION('',(-1.22464679914735E-16,-9.57023793830256E-30,1.));
#11912=DIRECTION('center_axis',(0.,0.,1.));
#11913=DIRECTION('ref_axis',(-1.,-7.80244585388103E-14,0.));
#11914=DIRECTION('',(-1.22464679914735E-16,-9.57023793830256E-30,1.));
#11915=DIRECTION('center_axis',(0.,0.,1.));
#11916=DIRECTION('ref_axis',(-1.,-7.80244585388103E-14,0.));
#11917=DIRECTION('',(-1.22464679914735E-16,-9.57023793830256E-30,1.));
#11918=DIRECTION('center_axis',(0.,0.,1.));
#11919=DIRECTION('ref_axis',(-1.,-7.80244585388103E-14,0.));
#11920=DIRECTION('',(-1.22464679914735E-16,-9.57023793830256E-30,1.));
#11921=DIRECTION('center_axis',(0.,0.,1.));
#11922=DIRECTION('ref_axis',(0.609168765471054,-0.793040613824079,0.));
#11923=DIRECTION('',(-1.22464679914735E-16,-9.57023793830256E-30,1.));
#11924=DIRECTION('center_axis',(0.,0.,1.));
#11925=DIRECTION('ref_axis',(-1.,-7.80244585388103E-14,0.));
#11926=DIRECTION('center_axis',(0.,0.,1.));
#11927=DIRECTION('ref_axis',(-1.,0.,0.));
#11928=DIRECTION('',(0.,0.,1.));
#11929=DIRECTION('center_axis',(0.,0.,-1.));
#11930=DIRECTION('ref_axis',(-1.,0.,0.));
#11931=DIRECTION('',(0.,0.,1.));
#11932=DIRECTION('center_axis',(0.,0.,-1.));
#11933=DIRECTION('ref_axis',(-1.,0.,0.));
#11934=DIRECTION('center_axis',(0.,0.,-1.));
#11935=DIRECTION('ref_axis',(-1.,0.,0.));
#11936=DIRECTION('center_axis',(0.,0.,1.));
#11937=DIRECTION('ref_axis',(-1.,0.,0.));
#11938=DIRECTION('',(0.,0.,1.));
#11939=DIRECTION('center_axis',(0.,0.,1.));
#11940=DIRECTION('ref_axis',(-1.,0.,0.));
#11941=DIRECTION('',(0.,0.,1.));
#11942=DIRECTION('center_axis',(0.,0.,1.));
#11943=DIRECTION('ref_axis',(-1.,0.,0.));
#11944=DIRECTION('',(0.,0.,1.));
#11945=DIRECTION('center_axis',(0.,0.,1.));
#11946=DIRECTION('ref_axis',(-1.,0.,0.));
#11947=DIRECTION('',(0.,0.,1.));
#11948=DIRECTION('center_axis',(0.,0.,1.));
#11949=DIRECTION('ref_axis',(-1.,0.,0.));
#11950=DIRECTION('',(0.,0.,1.));
#11951=DIRECTION('center_axis',(0.,0.,1.));
#11952=DIRECTION('ref_axis',(-1.,0.,0.));
#11953=DIRECTION('',(0.,0.,1.));
#11954=DIRECTION('center_axis',(0.,0.,1.));
#11955=DIRECTION('ref_axis',(-1.,0.,0.));
#11956=DIRECTION('',(0.,0.,1.));
#11957=DIRECTION('center_axis',(0.,0.,1.));
#11958=DIRECTION('ref_axis',(-1.,0.,0.));
#11959=DIRECTION('',(0.,0.,1.));
#11960=DIRECTION('center_axis',(0.,0.,1.));
#11961=DIRECTION('ref_axis',(-1.,0.,0.));
#11962=DIRECTION('',(0.,0.,1.));
#11963=DIRECTION('center_axis',(0.,0.,1.));
#11964=DIRECTION('ref_axis',(-1.,0.,0.));
#11965=DIRECTION('',(0.,0.,1.));
#11966=DIRECTION('center_axis',(0.,0.,1.));
#11967=DIRECTION('ref_axis',(-1.,0.,0.));
#11968=DIRECTION('',(0.,0.,1.));
#11969=DIRECTION('center_axis',(0.,0.,1.));
#11970=DIRECTION('ref_axis',(-1.,0.,0.));
#11971=DIRECTION('',(0.,0.,1.));
#11972=DIRECTION('center_axis',(0.,0.,1.));
#11973=DIRECTION('ref_axis',(-1.,0.,0.));
#11974=DIRECTION('',(0.,0.,1.));
#11975=DIRECTION('center_axis',(0.,0.,1.));
#11976=DIRECTION('ref_axis',(-0.938007151213456,-0.346615903086422,0.));
#11977=DIRECTION('',(0.,0.,1.));
#11978=DIRECTION('center_axis',(0.,0.,-1.));
#11979=DIRECTION('ref_axis',(-1.,0.,0.));
#11980=DIRECTION('center_axis',(0.,0.,1.));
#11981=DIRECTION('ref_axis',(-1.,-7.80244585388104E-14,0.));
#11982=DIRECTION('',(-1.22464679914735E-16,-9.57023793830257E-30,1.));
#11983=DIRECTION('center_axis',(0.,0.,-1.));
#11984=DIRECTION('ref_axis',(-1.,-7.80244585388104E-14,0.));
#11985=DIRECTION('center_axis',(0.,0.,1.));
#11986=DIRECTION('ref_axis',(-1.,-7.80244585388104E-14,0.));
#11987=DIRECTION('',(-1.22464679914735E-16,-9.57023793830257E-30,1.));
#11988=DIRECTION('center_axis',(0.,0.,1.));
#11989=DIRECTION('ref_axis',(-1.,-7.80244585388104E-14,0.));
#11990=DIRECTION('',(-1.22464679914735E-16,-9.57023793830257E-30,1.));
#11991=DIRECTION('center_axis',(0.,0.,1.));
#11992=DIRECTION('ref_axis',(-1.,-7.80244585388104E-14,0.));
#11993=DIRECTION('',(-1.22464679914735E-16,-9.57023793830257E-30,1.));
#11994=DIRECTION('center_axis',(0.,0.,1.));
#11995=DIRECTION('ref_axis',(-1.,-7.80244585388104E-14,0.));
#11996=DIRECTION('',(-1.22464679914735E-16,-9.57023793830257E-30,1.));
#11997=DIRECTION('center_axis',(0.,0.,1.));
#11998=DIRECTION('ref_axis',(-1.,-7.80244585388104E-14,0.));
#11999=DIRECTION('',(-1.22464679914735E-16,-9.57023793830257E-30,1.));
#12000=DIRECTION('center_axis',(0.,0.,1.));
#12001=DIRECTION('ref_axis',(-1.,-7.80244585388104E-14,0.));
#12002=DIRECTION('',(-1.22464679914735E-16,-9.57023793830257E-30,1.));
#12003=DIRECTION('center_axis',(0.,0.,1.));
#12004=DIRECTION('ref_axis',(-1.,-7.80244585388104E-14,0.));
#12005=DIRECTION('',(-1.22464679914735E-16,-9.57023793830257E-30,1.));
#12006=DIRECTION('center_axis',(0.,0.,1.));
#12007=DIRECTION('ref_axis',(-1.,-7.80244585388104E-14,0.));
#12008=DIRECTION('',(-1.22464679914735E-16,-9.57023793830257E-30,1.));
#12009=DIRECTION('center_axis',(0.,0.,1.));
#12010=DIRECTION('ref_axis',(-1.,-7.80244585388104E-14,0.));
#12011=DIRECTION('',(-1.22464679914735E-16,-9.57023793830257E-30,1.));
#12012=DIRECTION('center_axis',(0.,0.,1.));
#12013=DIRECTION('ref_axis',(-1.,-7.80244585388104E-14,0.));
#12014=DIRECTION('',(-1.22464679914735E-16,-9.57023793830257E-30,1.));
#12015=DIRECTION('center_axis',(0.,0.,1.));
#12016=DIRECTION('ref_axis',(-1.,-7.80244585388104E-14,0.));
#12017=DIRECTION('',(-1.22464679914735E-16,-9.57023793830257E-30,1.));
#12018=DIRECTION('center_axis',(0.,0.,1.));
#12019=DIRECTION('ref_axis',(-1.,-7.80244585388104E-14,0.));
#12020=DIRECTION('',(-1.22464679914735E-16,-9.57023793830257E-30,1.));
#12021=DIRECTION('center_axis',(0.,0.,1.));
#12022=DIRECTION('ref_axis',(-1.,-7.80244585388104E-14,0.));
#12023=DIRECTION('',(-1.22464679914735E-16,-9.57023793830257E-30,1.));
#12024=DIRECTION('center_axis',(0.,0.,1.));
#12025=DIRECTION('ref_axis',(0.609168720998191,-0.793040647985605,0.));
#12026=DIRECTION('',(-1.22464679914735E-16,-9.57023793830257E-30,1.));
#12027=DIRECTION('center_axis',(0.,0.,1.));
#12028=DIRECTION('ref_axis',(-1.,-7.80244585388104E-14,0.));
#12029=DIRECTION('center_axis',(0.,0.,1.));
#12030=DIRECTION('ref_axis',(-1.,0.,0.));
#12031=DIRECTION('',(0.,0.,1.));
#12032=DIRECTION('center_axis',(0.,0.,-1.));
#12033=DIRECTION('ref_axis',(-1.,0.,0.));
#12034=DIRECTION('',(0.,0.,1.));
#12035=DIRECTION('center_axis',(0.,0.,-1.));
#12036=DIRECTION('ref_axis',(-1.,0.,0.));
#12037=DIRECTION('center_axis',(0.,0.,-1.));
#12038=DIRECTION('ref_axis',(-1.,0.,0.));
#12039=DIRECTION('center_axis',(0.,0.,1.));
#12040=DIRECTION('ref_axis',(-1.,0.,0.));
#12041=DIRECTION('',(0.,0.,1.));
#12042=DIRECTION('center_axis',(0.,0.,1.));
#12043=DIRECTION('ref_axis',(-1.,0.,0.));
#12044=DIRECTION('',(0.,0.,1.));
#12045=DIRECTION('center_axis',(0.,0.,1.));
#12046=DIRECTION('ref_axis',(-1.,0.,0.));
#12047=DIRECTION('',(0.,0.,1.));
#12048=DIRECTION('center_axis',(0.,0.,1.));
#12049=DIRECTION('ref_axis',(-1.,0.,0.));
#12050=DIRECTION('',(0.,0.,1.));
#12051=DIRECTION('center_axis',(0.,0.,1.));
#12052=DIRECTION('ref_axis',(-1.,0.,0.));
#12053=DIRECTION('',(0.,0.,1.));
#12054=DIRECTION('center_axis',(0.,0.,1.));
#12055=DIRECTION('ref_axis',(-1.,0.,0.));
#12056=DIRECTION('',(0.,0.,1.));
#12057=DIRECTION('center_axis',(0.,0.,1.));
#12058=DIRECTION('ref_axis',(-1.,0.,0.));
#12059=DIRECTION('',(0.,0.,1.));
#12060=DIRECTION('center_axis',(0.,0.,1.));
#12061=DIRECTION('ref_axis',(-1.,0.,0.));
#12062=DIRECTION('',(0.,0.,1.));
#12063=DIRECTION('center_axis',(0.,0.,1.));
#12064=DIRECTION('ref_axis',(-1.,0.,0.));
#12065=DIRECTION('',(0.,0.,1.));
#12066=DIRECTION('center_axis',(0.,0.,1.));
#12067=DIRECTION('ref_axis',(-1.,0.,0.));
#12068=DIRECTION('',(0.,0.,1.));
#12069=DIRECTION('center_axis',(0.,0.,1.));
#12070=DIRECTION('ref_axis',(-1.,0.,0.));
#12071=DIRECTION('',(0.,0.,1.));
#12072=DIRECTION('center_axis',(0.,0.,1.));
#12073=DIRECTION('ref_axis',(-1.,0.,0.));
#12074=DIRECTION('',(0.,0.,1.));
#12075=DIRECTION('center_axis',(0.,0.,1.));
#12076=DIRECTION('ref_axis',(-1.,0.,0.));
#12077=DIRECTION('',(0.,0.,1.));
#12078=DIRECTION('center_axis',(0.,0.,1.));
#12079=DIRECTION('ref_axis',(-0.938007139797982,-0.346615933978819,0.));
#12080=DIRECTION('',(0.,0.,1.));
#12081=DIRECTION('center_axis',(0.,0.,-1.));
#12082=DIRECTION('ref_axis',(-1.,0.,0.));
#12083=DIRECTION('center_axis',(0.,0.,1.));
#12084=DIRECTION('ref_axis',(-1.,-7.2244869017417E-14,0.));
#12085=DIRECTION('',(-1.22464679914735E-16,-8.86244235752658E-30,1.));
#12086=DIRECTION('center_axis',(0.,0.,-1.));
#12087=DIRECTION('ref_axis',(-1.,-7.22448690174171E-14,0.));
#12088=DIRECTION('center_axis',(0.,0.,1.));
#12089=DIRECTION('ref_axis',(-1.,-7.2244869017417E-14,0.));
#12090=DIRECTION('',(-1.22464679914735E-16,-8.86244235752658E-30,1.));
#12091=DIRECTION('center_axis',(0.,0.,1.));
#12092=DIRECTION('ref_axis',(-1.,-7.2244869017417E-14,0.));
#12093=DIRECTION('',(-1.22464679914735E-16,-8.86244235752658E-30,1.));
#12094=DIRECTION('center_axis',(0.,0.,1.));
#12095=DIRECTION('ref_axis',(-1.,-7.2244869017417E-14,0.));
#12096=DIRECTION('',(-1.22464679914735E-16,-8.86244235752658E-30,1.));
#12097=DIRECTION('center_axis',(0.,0.,1.));
#12098=DIRECTION('ref_axis',(-1.,-7.2244869017417E-14,0.));
#12099=DIRECTION('',(-1.22464679914735E-16,-8.86244235752658E-30,1.));
#12100=DIRECTION('center_axis',(0.,0.,1.));
#12101=DIRECTION('ref_axis',(-1.,-7.2244869017417E-14,0.));
#12102=DIRECTION('',(-1.22464679914735E-16,-8.86244235752658E-30,1.));
#12103=DIRECTION('center_axis',(0.,0.,1.));
#12104=DIRECTION('ref_axis',(-1.,-7.2244869017417E-14,0.));
#12105=DIRECTION('',(-1.22464679914735E-16,-8.86244235752658E-30,1.));
#12106=DIRECTION('center_axis',(0.,0.,1.));
#12107=DIRECTION('ref_axis',(-1.,-7.2244869017417E-14,0.));
#12108=DIRECTION('',(-1.22464679914735E-16,-8.86244235752658E-30,1.));
#12109=DIRECTION('center_axis',(0.,0.,1.));
#12110=DIRECTION('ref_axis',(-1.,-7.2244869017417E-14,0.));
#12111=DIRECTION('',(-1.22464679914735E-16,-8.86244235752658E-30,1.));
#12112=DIRECTION('center_axis',(0.,0.,1.));
#12113=DIRECTION('ref_axis',(-1.,-7.2244869017417E-14,0.));
#12114=DIRECTION('',(-1.22464679914735E-16,-8.86244235752658E-30,1.));
#12115=DIRECTION('center_axis',(0.,0.,1.));
#12116=DIRECTION('ref_axis',(-1.,-7.2244869017417E-14,0.));
#12117=DIRECTION('',(-1.22464679914735E-16,-8.86244235752658E-30,1.));
#12118=DIRECTION('center_axis',(0.,0.,1.));
#12119=DIRECTION('ref_axis',(-1.,-7.2244869017417E-14,0.));
#12120=DIRECTION('',(-1.22464679914735E-16,-8.86244235752658E-30,1.));
#12121=DIRECTION('center_axis',(0.,0.,1.));
#12122=DIRECTION('ref_axis',(-1.,-7.2244869017417E-14,0.));
#12123=DIRECTION('',(-1.22464679914735E-16,-8.86244235752658E-30,1.));
#12124=DIRECTION('center_axis',(0.,0.,1.));
#12125=DIRECTION('ref_axis',(-1.,-7.2244869017417E-14,0.));
#12126=DIRECTION('',(-1.22464679914735E-16,-8.86244235752658E-30,1.));
#12127=DIRECTION('center_axis',(0.,0.,1.));
#12128=DIRECTION('ref_axis',(0.609168734065488,-0.79304063794805,0.));
#12129=DIRECTION('',(-1.22464679914735E-16,-8.86244235752658E-30,1.));
#12130=DIRECTION('center_axis',(0.,0.,1.));
#12131=DIRECTION('ref_axis',(-1.,-7.2244869017417E-14,0.));
#12132=DIRECTION('center_axis',(0.,0.,1.));
#12133=DIRECTION('ref_axis',(0.935988336829059,0.352031011872493,0.));
#12134=DIRECTION('',(0.,0.,-1.));
#12135=DIRECTION('center_axis',(0.,0.,1.));
#12136=DIRECTION('ref_axis',(1.,0.,0.));
#12137=DIRECTION('center_axis',(0.,0.,1.));
#12138=DIRECTION('ref_axis',(1.,0.,0.));
#12139=DIRECTION('',(0.,0.,-1.));
#12140=DIRECTION('center_axis',(0.,0.,1.));
#12141=DIRECTION('ref_axis',(1.,0.,0.));
#12142=DIRECTION('',(0.,0.,-1.));
#12143=DIRECTION('center_axis',(0.,0.,1.));
#12144=DIRECTION('ref_axis',(1.,0.,0.));
#12145=DIRECTION('',(0.,0.,-1.));
#12146=DIRECTION('center_axis',(0.,0.,1.));
#12147=DIRECTION('ref_axis',(1.,0.,0.));
#12148=DIRECTION('',(0.,0.,-1.));
#12149=DIRECTION('center_axis',(0.,0.,1.));
#12150=DIRECTION('ref_axis',(1.,0.,0.));
#12151=DIRECTION('',(0.,0.,-1.));
#12152=DIRECTION('center_axis',(0.,0.,1.));
#12153=DIRECTION('ref_axis',(1.,0.,0.));
#12154=DIRECTION('',(0.,0.,-1.));
#12155=DIRECTION('center_axis',(0.,0.,1.));
#12156=DIRECTION('ref_axis',(1.,0.,0.));
#12157=DIRECTION('',(0.,0.,-1.));
#12158=DIRECTION('center_axis',(0.,0.,-1.));
#12159=DIRECTION('ref_axis',(1.,0.,0.));
#12160=DIRECTION('center_axis',(0.,0.,1.));
#12161=DIRECTION('ref_axis',(1.,2.7012746630748E-14,0.));
#12162=DIRECTION('',(1.22464679914735E-16,3.32310496757901E-30,1.));
#12163=DIRECTION('center_axis',(0.,0.,-1.));
#12164=DIRECTION('ref_axis',(1.,2.7012746630748E-14,0.));
#12165=DIRECTION('center_axis',(0.,0.,1.));
#12166=DIRECTION('ref_axis',(1.,2.7012746630748E-14,0.));
#12167=DIRECTION('',(1.22464679914735E-16,3.32310496757901E-30,1.));
#12168=DIRECTION('center_axis',(0.,0.,1.));
#12169=DIRECTION('ref_axis',(1.,2.7012746630748E-14,0.));
#12170=DIRECTION('',(1.22464679914735E-16,3.32310496757901E-30,1.));
#12171=DIRECTION('center_axis',(0.,0.,1.));
#12172=DIRECTION('ref_axis',(1.,2.7012746630748E-14,0.));
#12173=DIRECTION('',(1.22464679914735E-16,3.32310496757901E-30,1.));
#12174=DIRECTION('center_axis',(0.,0.,1.));
#12175=DIRECTION('ref_axis',(1.,2.7012746630748E-14,0.));
#12176=DIRECTION('',(1.22464679914735E-16,3.32310496757901E-30,1.));
#12177=DIRECTION('center_axis',(0.,0.,1.));
#12178=DIRECTION('ref_axis',(1.,2.7012746630748E-14,0.));
#12179=DIRECTION('',(1.22464679914735E-16,3.32310496757901E-30,1.));
#12180=DIRECTION('center_axis',(0.,0.,1.));
#12181=DIRECTION('ref_axis',(1.,2.7012746630748E-14,0.));
#12182=DIRECTION('',(1.22464679914735E-16,3.32310496757901E-30,1.));
#12183=DIRECTION('center_axis',(0.,0.,1.));
#12184=DIRECTION('ref_axis',(-0.608508919018736,0.79354703419183,0.));
#12185=DIRECTION('',(1.22464679914735E-16,3.32310496757901E-30,1.));
#12186=DIRECTION('center_axis',(0.,0.,1.));
#12187=DIRECTION('ref_axis',(1.,2.7012746630748E-14,0.));
#12188=DIRECTION('center_axis',(0.,0.,1.));
#12189=DIRECTION('ref_axis',(1.,2.7012746630748E-14,0.));
#12190=DIRECTION('center_axis',(0.,0.,1.));
#12191=DIRECTION('ref_axis',(1.,0.,0.));
#12192=DIRECTION('center_axis',(0.,0.,1.));
#12193=DIRECTION('ref_axis',(1.,0.,0.));
#12194=DIRECTION('center_axis',(0.,0.,1.));
#12195=DIRECTION('ref_axis',(1.,0.,0.));
#12196=DIRECTION('center_axis',(0.,0.,1.));
#12197=DIRECTION('ref_axis',(1.,0.,0.));
#12198=DIRECTION('center_axis',(0.,0.,1.));
#12199=DIRECTION('ref_axis',(1.,0.,0.));
#12200=DIRECTION('',(0.,0.,-1.));
#12201=DIRECTION('center_axis',(0.,0.,1.));
#12202=DIRECTION('ref_axis',(1.,0.,0.));
#12203=DIRECTION('',(0.,1.,0.));
#12204=DIRECTION('',(1.,0.,0.));
#12205=DIRECTION('',(0.,1.,0.));
#12206=DIRECTION('',(-1.,0.,0.));
#12207=DIRECTION('center_axis',(0.,0.,1.));
#12208=DIRECTION('ref_axis',(1.,0.,0.));
#12209=DIRECTION('center_axis',(0.,0.,1.));
#12210=DIRECTION('ref_axis',(-1.,-7.2244869017417E-14,0.));
#12211=DIRECTION('center_axis',(0.,0.,1.));
#12212=DIRECTION('ref_axis',(-1.,0.,0.));
#12213=DIRECTION('center_axis',(0.,0.,1.));
#12214=DIRECTION('ref_axis',(1.,0.,0.));
#12215=DIRECTION('center_axis',(0.,0.,1.));
#12216=DIRECTION('ref_axis',(-1.,-7.80244585388104E-14,0.));
#12217=DIRECTION('center_axis',(0.,0.,1.));
#12218=DIRECTION('ref_axis',(-1.,0.,0.));
#12219=DIRECTION('center_axis',(0.,0.,1.));
#12220=DIRECTION('ref_axis',(1.,0.,0.));
#12221=DIRECTION('',(1.,0.,0.));
#12222=DIRECTION('center_axis',(0.,0.,1.));
#12223=DIRECTION('ref_axis',(1.,0.,0.));
#12224=DIRECTION('',(1.,0.,0.));
#12225=DIRECTION('',(1.,0.,0.));
#12226=DIRECTION('center_axis',(0.,0.,-1.));
#12227=DIRECTION('ref_axis',(-1.,0.,0.));
#12228=DIRECTION('center_axis',(0.,0.,1.));
#12229=DIRECTION('ref_axis',(1.,0.,0.));
#12230=DIRECTION('',(1.,0.,0.));
#12231=DIRECTION('center_axis',(0.,0.,1.));
#12232=DIRECTION('ref_axis',(-1.,-7.80244585388103E-14,0.));
#12233=DIRECTION('center_axis',(0.,0.,1.));
#12234=DIRECTION('ref_axis',(-1.,0.,0.));
#12235=DIRECTION('center_axis',(0.,0.,1.));
#12236=DIRECTION('ref_axis',(1.,0.,0.));
#12237=DIRECTION('',(1.,0.,0.));
#12238=DIRECTION('center_axis',(0.,0.,1.));
#12239=DIRECTION('ref_axis',(1.,0.,0.));
#12240=DIRECTION('',(1.,0.,0.));
#12241=DIRECTION('',(1.,0.,0.));
#12242=DIRECTION('center_axis',(0.,0.,-1.));
#12243=DIRECTION('ref_axis',(-1.,0.,0.));
#12244=DIRECTION('center_axis',(0.,0.,1.));
#12245=DIRECTION('ref_axis',(1.,0.,0.));
#12246=DIRECTION('',(1.,0.,0.));
#12247=DIRECTION('center_axis',(0.,0.,1.));
#12248=DIRECTION('ref_axis',(-1.,-7.80244585388103E-14,0.));
#12249=DIRECTION('center_axis',(0.,0.,1.));
#12250=DIRECTION('ref_axis',(-1.,0.,0.));
#12251=DIRECTION('center_axis',(0.,0.,1.));
#12252=DIRECTION('ref_axis',(-1.,0.,0.));
#12253=DIRECTION('center_axis',(0.,0.,1.));
#12254=DIRECTION('ref_axis',(-1.,0.,0.));
#12255=DIRECTION('center_axis',(0.,0.,1.));
#12256=DIRECTION('ref_axis',(-1.,0.,0.));
#12257=DIRECTION('center_axis',(0.,0.,1.));
#12258=DIRECTION('ref_axis',(-1.,0.,0.));
#12259=DIRECTION('center_axis',(0.,0.,1.));
#12260=DIRECTION('ref_axis',(1.,0.,0.));
#12261=DIRECTION('center_axis',(0.,0.,-1.));
#12262=DIRECTION('ref_axis',(1.,-8.21286773296138E-14,0.));
#12263=DIRECTION('center_axis',(0.,0.,-1.));
#12264=DIRECTION('ref_axis',(1.,0.,0.));
#12265=DIRECTION('center_axis',(0.,0.,1.));
#12266=DIRECTION('ref_axis',(1.,0.,0.));
#12267=DIRECTION('center_axis',(0.,0.,-1.));
#12268=DIRECTION('ref_axis',(1.,-8.21286773296134E-14,0.));
#12269=DIRECTION('center_axis',(0.,0.,-1.));
#12270=DIRECTION('ref_axis',(1.,0.,0.));
#12271=DIRECTION('center_axis',(0.,0.,1.));
#12272=DIRECTION('ref_axis',(1.,0.,0.));
#12273=DIRECTION('center_axis',(0.,0.,-1.));
#12274=DIRECTION('ref_axis',(1.,-6.48384294707476E-14,0.));
#12275=DIRECTION('center_axis',(0.,0.,-1.));
#12276=DIRECTION('ref_axis',(1.,0.,0.));
#12277=DIRECTION('center_axis',(0.,0.,1.));
#12278=DIRECTION('ref_axis',(1.,0.,0.));
#12279=DIRECTION('center_axis',(0.,0.,-1.));
#12280=DIRECTION('ref_axis',(1.,-7.34835534001804E-14,0.));
#12281=DIRECTION('center_axis',(0.,0.,-1.));
#12282=DIRECTION('ref_axis',(1.,0.,0.));
#12283=DIRECTION('center_axis',(0.,0.,-1.));
#12284=DIRECTION('ref_axis',(1.,0.,0.));
#12285=DIRECTION('center_axis',(0.,0.,-1.));
#12286=DIRECTION('ref_axis',(1.,0.,0.));
#12287=DIRECTION('center_axis',(0.,0.,-1.));
#12288=DIRECTION('ref_axis',(1.,0.,0.));
#12289=DIRECTION('center_axis',(0.,0.,-1.));
#12290=DIRECTION('ref_axis',(1.,0.,0.));
#12291=DIRECTION('center_axis',(-1.,0.,0.));
#12292=DIRECTION('ref_axis',(0.,1.,0.));
#12293=DIRECTION('center_axis',(-1.,0.,0.));
#12294=DIRECTION('ref_axis',(0.,1.,0.));
#12295=DIRECTION('',(-1.,0.,0.));
#12296=DIRECTION('center_axis',(1.,0.,0.));
#12297=DIRECTION('ref_axis',(0.,1.,0.));
#12298=DIRECTION('center_axis',(-1.,0.,0.));
#12299=DIRECTION('ref_axis',(0.,1.,0.));
#12300=DIRECTION('center_axis',(-1.,0.,0.));
#12301=DIRECTION('ref_axis',(0.,1.,0.));
#12302=DIRECTION('',(-1.,0.,0.));
#12303=DIRECTION('center_axis',(1.,0.,0.));
#12304=DIRECTION('ref_axis',(0.,1.,0.));
#12305=DIRECTION('center_axis',(-1.,0.,0.));
#12306=DIRECTION('ref_axis',(0.,1.,0.));
#12307=DIRECTION('center_axis',(-1.,0.,0.));
#12308=DIRECTION('ref_axis',(0.,1.,0.));
#12309=DIRECTION('',(-1.,0.,0.));
#12310=DIRECTION('center_axis',(1.,0.,0.));
#12311=DIRECTION('ref_axis',(0.,1.,0.));
#12312=DIRECTION('center_axis',(-1.,0.,0.));
#12313=DIRECTION('ref_axis',(0.,1.,0.));
#12314=DIRECTION('center_axis',(-1.,0.,0.));
#12315=DIRECTION('ref_axis',(0.,1.,0.));
#12316=DIRECTION('',(-1.,0.,0.));
#12317=DIRECTION('center_axis',(1.,0.,0.));
#12318=DIRECTION('ref_axis',(0.,1.,0.));
#12319=DIRECTION('center_axis',(-1.,0.,0.));
#12320=DIRECTION('ref_axis',(0.,1.,0.));
#12321=DIRECTION('center_axis',(-1.,0.,0.));
#12322=DIRECTION('ref_axis',(0.,1.,0.));
#12323=DIRECTION('',(-1.,0.,0.));
#12324=DIRECTION('center_axis',(1.,0.,0.));
#12325=DIRECTION('ref_axis',(0.,1.,0.));
#12326=DIRECTION('center_axis',(-1.,0.,0.));
#12327=DIRECTION('ref_axis',(0.,1.,0.));
#12328=DIRECTION('center_axis',(-1.,0.,0.));
#12329=DIRECTION('ref_axis',(0.,1.,0.));
#12330=DIRECTION('',(-1.,0.,0.));
#12331=DIRECTION('center_axis',(1.,0.,0.));
#12332=DIRECTION('ref_axis',(0.,1.,0.));
#12333=DIRECTION('center_axis',(-1.,0.,0.));
#12334=DIRECTION('ref_axis',(0.,1.,0.));
#12335=DIRECTION('center_axis',(-1.,0.,0.));
#12336=DIRECTION('ref_axis',(0.,1.,0.));
#12337=DIRECTION('',(-1.,0.,0.));
#12338=DIRECTION('center_axis',(1.,0.,0.));
#12339=DIRECTION('ref_axis',(0.,1.,0.));
#12340=DIRECTION('center_axis',(-1.,0.,0.));
#12341=DIRECTION('ref_axis',(0.,1.,0.));
#12342=DIRECTION('center_axis',(-1.,0.,0.));
#12343=DIRECTION('ref_axis',(0.,1.,0.));
#12344=DIRECTION('',(-1.,0.,0.));
#12345=DIRECTION('center_axis',(1.,0.,0.));
#12346=DIRECTION('ref_axis',(0.,1.,0.));
#12347=DIRECTION('center_axis',(-1.,0.,0.));
#12348=DIRECTION('ref_axis',(0.,3.3690166589284E-15,1.));
#12349=DIRECTION('center_axis',(-1.,0.,0.));
#12350=DIRECTION('ref_axis',(0.,1.,0.));
#12351=DIRECTION('',(-1.,0.,0.));
#12352=DIRECTION('',(-1.,0.,0.));
#12353=DIRECTION('center_axis',(1.,0.,0.));
#12354=DIRECTION('ref_axis',(0.,1.,0.));
#12355=DIRECTION('center_axis',(-1.,0.,0.));
#12356=DIRECTION('ref_axis',(0.,1.,0.));
#12357=DIRECTION('center_axis',(-1.,0.,0.));
#12358=DIRECTION('ref_axis',(0.,1.,0.));
#12359=DIRECTION('',(-1.,0.,0.));
#12360=DIRECTION('center_axis',(1.,0.,0.));
#12361=DIRECTION('ref_axis',(0.,1.,0.));
#12362=DIRECTION('center_axis',(-1.,0.,0.));
#12363=DIRECTION('ref_axis',(0.,1.,0.));
#12364=DIRECTION('center_axis',(-1.,0.,0.));
#12365=DIRECTION('ref_axis',(0.,1.,0.));
#12366=DIRECTION('',(-1.,0.,0.));
#12367=DIRECTION('center_axis',(1.,0.,0.));
#12368=DIRECTION('ref_axis',(0.,1.,0.));
#12369=DIRECTION('center_axis',(-1.,0.,0.));
#12370=DIRECTION('ref_axis',(0.,1.,0.));
#12371=DIRECTION('center_axis',(-1.,0.,0.));
#12372=DIRECTION('ref_axis',(0.,1.,0.));
#12373=DIRECTION('',(-1.,0.,0.));
#12374=DIRECTION('center_axis',(1.,0.,0.));
#12375=DIRECTION('ref_axis',(0.,1.,0.));
#12376=DIRECTION('center_axis',(-1.,0.,0.));
#12377=DIRECTION('ref_axis',(0.,1.,0.));
#12378=DIRECTION('center_axis',(-1.,0.,0.));
#12379=DIRECTION('ref_axis',(0.,1.,0.));
#12380=DIRECTION('',(-1.,0.,0.));
#12381=DIRECTION('center_axis',(1.,0.,0.));
#12382=DIRECTION('ref_axis',(0.,1.,0.));
#12383=DIRECTION('center_axis',(-1.,0.,0.));
#12384=DIRECTION('ref_axis',(0.,1.,0.));
#12385=DIRECTION('center_axis',(-1.,0.,0.));
#12386=DIRECTION('ref_axis',(0.,1.,0.));
#12387=DIRECTION('',(-1.,0.,0.));
#12388=DIRECTION('center_axis',(1.,0.,0.));
#12389=DIRECTION('ref_axis',(0.,1.,0.));
#12390=DIRECTION('center_axis',(-1.,0.,0.));
#12391=DIRECTION('ref_axis',(0.,1.,0.));
#12392=DIRECTION('center_axis',(-1.,0.,0.));
#12393=DIRECTION('ref_axis',(0.,1.,0.));
#12394=DIRECTION('',(-1.,0.,0.));
#12395=DIRECTION('center_axis',(1.,0.,0.));
#12396=DIRECTION('ref_axis',(0.,1.,0.));
#12397=DIRECTION('center_axis',(-1.,0.,0.));
#12398=DIRECTION('ref_axis',(0.,1.,0.));
#12399=DIRECTION('center_axis',(-1.,0.,0.));
#12400=DIRECTION('ref_axis',(0.,1.,0.));
#12401=DIRECTION('',(-1.,0.,0.));
#12402=DIRECTION('center_axis',(1.,0.,0.));
#12403=DIRECTION('ref_axis',(0.,1.,0.));
#12404=DIRECTION('center_axis',(-1.,0.,0.));
#12405=DIRECTION('ref_axis',(0.,-3.7364106986726E-15,1.));
#12406=DIRECTION('center_axis',(-1.,0.,0.));
#12407=DIRECTION('ref_axis',(0.,1.,0.));
#12408=DIRECTION('',(-1.,0.,0.));
#12409=DIRECTION('',(-1.,0.,0.));
#12410=DIRECTION('center_axis',(1.,0.,0.));
#12411=DIRECTION('ref_axis',(0.,1.,0.));
#12412=DIRECTION('center_axis',(-1.,0.,0.));
#12413=DIRECTION('ref_axis',(0.,1.,0.));
#12414=DIRECTION('center_axis',(-1.,0.,0.));
#12415=DIRECTION('ref_axis',(0.,1.,0.));
#12416=DIRECTION('',(-1.,0.,0.));
#12417=DIRECTION('center_axis',(1.,0.,0.));
#12418=DIRECTION('ref_axis',(0.,1.,0.));
#12419=DIRECTION('center_axis',(0.,-1.,0.));
#12420=DIRECTION('ref_axis',(-1.,0.,0.));
#12421=DIRECTION('',(-1.,0.,0.));
#12422=DIRECTION('',(0.,0.,-1.));
#12423=DIRECTION('',(-1.,0.,0.));
#12424=DIRECTION('',(0.,0.,-1.));
#12425=DIRECTION('center_axis',(1.,0.,0.));
#12426=DIRECTION('ref_axis',(0.,-1.,0.));
#12427=DIRECTION('',(0.,-1.,0.));
#12428=DIRECTION('',(0.,0.,-1.));
#12429=DIRECTION('',(0.,-1.,0.));
#12430=DIRECTION('center_axis',(0.,1.,0.));
#12431=DIRECTION('ref_axis',(1.,0.,0.));
#12432=DIRECTION('',(1.,0.,0.));
#12433=DIRECTION('',(0.,0.,-1.));
#12434=DIRECTION('',(1.,0.,0.));
#12435=DIRECTION('center_axis',(-1.,0.,0.));
#12436=DIRECTION('ref_axis',(0.,1.,0.));
#12437=DIRECTION('',(0.,1.,0.));
#12438=DIRECTION('',(0.,1.,0.));
#12439=DIRECTION('center_axis',(0.,0.,-1.));
#12440=DIRECTION('ref_axis',(-1.,0.,0.));
#12441=DIRECTION('center_axis',(0.,1.,0.));
#12442=DIRECTION('ref_axis',(-1.,0.,0.));
#12443=DIRECTION('',(0.,0.,1.));
#12444=DIRECTION('',(1.,0.,0.));
#12445=DIRECTION('',(0.,0.,-1.));
#12446=DIRECTION('center_axis',(1.,0.,0.));
#12447=DIRECTION('ref_axis',(0.,1.,0.));
#12448=DIRECTION('',(0.,1.,0.));
#12449=DIRECTION('',(0.,0.,1.));
#12450=DIRECTION('center_axis',(0.,-1.,0.));
#12451=DIRECTION('ref_axis',(1.,0.,0.));
#12452=DIRECTION('',(-1.,0.,0.));
#12453=DIRECTION('',(0.,0.,-1.));
#12454=DIRECTION('center_axis',(-1.,0.,0.));
#12455=DIRECTION('ref_axis',(0.,-1.,0.));
#12456=DIRECTION('',(0.,1.,0.));
#12457=DIRECTION('center_axis',(0.,0.,1.));
#12458=DIRECTION('ref_axis',(1.,0.,0.));
#12459=DIRECTION('axis',(0.,0.,1.));
#12460=DIRECTION('refdir',(1.,0.,0.));
#12461=DIRECTION('center_axis',(0.,0.,-1.));
#12462=DIRECTION('ref_axis',(1.,0.,0.));
#12463=DIRECTION('center_axis',(0.,0.,-1.));
#12464=DIRECTION('ref_axis',(1.,0.,0.));
#12465=DIRECTION('',(0.,0.,-1.));
#12466=DIRECTION('center_axis',(0.,0.,1.));
#12467=DIRECTION('ref_axis',(1.,0.,0.));
#12468=DIRECTION('center_axis',(0.,0.,-1.));
#12469=DIRECTION('ref_axis',(1.,0.,0.));
#12470=DIRECTION('center_axis',(0.,0.,-1.));
#12471=DIRECTION('ref_axis',(1.,0.,0.));
#12472=DIRECTION('',(0.,0.,-1.));
#12473=DIRECTION('center_axis',(0.,0.,1.));
#12474=DIRECTION('ref_axis',(1.,0.,0.));
#12475=DIRECTION('center_axis',(0.,0.,-1.));
#12476=DIRECTION('ref_axis',(1.,0.,0.));
#12477=DIRECTION('center_axis',(0.,0.,-1.));
#12478=DIRECTION('ref_axis',(1.,0.,0.));
#12479=DIRECTION('',(0.,0.,-1.));
#12480=DIRECTION('center_axis',(0.,0.,1.));
#12481=DIRECTION('ref_axis',(1.,0.,0.));
#12482=DIRECTION('center_axis',(0.,0.,-1.));
#12483=DIRECTION('ref_axis',(1.,0.,0.));
#12484=DIRECTION('center_axis',(0.,0.,-1.));
#12485=DIRECTION('ref_axis',(1.,0.,0.));
#12486=DIRECTION('',(0.,0.,-1.));
#12487=DIRECTION('center_axis',(0.,0.,1.));
#12488=DIRECTION('ref_axis',(1.,0.,0.));
#12489=DIRECTION('center_axis',(0.,1.,0.));
#12490=DIRECTION('ref_axis',(-1.,0.,0.));
#12491=DIRECTION('',(-1.,0.,0.));
#12492=DIRECTION('',(0.,0.,1.));
#12493=DIRECTION('',(-1.,0.,0.));
#12494=DIRECTION('',(0.,0.,1.));
#12495=DIRECTION('center_axis',(1.,0.,0.));
#12496=DIRECTION('ref_axis',(0.,1.,0.));
#12497=DIRECTION('',(0.,1.,0.));
#12498=DIRECTION('',(0.,1.,0.));
#12499=DIRECTION('',(0.,0.,1.));
#12500=DIRECTION('center_axis',(0.,-1.,0.));
#12501=DIRECTION('ref_axis',(1.,0.,0.));
#12502=DIRECTION('',(1.,0.,0.));
#12503=DIRECTION('',(1.,0.,0.));
#12504=DIRECTION('',(0.,0.,1.));
#12505=DIRECTION('center_axis',(-1.,0.,0.));
#12506=DIRECTION('ref_axis',(0.,-1.,0.));
#12507=DIRECTION('',(0.,-1.,0.));
#12508=DIRECTION('',(0.,-1.,0.));
#12509=DIRECTION('center_axis',(0.,0.,1.));
#12510=DIRECTION('ref_axis',(1.,0.,0.));
#12511=DIRECTION('center_axis',(0.,0.,1.));
#12512=DIRECTION('ref_axis',(1.,0.,0.));
#12513=DIRECTION('axis',(0.,0.,1.));
#12514=DIRECTION('refdir',(1.,0.,0.));
#12515=DIRECTION('center_axis',(0.,0.,-1.));
#12516=DIRECTION('ref_axis',(1.,0.,0.));
#12517=DIRECTION('center_axis',(0.,0.,-1.));
#12518=DIRECTION('ref_axis',(1.,0.,0.));
#12519=DIRECTION('',(0.,0.,-1.));
#12520=DIRECTION('center_axis',(0.,0.,1.));
#12521=DIRECTION('ref_axis',(1.,0.,0.));
#12522=DIRECTION('center_axis',(0.,0.,-1.));
#12523=DIRECTION('ref_axis',(1.,0.,0.));
#12524=DIRECTION('center_axis',(0.,0.,-1.));
#12525=DIRECTION('ref_axis',(1.,0.,0.));
#12526=DIRECTION('',(0.,0.,-1.));
#12527=DIRECTION('center_axis',(0.,0.,1.));
#12528=DIRECTION('ref_axis',(1.,0.,0.));
#12529=DIRECTION('center_axis',(0.,0.,-1.));
#12530=DIRECTION('ref_axis',(1.,0.,0.));
#12531=DIRECTION('center_axis',(0.,0.,-1.));
#12532=DIRECTION('ref_axis',(1.,0.,0.));
#12533=DIRECTION('',(0.,0.,-1.));
#12534=DIRECTION('center_axis',(0.,0.,1.));
#12535=DIRECTION('ref_axis',(1.,0.,0.));
#12536=DIRECTION('center_axis',(0.,0.,-1.));
#12537=DIRECTION('ref_axis',(1.,0.,0.));
#12538=DIRECTION('center_axis',(0.,0.,-1.));
#12539=DIRECTION('ref_axis',(1.,0.,0.));
#12540=DIRECTION('',(0.,0.,-1.));
#12541=DIRECTION('center_axis',(0.,0.,1.));
#12542=DIRECTION('ref_axis',(1.,0.,0.));
#12543=DIRECTION('center_axis',(0.,-1.,0.));
#12544=DIRECTION('ref_axis',(-1.,0.,0.));
#12545=DIRECTION('',(-1.,0.,0.));
#12546=DIRECTION('',(0.,0.,-1.));
#12547=DIRECTION('',(1.,0.,0.));
#12548=DIRECTION('',(0.,0.,-1.));
#12549=DIRECTION('center_axis',(1.,0.,0.));
#12550=DIRECTION('ref_axis',(0.,-1.,0.));
#12551=DIRECTION('',(0.,-1.,0.));
#12552=DIRECTION('',(0.,0.,-1.));
#12553=DIRECTION('',(0.,1.,0.));
#12554=DIRECTION('center_axis',(0.,1.,0.));
#12555=DIRECTION('ref_axis',(1.,0.,0.));
#12556=DIRECTION('',(1.,0.,0.));
#12557=DIRECTION('',(0.,0.,-1.));
#12558=DIRECTION('',(-1.,0.,0.));
#12559=DIRECTION('center_axis',(-1.,0.,0.));
#12560=DIRECTION('ref_axis',(0.,1.,0.));
#12561=DIRECTION('',(0.,1.,0.));
#12562=DIRECTION('',(0.,-1.,0.));
#12563=DIRECTION('center_axis',(0.,1.,0.));
#12564=DIRECTION('ref_axis',(-1.,0.,0.));
#12565=DIRECTION('',(-1.,0.,0.));
#12566=DIRECTION('',(0.,0.,1.));
#12567=DIRECTION('',(-1.,0.,0.));
#12568=DIRECTION('',(0.,0.,1.));
#12569=DIRECTION('center_axis',(1.,0.,0.));
#12570=DIRECTION('ref_axis',(0.,1.,0.));
#12571=DIRECTION('',(0.,1.,0.));
#12572=DIRECTION('',(0.,1.,0.));
#12573=DIRECTION('',(0.,0.,1.));
#12574=DIRECTION('center_axis',(0.,-1.,0.));
#12575=DIRECTION('ref_axis',(1.,0.,0.));
#12576=DIRECTION('',(1.,0.,0.));
#12577=DIRECTION('',(1.,0.,0.));
#12578=DIRECTION('',(0.,0.,1.));
#12579=DIRECTION('center_axis',(-1.,0.,0.));
#12580=DIRECTION('ref_axis',(0.,-1.,0.));
#12581=DIRECTION('',(0.,-1.,0.));
#12582=DIRECTION('',(0.,-1.,0.));
#12583=DIRECTION('center_axis',(0.,0.,1.));
#12584=DIRECTION('ref_axis',(1.,0.,0.));
#12585=DIRECTION('center_axis',(0.,0.,1.));
#12586=DIRECTION('ref_axis',(1.,0.,0.));
#12587=DIRECTION('axis',(0.,0.,1.));
#12588=DIRECTION('refdir',(1.,0.,0.));
#12589=DIRECTION('center_axis',(0.,0.,1.));
#12590=DIRECTION('ref_axis',(1.,0.,0.));
#12591=DIRECTION('center_axis',(0.,0.,-1.));
#12592=DIRECTION('ref_axis',(1.,0.,0.));
#12593=DIRECTION('',(0.,0.,-1.));
#12594=DIRECTION('center_axis',(0.,0.,-1.));
#12595=DIRECTION('ref_axis',(1.,0.,0.));
#12596=DIRECTION('center_axis',(0.,0.,1.));
#12597=DIRECTION('ref_axis',(1.,0.,0.));
#12598=DIRECTION('center_axis',(0.,0.,1.));
#12599=DIRECTION('ref_axis',(1.,0.,0.));
#12600=DIRECTION('',(0.,0.,-1.));
#12601=DIRECTION('center_axis',(0.,0.,1.));
#12602=DIRECTION('ref_axis',(1.,0.,0.));
#12603=DIRECTION('center_axis',(0.,0.,1.));
#12604=DIRECTION('ref_axis',(1.,0.,0.));
#12605=DIRECTION('center_axis',(0.,0.,1.));
#12606=DIRECTION('ref_axis',(1.,0.,0.));
#12607=DIRECTION('axis',(0.,0.,1.));
#12608=DIRECTION('refdir',(1.,0.,0.));
#12609=DIRECTION('center_axis',(0.,0.,-1.));
#12610=DIRECTION('ref_axis',(1.,0.,0.));
#12611=DIRECTION('center_axis',(0.,0.,-1.));
#12612=DIRECTION('ref_axis',(1.,0.,0.));
#12613=DIRECTION('',(0.,0.,-1.));
#12614=DIRECTION('center_axis',(0.,0.,1.));
#12615=DIRECTION('ref_axis',(1.,0.,0.));
#12616=DIRECTION('center_axis',(0.,0.,-1.));
#12617=DIRECTION('ref_axis',(1.,0.,0.));
#12618=DIRECTION('center_axis',(0.,0.,-1.));
#12619=DIRECTION('ref_axis',(1.,0.,0.));
#12620=DIRECTION('',(0.,0.,-1.));
#12621=DIRECTION('center_axis',(0.,0.,1.));
#12622=DIRECTION('ref_axis',(1.,0.,0.));
#12623=DIRECTION('center_axis',(0.,0.,-1.));
#12624=DIRECTION('ref_axis',(1.,0.,0.));
#12625=DIRECTION('center_axis',(0.,0.,-1.));
#12626=DIRECTION('ref_axis',(1.,0.,0.));
#12627=DIRECTION('',(0.,0.,-1.));
#12628=DIRECTION('center_axis',(0.,0.,1.));
#12629=DIRECTION('ref_axis',(1.,0.,0.));
#12630=DIRECTION('center_axis',(0.,0.,-1.));
#12631=DIRECTION('ref_axis',(1.,0.,0.));
#12632=DIRECTION('center_axis',(0.,0.,-1.));
#12633=DIRECTION('ref_axis',(1.,0.,0.));
#12634=DIRECTION('',(0.,0.,-1.));
#12635=DIRECTION('center_axis',(0.,0.,1.));
#12636=DIRECTION('ref_axis',(1.,0.,0.));
#12637=DIRECTION('center_axis',(0.,0.,-1.));
#12638=DIRECTION('ref_axis',(1.,0.,0.));
#12639=DIRECTION('center_axis',(0.,0.,-1.));
#12640=DIRECTION('ref_axis',(1.,0.,0.));
#12641=DIRECTION('',(0.,0.,-1.));
#12642=DIRECTION('center_axis',(0.,0.,1.));
#12643=DIRECTION('ref_axis',(1.,0.,0.));
#12644=DIRECTION('center_axis',(0.,0.,-1.));
#12645=DIRECTION('ref_axis',(1.,0.,0.));
#12646=DIRECTION('center_axis',(0.,0.,-1.));
#12647=DIRECTION('ref_axis',(1.,0.,0.));
#12648=DIRECTION('',(0.,0.,-1.));
#12649=DIRECTION('center_axis',(0.,0.,1.));
#12650=DIRECTION('ref_axis',(1.,0.,0.));
#12651=DIRECTION('center_axis',(0.,0.,-1.));
#12652=DIRECTION('ref_axis',(1.,0.,0.));
#12653=DIRECTION('center_axis',(0.,0.,-1.));
#12654=DIRECTION('ref_axis',(1.,0.,0.));
#12655=DIRECTION('',(0.,0.,-1.));
#12656=DIRECTION('center_axis',(0.,0.,1.));
#12657=DIRECTION('ref_axis',(1.,0.,0.));
#12658=DIRECTION('center_axis',(0.,0.,-1.));
#12659=DIRECTION('ref_axis',(1.,0.,0.));
#12660=DIRECTION('center_axis',(0.,0.,-1.));
#12661=DIRECTION('ref_axis',(1.,0.,0.));
#12662=DIRECTION('',(0.,0.,-1.));
#12663=DIRECTION('center_axis',(0.,0.,1.));
#12664=DIRECTION('ref_axis',(1.,0.,0.));
#12665=DIRECTION('center_axis',(0.,0.,-1.));
#12666=DIRECTION('ref_axis',(1.,0.,0.));
#12667=DIRECTION('center_axis',(0.,0.,-1.));
#12668=DIRECTION('ref_axis',(1.,0.,0.));
#12669=DIRECTION('',(0.,0.,-1.));
#12670=DIRECTION('center_axis',(0.,0.,1.));
#12671=DIRECTION('ref_axis',(1.,0.,0.));
#12672=DIRECTION('center_axis',(0.,0.,-1.));
#12673=DIRECTION('ref_axis',(1.,0.,0.));
#12674=DIRECTION('center_axis',(0.,0.,-1.));
#12675=DIRECTION('ref_axis',(1.,0.,0.));
#12676=DIRECTION('',(0.,0.,-1.));
#12677=DIRECTION('center_axis',(0.,0.,1.));
#12678=DIRECTION('ref_axis',(1.,0.,0.));
#12679=DIRECTION('center_axis',(0.,0.,-1.));
#12680=DIRECTION('ref_axis',(1.,0.,0.));
#12681=DIRECTION('center_axis',(0.,0.,-1.));
#12682=DIRECTION('ref_axis',(1.,0.,0.));
#12683=DIRECTION('',(0.,0.,-1.));
#12684=DIRECTION('center_axis',(0.,0.,1.));
#12685=DIRECTION('ref_axis',(1.,0.,0.));
#12686=DIRECTION('center_axis',(0.,0.,-1.));
#12687=DIRECTION('ref_axis',(1.,0.,0.));
#12688=DIRECTION('center_axis',(0.,0.,-1.));
#12689=DIRECTION('ref_axis',(1.,0.,0.));
#12690=DIRECTION('',(0.,0.,-1.));
#12691=DIRECTION('center_axis',(0.,0.,1.));
#12692=DIRECTION('ref_axis',(1.,0.,0.));
#12693=DIRECTION('center_axis',(0.,0.,-1.));
#12694=DIRECTION('ref_axis',(1.,0.,0.));
#12695=DIRECTION('center_axis',(0.,0.,-1.));
#12696=DIRECTION('ref_axis',(1.,0.,0.));
#12697=DIRECTION('',(0.,0.,-1.));
#12698=DIRECTION('center_axis',(0.,0.,1.));
#12699=DIRECTION('ref_axis',(1.,0.,0.));
#12700=DIRECTION('center_axis',(0.,0.,-1.));
#12701=DIRECTION('ref_axis',(1.,0.,0.));
#12702=DIRECTION('center_axis',(0.,0.,-1.));
#12703=DIRECTION('ref_axis',(1.,0.,0.));
#12704=DIRECTION('',(0.,0.,-1.));
#12705=DIRECTION('center_axis',(0.,0.,1.));
#12706=DIRECTION('ref_axis',(1.,0.,0.));
#12707=DIRECTION('center_axis',(0.,0.,-1.));
#12708=DIRECTION('ref_axis',(1.,0.,0.));
#12709=DIRECTION('center_axis',(0.,0.,-1.));
#12710=DIRECTION('ref_axis',(1.,0.,0.));
#12711=DIRECTION('',(0.,0.,-1.));
#12712=DIRECTION('center_axis',(0.,0.,1.));
#12713=DIRECTION('ref_axis',(1.,0.,0.));
#12714=DIRECTION('center_axis',(0.,0.,-1.));
#12715=DIRECTION('ref_axis',(1.,0.,0.));
#12716=DIRECTION('center_axis',(0.,0.,-1.));
#12717=DIRECTION('ref_axis',(1.,0.,0.));
#12718=DIRECTION('',(0.,0.,-1.));
#12719=DIRECTION('center_axis',(0.,0.,1.));
#12720=DIRECTION('ref_axis',(1.,0.,0.));
#12721=DIRECTION('center_axis',(0.,0.,-1.));
#12722=DIRECTION('ref_axis',(1.,0.,0.));
#12723=DIRECTION('center_axis',(0.,0.,-1.));
#12724=DIRECTION('ref_axis',(1.,0.,0.));
#12725=DIRECTION('',(0.,0.,-1.));
#12726=DIRECTION('center_axis',(0.,0.,1.));
#12727=DIRECTION('ref_axis',(1.,0.,0.));
#12728=DIRECTION('center_axis',(0.,0.,-1.));
#12729=DIRECTION('ref_axis',(1.,0.,0.));
#12730=DIRECTION('center_axis',(0.,0.,-1.));
#12731=DIRECTION('ref_axis',(1.,0.,0.));
#12732=DIRECTION('',(0.,0.,-1.));
#12733=DIRECTION('center_axis',(0.,0.,1.));
#12734=DIRECTION('ref_axis',(1.,0.,0.));
#12735=DIRECTION('center_axis',(0.,1.,0.));
#12736=DIRECTION('ref_axis',(-1.,0.,0.));
#12737=DIRECTION('',(-1.,0.,0.));
#12738=DIRECTION('',(0.,0.,-1.));
#12739=DIRECTION('',(-1.,0.,0.));
#12740=DIRECTION('',(0.,0.,1.));
#12741=DIRECTION('center_axis',(1.,0.,0.));
#12742=DIRECTION('ref_axis',(0.,1.,0.));
#12743=DIRECTION('',(0.,-1.,0.));
#12744=DIRECTION('',(0.,-1.,0.));
#12745=DIRECTION('',(0.,0.,1.));
#12746=DIRECTION('center_axis',(0.,-1.,0.));
#12747=DIRECTION('ref_axis',(1.,0.,0.));
#12748=DIRECTION('',(-1.,0.,0.));
#12749=DIRECTION('',(-1.,0.,0.));
#12750=DIRECTION('',(0.,0.,-1.));
#12751=DIRECTION('center_axis',(-1.,0.,0.));
#12752=DIRECTION('ref_axis',(0.,-1.,0.));
#12753=DIRECTION('',(0.,1.,0.));
#12754=DIRECTION('',(0.,1.,0.));
#12755=DIRECTION('center_axis',(0.,0.,1.));
#12756=DIRECTION('ref_axis',(1.,0.,0.));
#12757=DIRECTION('center_axis',(0.,0.,1.));
#12758=DIRECTION('ref_axis',(1.,0.,0.));
#12759=DIRECTION('axis',(0.,0.,1.));
#12760=DIRECTION('refdir',(1.,0.,0.));
#12761=DIRECTION('center_axis',(0.,0.,-1.));
#12762=DIRECTION('ref_axis',(1.,0.,0.));
#12763=DIRECTION('center_axis',(0.,0.,-1.));
#12764=DIRECTION('ref_axis',(1.,0.,0.));
#12765=DIRECTION('',(0.,0.,-1.));
#12766=DIRECTION('center_axis',(0.,0.,1.));
#12767=DIRECTION('ref_axis',(1.,0.,0.));
#12768=DIRECTION('center_axis',(0.,0.,-1.));
#12769=DIRECTION('ref_axis',(1.,0.,0.));
#12770=DIRECTION('center_axis',(0.,0.,-1.));
#12771=DIRECTION('ref_axis',(1.,0.,0.));
#12772=DIRECTION('',(0.,0.,-1.));
#12773=DIRECTION('center_axis',(0.,0.,1.));
#12774=DIRECTION('ref_axis',(1.,0.,0.));
#12775=DIRECTION('center_axis',(0.,0.,-1.));
#12776=DIRECTION('ref_axis',(1.,0.,0.));
#12777=DIRECTION('center_axis',(0.,0.,-1.));
#12778=DIRECTION('ref_axis',(1.,0.,0.));
#12779=DIRECTION('',(0.,0.,-1.));
#12780=DIRECTION('center_axis',(0.,0.,1.));
#12781=DIRECTION('ref_axis',(1.,0.,0.));
#12782=DIRECTION('center_axis',(0.,0.,-1.));
#12783=DIRECTION('ref_axis',(1.,0.,0.));
#12784=DIRECTION('center_axis',(0.,0.,-1.));
#12785=DIRECTION('ref_axis',(1.,0.,0.));
#12786=DIRECTION('',(0.,0.,-1.));
#12787=DIRECTION('center_axis',(0.,0.,1.));
#12788=DIRECTION('ref_axis',(1.,0.,0.));
#12789=DIRECTION('center_axis',(0.,0.,-1.));
#12790=DIRECTION('ref_axis',(1.,0.,0.));
#12791=DIRECTION('center_axis',(0.,0.,-1.));
#12792=DIRECTION('ref_axis',(1.,0.,0.));
#12793=DIRECTION('',(0.,0.,-1.));
#12794=DIRECTION('center_axis',(0.,0.,1.));
#12795=DIRECTION('ref_axis',(1.,0.,0.));
#12796=DIRECTION('center_axis',(0.,0.,-1.));
#12797=DIRECTION('ref_axis',(1.,0.,0.));
#12798=DIRECTION('center_axis',(0.,0.,-1.));
#12799=DIRECTION('ref_axis',(1.,0.,0.));
#12800=DIRECTION('',(0.,0.,-1.));
#12801=DIRECTION('center_axis',(0.,0.,1.));
#12802=DIRECTION('ref_axis',(1.,0.,0.));
#12803=DIRECTION('center_axis',(0.,0.,-1.));
#12804=DIRECTION('ref_axis',(1.,0.,0.));
#12805=DIRECTION('center_axis',(0.,0.,-1.));
#12806=DIRECTION('ref_axis',(1.,0.,0.));
#12807=DIRECTION('',(0.,0.,-1.));
#12808=DIRECTION('center_axis',(0.,0.,1.));
#12809=DIRECTION('ref_axis',(1.,0.,0.));
#12810=DIRECTION('center_axis',(0.,1.,0.));
#12811=DIRECTION('ref_axis',(-1.,0.,0.));
#12812=DIRECTION('',(-1.,0.,0.));
#12813=DIRECTION('',(0.,0.,1.));
#12814=DIRECTION('',(-1.,0.,0.));
#12815=DIRECTION('',(0.,0.,1.));
#12816=DIRECTION('center_axis',(1.,0.,0.));
#12817=DIRECTION('ref_axis',(0.,1.,0.));
#12818=DIRECTION('',(0.,1.,0.));
#12819=DIRECTION('',(0.,1.,0.));
#12820=DIRECTION('',(0.,0.,1.));
#12821=DIRECTION('center_axis',(0.,-1.,0.));
#12822=DIRECTION('ref_axis',(1.,0.,0.));
#12823=DIRECTION('',(1.,0.,0.));
#12824=DIRECTION('',(1.,0.,0.));
#12825=DIRECTION('',(0.,0.,1.));
#12826=DIRECTION('center_axis',(-1.,0.,0.));
#12827=DIRECTION('ref_axis',(0.,-1.,0.));
#12828=DIRECTION('',(0.,-1.,0.));
#12829=DIRECTION('',(0.,-1.,0.));
#12830=DIRECTION('center_axis',(0.,0.,1.));
#12831=DIRECTION('ref_axis',(1.,0.,0.));
#12832=DIRECTION('center_axis',(0.,0.,1.));
#12833=DIRECTION('ref_axis',(1.,0.,0.));
#12834=DIRECTION('axis',(0.,0.,1.));
#12835=DIRECTION('refdir',(1.,0.,0.));
#12836=DIRECTION('center_axis',(0.,0.,1.));
#12837=DIRECTION('ref_axis',(1.,0.,0.));
#12838=DIRECTION('',(0.,0.,-1.));
#12839=DIRECTION('center_axis',(0.,0.,-1.));
#12840=DIRECTION('ref_axis',(1.,0.,0.));
#12841=DIRECTION('center_axis',(0.,0.,1.));
#12842=DIRECTION('ref_axis',(1.,0.,0.));
#12843=DIRECTION('',(0.,0.,-1.));
#12844=DIRECTION('center_axis',(0.,0.,1.));
#12845=DIRECTION('ref_axis',(1.,0.,0.));
#12846=DIRECTION('',(0.,0.,-1.));
#12847=DIRECTION('center_axis',(0.,0.,1.));
#12848=DIRECTION('ref_axis',(1.,0.,0.));
#12849=DIRECTION('',(0.,0.,-1.));
#12850=DIRECTION('center_axis',(0.,0.,1.));
#12851=DIRECTION('ref_axis',(1.,0.,0.));
#12852=DIRECTION('',(0.,0.,-1.));
#12853=DIRECTION('center_axis',(0.,0.,1.));
#12854=DIRECTION('ref_axis',(1.,0.,0.));
#12855=DIRECTION('',(0.,0.,-1.));
#12856=DIRECTION('center_axis',(0.,0.,1.));
#12857=DIRECTION('ref_axis',(1.,0.,0.));
#12858=DIRECTION('',(0.,0.,-1.));
#12859=DIRECTION('center_axis',(0.,0.,1.));
#12860=DIRECTION('ref_axis',(1.,0.,0.));
#12861=DIRECTION('',(0.,0.,-1.));
#12862=DIRECTION('center_axis',(0.,0.,1.));
#12863=DIRECTION('ref_axis',(1.,0.,0.));
#12864=DIRECTION('',(0.,0.,-1.));
#12865=DIRECTION('center_axis',(0.,0.,1.));
#12866=DIRECTION('ref_axis',(1.,0.,0.));
#12867=DIRECTION('',(0.,0.,-1.));
#12868=DIRECTION('center_axis',(0.,0.,1.));
#12869=DIRECTION('ref_axis',(1.,0.,0.));
#12870=DIRECTION('',(0.,0.,-1.));
#12871=DIRECTION('center_axis',(0.,0.,1.));
#12872=DIRECTION('ref_axis',(1.,0.,0.));
#12873=DIRECTION('',(0.,0.,-1.));
#12874=DIRECTION('center_axis',(0.,0.,1.));
#12875=DIRECTION('ref_axis',(1.,0.,0.));
#12876=DIRECTION('',(0.,0.,-1.));
#12877=DIRECTION('center_axis',(0.,0.,1.));
#12878=DIRECTION('ref_axis',(1.,0.,0.));
#12879=DIRECTION('',(0.,0.,-1.));
#12880=DIRECTION('center_axis',(0.,0.,1.));
#12881=DIRECTION('ref_axis',(1.,0.,0.));
#12882=DIRECTION('',(0.,0.,-1.));
#12883=DIRECTION('center_axis',(0.,0.,1.));
#12884=DIRECTION('ref_axis',(1.,0.,0.));
#12885=DIRECTION('',(0.,0.,-1.));
#12886=DIRECTION('center_axis',(0.,0.,1.));
#12887=DIRECTION('ref_axis',(1.,1.29731060939901E-13,0.));
#12888=DIRECTION('',(0.,0.,1.));
#12889=DIRECTION('center_axis',(0.,0.,-1.));
#12890=DIRECTION('ref_axis',(1.,1.29731060939901E-13,0.));
#12891=DIRECTION('center_axis',(0.,0.,1.));
#12892=DIRECTION('ref_axis',(1.,1.29731060939901E-13,0.));
#12893=DIRECTION('',(0.,0.,1.));
#12894=DIRECTION('center_axis',(0.,0.,1.));
#12895=DIRECTION('ref_axis',(1.,1.29731060939901E-13,0.));
#12896=DIRECTION('',(0.,0.,1.));
#12897=DIRECTION('center_axis',(0.,0.,1.));
#12898=DIRECTION('ref_axis',(1.,1.29731060939901E-13,0.));
#12899=DIRECTION('',(0.,0.,1.));
#12900=DIRECTION('center_axis',(0.,0.,1.));
#12901=DIRECTION('ref_axis',(1.,1.29731060939901E-13,0.));
#12902=DIRECTION('',(0.,0.,1.));
#12903=DIRECTION('center_axis',(0.,0.,1.));
#12904=DIRECTION('ref_axis',(1.,1.29731060939901E-13,0.));
#12905=DIRECTION('',(0.,0.,1.));
#12906=DIRECTION('center_axis',(0.,0.,1.));
#12907=DIRECTION('ref_axis',(1.,1.29731060939901E-13,0.));
#12908=DIRECTION('',(0.,0.,1.));
#12909=DIRECTION('center_axis',(0.,0.,1.));
#12910=DIRECTION('ref_axis',(1.,1.29731060939901E-13,0.));
#12911=DIRECTION('',(0.,0.,1.));
#12912=DIRECTION('center_axis',(0.,0.,1.));
#12913=DIRECTION('ref_axis',(1.,1.29731060939901E-13,0.));
#12914=DIRECTION('',(0.,0.,1.));
#12915=DIRECTION('center_axis',(0.,0.,1.));
#12916=DIRECTION('ref_axis',(1.,1.29731060939901E-13,0.));
#12917=DIRECTION('',(0.,0.,1.));
#12918=DIRECTION('center_axis',(0.,0.,1.));
#12919=DIRECTION('ref_axis',(1.,1.29731060939901E-13,0.));
#12920=DIRECTION('',(0.,0.,1.));
#12921=DIRECTION('center_axis',(0.,0.,1.));
#12922=DIRECTION('ref_axis',(1.,1.29731060939901E-13,0.));
#12923=DIRECTION('',(0.,0.,1.));
#12924=DIRECTION('center_axis',(0.,0.,1.));
#12925=DIRECTION('ref_axis',(1.,1.29731060939901E-13,0.));
#12926=DIRECTION('',(0.,0.,1.));
#12927=DIRECTION('center_axis',(0.,0.,1.));
#12928=DIRECTION('ref_axis',(1.,1.29731060939901E-13,0.));
#12929=DIRECTION('',(0.,0.,1.));
#12930=DIRECTION('center_axis',(0.,0.,1.));
#12931=DIRECTION('ref_axis',(1.,1.29731060939901E-13,0.));
#12932=DIRECTION('',(0.,0.,1.));
#12933=DIRECTION('center_axis',(0.,0.,1.));
#12934=DIRECTION('ref_axis',(1.,1.29731060939901E-13,0.));
#12935=DIRECTION('',(0.,0.,1.));
#12936=DIRECTION('center_axis',(0.,0.,-1.));
#12937=DIRECTION('ref_axis',(1.,0.,0.));
#12938=DIRECTION('center_axis',(0.,0.,-1.));
#12939=DIRECTION('ref_axis',(1.,0.,0.));
#12940=DIRECTION('',(0.707106781186548,8.65956056235494E-17,0.707106781186547));
#12941=DIRECTION('center_axis',(0.,0.,1.));
#12942=DIRECTION('ref_axis',(1.,0.,0.));
#12943=DIRECTION('center_axis',(0.,0.,1.));
#12944=DIRECTION('ref_axis',(1.,1.29731060939901E-13,0.));
#12945=DIRECTION('center_axis',(0.,0.,-1.));
#12946=DIRECTION('ref_axis',(1.,1.29731060939901E-13,0.));
#12947=DIRECTION('center_axis',(0.,0.,1.));
#12948=DIRECTION('ref_axis',(1.,0.,0.));
#12949=DIRECTION('center_axis',(-1.60246890531964E-16,-1.,0.));
#12950=DIRECTION('ref_axis',(1.,-1.60246890531964E-16,0.));
#12951=DIRECTION('',(1.,-1.60246890531964E-16,0.));
#12952=DIRECTION('',(0.,0.,1.));
#12953=DIRECTION('',(1.,-1.60246890531964E-16,0.));
#12954=DIRECTION('',(0.,0.,1.));
#12955=DIRECTION('center_axis',(-0.866025403784439,-0.5,0.));
#12956=DIRECTION('ref_axis',(0.5,-0.866025403784439,0.));
#12957=DIRECTION('',(0.5,-0.866025403784439,0.));
#12958=DIRECTION('',(0.,0.,1.));
#12959=DIRECTION('',(0.5,-0.866025403784439,0.));
#12960=DIRECTION('center_axis',(-0.866025403784439,0.5,0.));
#12961=DIRECTION('ref_axis',(-0.5,-0.866025403784439,0.));
#12962=DIRECTION('',(-0.5,-0.866025403784439,0.));
#12963=DIRECTION('',(0.,0.,1.));
#12964=DIRECTION('',(-0.5,-0.866025403784439,0.));
#12965=DIRECTION('center_axis',(1.60246890531964E-16,1.,0.));
#12966=DIRECTION('ref_axis',(-1.,1.60246890531964E-16,0.));
#12967=DIRECTION('',(-1.,1.60246890531964E-16,0.));
#12968=DIRECTION('',(0.,0.,1.));
#12969=DIRECTION('',(-1.,1.60246890531964E-16,0.));
#12970=DIRECTION('center_axis',(0.866025403784439,0.5,0.));
#12971=DIRECTION('ref_axis',(-0.5,0.866025403784439,0.));
#12972=DIRECTION('',(-0.5,0.866025403784439,0.));
#12973=DIRECTION('',(0.,0.,1.));
#12974=DIRECTION('',(-0.5,0.866025403784439,0.));
#12975=DIRECTION('center_axis',(0.866025403784439,-0.5,0.));
#12976=DIRECTION('ref_axis',(0.5,0.866025403784439,0.));
#12977=DIRECTION('',(0.5,0.866025403784439,0.));
#12978=DIRECTION('',(0.5,0.866025403784439,0.));
#12979=DIRECTION('center_axis',(0.,0.,1.));
#12980=DIRECTION('ref_axis',(1.,0.,0.));
#12981=DIRECTION('center_axis',(0.,0.,1.));
#12982=DIRECTION('ref_axis',(1.,0.,0.));
#12983=DIRECTION('center_axis',(0.,0.,1.));
#12984=DIRECTION('ref_axis',(1.,0.,0.));
#12985=DIRECTION('center_axis',(0.,0.,1.));
#12986=DIRECTION('ref_axis',(1.,0.,0.));
#12987=DIRECTION('',(0.,0.,-1.));
#12988=DIRECTION('center_axis',(0.,0.,1.));
#12989=DIRECTION('ref_axis',(1.,0.,0.));
#12990=DIRECTION('center_axis',(0.,0.,1.));
#12991=DIRECTION('ref_axis',(1.,0.,0.));
#12992=DIRECTION('center_axis',(0.,0.,1.));
#12993=DIRECTION('ref_axis',(1.,0.,0.));
#12994=DIRECTION('axis',(0.,0.,1.));
#12995=DIRECTION('refdir',(1.,0.,0.));
#12996=DIRECTION('center_axis',(0.,0.,1.));
#12997=DIRECTION('ref_axis',(1.,0.,0.));
#12998=DIRECTION('',(0.,0.,-1.));
#12999=DIRECTION('center_axis',(0.,0.,-1.));
#13000=DIRECTION('ref_axis',(1.,0.,0.));
#13001=DIRECTION('center_axis',(0.,0.,1.));
#13002=DIRECTION('ref_axis',(1.,0.,0.));
#13003=DIRECTION('',(0.,0.,-1.));
#13004=DIRECTION('center_axis',(0.,0.,1.));
#13005=DIRECTION('ref_axis',(1.,0.,0.));
#13006=DIRECTION('',(0.,0.,-1.));
#13007=DIRECTION('center_axis',(0.,0.,1.));
#13008=DIRECTION('ref_axis',(1.,0.,0.));
#13009=DIRECTION('',(0.,0.,-1.));
#13010=DIRECTION('center_axis',(0.,0.,1.));
#13011=DIRECTION('ref_axis',(1.,0.,0.));
#13012=DIRECTION('',(0.,0.,-1.));
#13013=DIRECTION('center_axis',(0.,0.,1.));
#13014=DIRECTION('ref_axis',(1.,0.,0.));
#13015=DIRECTION('',(0.,0.,-1.));
#13016=DIRECTION('center_axis',(0.,0.,1.));
#13017=DIRECTION('ref_axis',(1.,0.,0.));
#13018=DIRECTION('',(0.,0.,-1.));
#13019=DIRECTION('center_axis',(0.,0.,1.));
#13020=DIRECTION('ref_axis',(1.,0.,0.));
#13021=DIRECTION('',(0.,0.,-1.));
#13022=DIRECTION('center_axis',(0.,0.,1.));
#13023=DIRECTION('ref_axis',(1.,0.,0.));
#13024=DIRECTION('',(0.,0.,-1.));
#13025=DIRECTION('center_axis',(0.,0.,1.));
#13026=DIRECTION('ref_axis',(1.,0.,0.));
#13027=DIRECTION('',(0.,0.,-1.));
#13028=DIRECTION('center_axis',(0.,0.,1.));
#13029=DIRECTION('ref_axis',(1.,0.,0.));
#13030=DIRECTION('',(0.,0.,-1.));
#13031=DIRECTION('center_axis',(0.,0.,1.));
#13032=DIRECTION('ref_axis',(0.997344302588954,-0.0728309144069492,0.));
#13033=DIRECTION('',(0.,0.,1.));
#13034=DIRECTION('center_axis',(0.,0.,-1.));
#13035=DIRECTION('ref_axis',(1.,7.52212518638754E-14,0.));
#13036=DIRECTION('center_axis',(0.,0.,1.));
#13037=DIRECTION('ref_axis',(1.,7.52212518638754E-14,0.));
#13038=DIRECTION('',(0.,0.,1.));
#13039=DIRECTION('center_axis',(0.,0.,1.));
#13040=DIRECTION('ref_axis',(1.,7.52212518638754E-14,0.));
#13041=DIRECTION('',(0.,0.,1.));
#13042=DIRECTION('center_axis',(0.,0.,1.));
#13043=DIRECTION('ref_axis',(1.,7.52212518638754E-14,0.));
#13044=DIRECTION('',(0.,0.,1.));
#13045=DIRECTION('center_axis',(0.,0.,1.));
#13046=DIRECTION('ref_axis',(1.,7.52212518638754E-14,0.));
#13047=DIRECTION('',(0.,0.,1.));
#13048=DIRECTION('center_axis',(0.,0.,1.));
#13049=DIRECTION('ref_axis',(1.,7.52212518638754E-14,0.));
#13050=DIRECTION('',(0.,0.,1.));
#13051=DIRECTION('center_axis',(0.,0.,1.));
#13052=DIRECTION('ref_axis',(1.,7.52212518638754E-14,0.));
#13053=DIRECTION('',(0.,0.,1.));
#13054=DIRECTION('center_axis',(0.,0.,1.));
#13055=DIRECTION('ref_axis',(1.,7.52212518638754E-14,0.));
#13056=DIRECTION('',(0.,0.,1.));
#13057=DIRECTION('center_axis',(0.,0.,1.));
#13058=DIRECTION('ref_axis',(1.,7.52212518638754E-14,0.));
#13059=DIRECTION('',(0.,0.,1.));
#13060=DIRECTION('center_axis',(0.,0.,1.));
#13061=DIRECTION('ref_axis',(1.,7.52212518638754E-14,0.));
#13062=DIRECTION('',(0.,0.,1.));
#13063=DIRECTION('center_axis',(0.,0.,1.));
#13064=DIRECTION('ref_axis',(1.,7.52212518638754E-14,0.));
#13065=DIRECTION('',(0.,0.,1.));
#13066=DIRECTION('center_axis',(0.,0.,-1.));
#13067=DIRECTION('ref_axis',(1.,0.,0.));
#13068=DIRECTION('center_axis',(0.,0.,-1.));
#13069=DIRECTION('ref_axis',(1.,0.,0.));
#13070=DIRECTION('',(0.707106781186548,8.65956056235494E-17,0.707106781186547));
#13071=DIRECTION('center_axis',(0.,0.,1.));
#13072=DIRECTION('ref_axis',(1.,0.,0.));
#13073=DIRECTION('center_axis',(0.,0.,1.));
#13074=DIRECTION('ref_axis',(1.,7.52212518638754E-14,0.));
#13075=DIRECTION('center_axis',(0.,0.,-1.));
#13076=DIRECTION('ref_axis',(1.,7.52212518638754E-14,0.));
#13077=DIRECTION('center_axis',(0.,0.,1.));
#13078=DIRECTION('ref_axis',(1.,0.,0.));
#13079=DIRECTION('center_axis',(-1.92296268638356E-16,-1.,0.));
#13080=DIRECTION('ref_axis',(1.,-1.92296268638356E-16,0.));
#13081=DIRECTION('',(1.,-1.92296268638356E-16,0.));
#13082=DIRECTION('',(0.,0.,1.));
#13083=DIRECTION('',(1.,-1.92296268638356E-16,0.));
#13084=DIRECTION('',(0.,0.,1.));
#13085=DIRECTION('center_axis',(-0.866025403784439,-0.5,0.));
#13086=DIRECTION('ref_axis',(0.5,-0.866025403784439,0.));
#13087=DIRECTION('',(0.5,-0.866025403784439,0.));
#13088=DIRECTION('',(0.,0.,1.));
#13089=DIRECTION('',(0.5,-0.866025403784439,0.));
#13090=DIRECTION('center_axis',(-0.866025403784439,0.5,0.));
#13091=DIRECTION('ref_axis',(-0.5,-0.866025403784438,0.));
#13092=DIRECTION('',(-0.5,-0.866025403784438,0.));
#13093=DIRECTION('',(0.,0.,1.));
#13094=DIRECTION('',(-0.5,-0.866025403784439,0.));
#13095=DIRECTION('center_axis',(1.92296268638356E-16,1.,0.));
#13096=DIRECTION('ref_axis',(-1.,1.92296268638356E-16,0.));
#13097=DIRECTION('',(-1.,1.92296268638356E-16,0.));
#13098=DIRECTION('',(0.,0.,1.));
#13099=DIRECTION('',(-1.,1.92296268638356E-16,0.));
#13100=DIRECTION('center_axis',(0.866025403784439,0.5,0.));
#13101=DIRECTION('ref_axis',(-0.5,0.866025403784439,0.));
#13102=DIRECTION('',(-0.5,0.866025403784439,0.));
#13103=DIRECTION('',(0.,0.,1.));
#13104=DIRECTION('',(-0.5,0.866025403784439,0.));
#13105=DIRECTION('center_axis',(0.866025403784439,-0.5,0.));
#13106=DIRECTION('ref_axis',(0.5,0.866025403784439,0.));
#13107=DIRECTION('',(0.5,0.866025403784439,0.));
#13108=DIRECTION('',(0.5,0.866025403784439,0.));
#13109=DIRECTION('center_axis',(0.,0.,1.));
#13110=DIRECTION('ref_axis',(1.,0.,0.));
#13111=DIRECTION('center_axis',(0.,0.,1.));
#13112=DIRECTION('ref_axis',(1.,0.,0.));
#13113=DIRECTION('center_axis',(0.,0.,1.));
#13114=DIRECTION('ref_axis',(1.,0.,0.));
#13115=DIRECTION('center_axis',(0.,0.,1.));
#13116=DIRECTION('ref_axis',(1.,0.,0.));
#13117=DIRECTION('',(0.,0.,-1.));
#13118=DIRECTION('center_axis',(0.,0.,1.));
#13119=DIRECTION('ref_axis',(1.,0.,0.));
#13120=DIRECTION('center_axis',(0.,0.,1.));
#13121=DIRECTION('ref_axis',(1.,0.,0.));
#13122=DIRECTION('center_axis',(0.,0.,1.));
#13123=DIRECTION('ref_axis',(1.,0.,0.));
#13124=DIRECTION('axis',(0.,0.,1.));
#13125=DIRECTION('refdir',(1.,0.,0.));
#13126=DIRECTION('center_axis',(0.,0.,1.));
#13127=DIRECTION('ref_axis',(1.,0.,0.));
#13128=DIRECTION('',(0.,0.,-1.));
#13129=DIRECTION('center_axis',(0.,0.,-1.));
#13130=DIRECTION('ref_axis',(1.,0.,0.));
#13131=DIRECTION('center_axis',(0.,0.,1.));
#13132=DIRECTION('ref_axis',(1.,0.,0.));
#13133=DIRECTION('',(0.,0.,-1.));
#13134=DIRECTION('center_axis',(0.,0.,1.));
#13135=DIRECTION('ref_axis',(1.,0.,0.));
#13136=DIRECTION('',(0.,0.,-1.));
#13137=DIRECTION('center_axis',(0.,0.,1.));
#13138=DIRECTION('ref_axis',(1.,0.,0.));
#13139=DIRECTION('',(0.,0.,-1.));
#13140=DIRECTION('center_axis',(0.,0.,1.));
#13141=DIRECTION('ref_axis',(1.,0.,0.));
#13142=DIRECTION('',(0.,0.,-1.));
#13143=DIRECTION('center_axis',(0.,0.,1.));
#13144=DIRECTION('ref_axis',(1.,0.,0.));
#13145=DIRECTION('',(0.,0.,-1.));
#13146=DIRECTION('center_axis',(0.,0.,1.));
#13147=DIRECTION('ref_axis',(1.,0.,0.));
#13148=DIRECTION('',(0.,0.,-1.));
#13149=DIRECTION('center_axis',(0.,0.,1.));
#13150=DIRECTION('ref_axis',(1.,0.,0.));
#13151=DIRECTION('',(0.,0.,-1.));
#13152=DIRECTION('center_axis',(0.,0.,1.));
#13153=DIRECTION('ref_axis',(1.,0.,0.));
#13154=DIRECTION('',(0.,0.,-1.));
#13155=DIRECTION('center_axis',(0.,0.,1.));
#13156=DIRECTION('ref_axis',(1.,0.,0.));
#13157=DIRECTION('',(0.,0.,-1.));
#13158=DIRECTION('center_axis',(0.,0.,1.));
#13159=DIRECTION('ref_axis',(0.540789512512072,-0.84115795375004,0.));
#13160=DIRECTION('',(0.,0.,1.));
#13161=DIRECTION('center_axis',(0.,0.,1.));
#13162=DIRECTION('ref_axis',(1.,5.20562201223838E-14,0.));
#13163=DIRECTION('center_axis',(0.,0.,1.));
#13164=DIRECTION('ref_axis',(1.,5.20562201223838E-14,0.));
#13165=DIRECTION('',(0.,0.,1.));
#13166=DIRECTION('center_axis',(0.,0.,1.));
#13167=DIRECTION('ref_axis',(1.,5.20562201223838E-14,0.));
#13168=DIRECTION('',(0.,0.,1.));
#13169=DIRECTION('center_axis',(0.,0.,1.));
#13170=DIRECTION('ref_axis',(1.,5.20562201223838E-14,0.));
#13171=DIRECTION('',(0.,0.,1.));
#13172=DIRECTION('center_axis',(0.,0.,1.));
#13173=DIRECTION('ref_axis',(1.,5.20562201223838E-14,0.));
#13174=DIRECTION('',(0.,0.,1.));
#13175=DIRECTION('center_axis',(0.,0.,1.));
#13176=DIRECTION('ref_axis',(1.,5.20562201223838E-14,0.));
#13177=DIRECTION('',(0.,0.,1.));
#13178=DIRECTION('center_axis',(0.,0.,1.));
#13179=DIRECTION('ref_axis',(1.,5.20562201223838E-14,0.));
#13180=DIRECTION('',(0.,0.,1.));
#13181=DIRECTION('center_axis',(0.,0.,1.));
#13182=DIRECTION('ref_axis',(1.,5.20562201223838E-14,0.));
#13183=DIRECTION('',(0.,0.,1.));
#13184=DIRECTION('center_axis',(0.,0.,1.));
#13185=DIRECTION('ref_axis',(1.,5.20562201223838E-14,0.));
#13186=DIRECTION('',(0.,0.,1.));
#13187=DIRECTION('center_axis',(0.,0.,1.));
#13188=DIRECTION('ref_axis',(0.888917950975616,0.4580664541672,0.));
#13189=DIRECTION('center_axis',(0.,0.,-1.));
#13190=DIRECTION('ref_axis',(1.,5.20562201223838E-14,0.));
#13191=DIRECTION('center_axis',(0.,0.,1.));
#13192=DIRECTION('ref_axis',(1.,0.,0.));
#13193=DIRECTION('center_axis',(0.,0.,-1.));
#13194=DIRECTION('ref_axis',(1.,0.,0.));
#13195=DIRECTION('center_axis',(0.,0.,1.));
#13196=DIRECTION('ref_axis',(1.,0.,0.));
#13197=DIRECTION('center_axis',(0.,0.,1.));
#13198=DIRECTION('ref_axis',(1.,0.,0.));
#13199=DIRECTION('center_axis',(0.,0.,1.));
#13200=DIRECTION('ref_axis',(1.,0.,0.));
#13201=DIRECTION('center_axis',(0.,0.,1.));
#13202=DIRECTION('ref_axis',(1.,0.,0.));
#13203=DIRECTION('center_axis',(0.,0.,1.));
#13204=DIRECTION('ref_axis',(1.,0.,0.));
#13205=DIRECTION('center_axis',(0.,0.,-1.));
#13206=DIRECTION('ref_axis',(1.,0.,0.));
#13207=DIRECTION('center_axis',(0.,0.,1.));
#13208=DIRECTION('ref_axis',(1.,0.,0.));
#13209=DIRECTION('',(0.,0.,-1.));
#13210=DIRECTION('center_axis',(0.,0.,1.));
#13211=DIRECTION('ref_axis',(1.,0.,0.));
#13212=DIRECTION('',(0.,0.,-1.));
#13213=DIRECTION('center_axis',(0.,0.,1.));
#13214=DIRECTION('ref_axis',(1.,0.,0.));
#13215=DIRECTION('center_axis',(0.,0.,1.));
#13216=DIRECTION('ref_axis',(1.,0.,0.));
#13217=DIRECTION('center_axis',(0.,0.,1.));
#13218=DIRECTION('ref_axis',(1.,0.,0.));
#13219=DIRECTION('center_axis',(0.,0.,1.));
#13220=DIRECTION('ref_axis',(1.,0.,0.));
#13221=DIRECTION('center_axis',(0.,0.,1.));
#13222=DIRECTION('ref_axis',(1.,0.,0.));
#13223=DIRECTION('center_axis',(0.,0.,-1.));
#13224=DIRECTION('ref_axis',(1.,0.,0.));
#13225=DIRECTION('center_axis',(0.,0.,1.));
#13226=DIRECTION('ref_axis',(1.,0.,0.));
#13227=DIRECTION('',(0.,0.,-1.));
#13228=DIRECTION('center_axis',(0.,0.,1.));
#13229=DIRECTION('ref_axis',(1.,0.,0.));
#13230=DIRECTION('',(0.,0.,-1.));
#13231=DIRECTION('center_axis',(0.,0.,1.));
#13232=DIRECTION('ref_axis',(1.,0.,0.));
#13233=DIRECTION('center_axis',(0.,0.,1.));
#13234=DIRECTION('ref_axis',(1.,0.,0.));
#13235=DIRECTION('center_axis',(0.,0.,1.));
#13236=DIRECTION('ref_axis',(1.,0.,0.));
#13237=DIRECTION('center_axis',(0.,0.,1.));
#13238=DIRECTION('ref_axis',(1.,0.,0.));
#13239=DIRECTION('center_axis',(0.,0.,1.));
#13240=DIRECTION('ref_axis',(1.,0.,0.));
#13241=DIRECTION('center_axis',(0.,0.,-1.));
#13242=DIRECTION('ref_axis',(1.,0.,0.));
#13243=DIRECTION('center_axis',(0.,0.,1.));
#13244=DIRECTION('ref_axis',(1.,0.,0.));
#13245=DIRECTION('',(0.,0.,-1.));
#13246=DIRECTION('center_axis',(0.,0.,1.));
#13247=DIRECTION('ref_axis',(1.,0.,0.));
#13248=DIRECTION('',(0.,0.,-1.));
#13249=DIRECTION('center_axis',(0.,0.,1.));
#13250=DIRECTION('ref_axis',(1.,0.,0.));
#13251=DIRECTION('center_axis',(0.,0.,1.));
#13252=DIRECTION('ref_axis',(1.,0.,0.));
#13253=DIRECTION('center_axis',(0.,0.,1.));
#13254=DIRECTION('ref_axis',(1.,0.,0.));
#13255=DIRECTION('',(0.,0.,-1.));
#13256=DIRECTION('center_axis',(0.,0.,1.));
#13257=DIRECTION('ref_axis',(1.,0.,0.));
#13258=DIRECTION('center_axis',(0.,0.,-1.));
#13259=DIRECTION('ref_axis',(1.,0.,0.));
#13260=DIRECTION('center_axis',(0.,0.,1.));
#13261=DIRECTION('ref_axis',(1.,0.,0.));
#13262=DIRECTION('center_axis',(0.,0.,1.));
#13263=DIRECTION('ref_axis',(1.,0.,0.));
#13264=DIRECTION('center_axis',(0.,0.,1.));
#13265=DIRECTION('ref_axis',(1.,0.,0.));
#13266=DIRECTION('',(0.,0.,-1.));
#13267=DIRECTION('center_axis',(0.,0.,1.));
#13268=DIRECTION('ref_axis',(1.,0.,0.));
#13269=DIRECTION('center_axis',(0.,0.,1.));
#13270=DIRECTION('ref_axis',(1.,0.,0.));
#13271=DIRECTION('center_axis',(0.,0.,1.));
#13272=DIRECTION('ref_axis',(1.,0.,0.));
#13273=DIRECTION('center_axis',(0.,0.,-1.));
#13274=DIRECTION('ref_axis',(1.,0.,0.));
#13275=DIRECTION('',(0.,0.,-1.));
#13276=DIRECTION('center_axis',(0.,0.,1.));
#13277=DIRECTION('ref_axis',(1.,0.,0.));
#13278=DIRECTION('axis',(0.,0.,1.));
#13279=DIRECTION('refdir',(1.,0.,0.));
#13280=DIRECTION('center_axis',(0.,0.,1.));
#13281=DIRECTION('ref_axis',(1.,0.,0.));
#13282=DIRECTION('center_axis',(0.,0.,-1.));
#13283=DIRECTION('ref_axis',(1.,0.,0.));
#13284=DIRECTION('',(0.,0.,-1.));
#13285=DIRECTION('center_axis',(0.,0.,-1.));
#13286=DIRECTION('ref_axis',(1.,0.,0.));
#13287=DIRECTION('center_axis',(0.,0.,1.));
#13288=DIRECTION('ref_axis',(1.,0.,0.));
#13289=DIRECTION('center_axis',(0.,0.,1.));
#13290=DIRECTION('ref_axis',(1.,0.,0.));
#13291=DIRECTION('',(0.,0.,-1.));
#13292=DIRECTION('center_axis',(0.,0.,1.));
#13293=DIRECTION('ref_axis',(1.,0.,0.));
#13294=DIRECTION('center_axis',(0.,0.,1.));
#13295=DIRECTION('ref_axis',(1.,0.,0.));
#13296=DIRECTION('center_axis',(0.,0.,1.));
#13297=DIRECTION('ref_axis',(1.,0.,0.));
#13298=DIRECTION('',(0.,0.,1.));
#13299=DIRECTION('',(1.,0.,0.));
#13300=DIRECTION('',(0.,0.,1.));
#13301=DIRECTION('',(1.,0.,0.));
#13302=DIRECTION('',(0.,0.,1.));
#13303=DIRECTION('',(1.,0.,0.));
#13304=DIRECTION('',(1.,0.,0.));
#13305=DIRECTION('',(0.,1.,0.));
#13306=DIRECTION('',(1.,0.,0.));
#13307=DIRECTION('',(0.,1.,0.));
#13308=DIRECTION('',(0.,0.,1.));
#13309=DIRECTION('',(1.,0.,0.));
#13310=DIRECTION('',(0.,-1.22464679914735E-16,-1.));
#13311=DIRECTION('',(0.342020143325669,0.939692620785908,-1.15079156022785E-16));
#13312=DIRECTION('',(0.,0.,1.));
#13313=DIRECTION('',(-0.984807753012208,0.17364817766693,0.));
#13314=DIRECTION('',(0.,0.,1.));
#13315=DIRECTION('',(-0.64278760968654,-0.766044443118978,0.));
#13316=DIRECTION('',(0.,0.,1.));
#13317=DIRECTION('',(1.,0.,0.));
#13318=DIRECTION('',(0.,0.,1.));
#13319=DIRECTION('',(-1.,1.22464679914735E-16,0.));
#13320=DIRECTION('',(0.,0.,1.));
#13321=DIRECTION('',(-1.,1.22464679914735E-16,0.));
#13322=DIRECTION('',(0.,0.,1.));
#13323=DIRECTION('',(-1.,1.22464679914735E-16,0.));
#13324=DIRECTION('',(1.,0.,0.));
#13325=DIRECTION('',(0.,1.,0.));
#13326=DIRECTION('',(1.,0.,0.));
#13327=DIRECTION('',(0.,1.,0.));
#13328=DIRECTION('',(1.,0.,0.));
#13329=DIRECTION('',(0.,1.,0.));
#13330=DIRECTION('',(1.,0.,0.));
#13331=DIRECTION('',(0.,1.,0.));
#13332=DIRECTION('',(1.,0.,0.));
#13333=DIRECTION('',(0.,1.,0.));
#13334=DIRECTION('',(1.,0.,0.));
#13335=DIRECTION('',(0.,1.,0.));
#13336=DIRECTION('',(1.,0.,0.));
#13337=DIRECTION('',(0.,1.,0.));
#13338=DIRECTION('',(1.,0.,0.));
#13339=DIRECTION('',(0.,1.,0.));
#13340=DIRECTION('',(1.,0.,0.));
#13341=DIRECTION('',(0.,1.,0.));
#13342=DIRECTION('',(1.,0.,0.));
#13343=DIRECTION('',(0.,1.,0.));
#13344=DIRECTION('',(1.,0.,0.));
#13345=DIRECTION('',(0.,1.,0.));
#13346=DIRECTION('',(1.,0.,0.));
#13347=DIRECTION('',(0.,1.,0.));
#13348=DIRECTION('',(1.,0.,0.));
#13349=DIRECTION('',(0.,1.,0.));
#13350=DIRECTION('',(1.,0.,0.));
#13351=DIRECTION('',(0.,1.,0.));
#13352=DIRECTION('',(1.,0.,0.));
#13353=DIRECTION('',(0.,1.,0.));
#13354=DIRECTION('',(1.,0.,0.));
#13355=DIRECTION('',(0.,1.,0.));
#13356=DIRECTION('',(1.,0.,0.));
#13357=DIRECTION('',(0.,1.,0.));
#13358=DIRECTION('',(1.,0.,0.));
#13359=DIRECTION('',(0.,1.,0.));
#13360=DIRECTION('',(1.,0.,0.));
#13361=DIRECTION('',(0.,1.,0.));
#13362=DIRECTION('',(1.,0.,0.));
#13363=DIRECTION('',(0.,1.,0.));
#13364=DIRECTION('',(1.,0.,0.));
#13365=DIRECTION('',(0.,1.,0.));
#13366=DIRECTION('',(1.,0.,0.));
#13367=DIRECTION('',(0.,1.,0.));
#13368=DIRECTION('',(1.,0.,0.));
#13369=DIRECTION('',(0.,1.,0.));
#13370=DIRECTION('',(1.,0.,0.));
#13371=DIRECTION('',(0.,1.,0.));
#13372=DIRECTION('',(1.,0.,0.));
#13373=DIRECTION('',(0.,1.,0.));
#13374=DIRECTION('',(1.,0.,0.));
#13375=DIRECTION('',(0.,1.,0.));
#13376=DIRECTION('',(1.,0.,0.));
#13377=DIRECTION('',(0.,1.,0.));
#13378=DIRECTION('',(1.,0.,0.));
#13379=DIRECTION('',(0.,1.,0.));
#13380=DIRECTION('',(1.,0.,0.));
#13381=DIRECTION('',(0.,1.,0.));
#13382=DIRECTION('',(1.,0.,0.));
#13383=DIRECTION('',(0.,1.,0.));
#13384=DIRECTION('',(1.,0.,0.));
#13385=DIRECTION('',(0.,1.,0.));
#13386=DIRECTION('',(1.,0.,0.));
#13387=DIRECTION('',(0.,1.,0.));
#13388=DIRECTION('',(1.,0.,0.));
#13389=DIRECTION('',(0.,1.,0.));
#13390=DIRECTION('',(1.,0.,0.));
#13391=DIRECTION('',(0.,1.,0.));
#13392=DIRECTION('',(1.,0.,0.));
#13393=DIRECTION('',(0.,1.,0.));
#13394=DIRECTION('',(1.,0.,0.));
#13395=DIRECTION('',(0.,1.,0.));
#13396=DIRECTION('',(1.,0.,0.));
#13397=DIRECTION('',(0.,1.,0.));
#13398=DIRECTION('',(1.,0.,0.));
#13399=DIRECTION('',(0.,1.,0.));
#13400=DIRECTION('',(1.,0.,0.));
#13401=DIRECTION('',(0.,1.,0.));
#13402=DIRECTION('',(1.,0.,0.));
#13403=DIRECTION('',(0.,1.,0.));
#13404=DIRECTION('',(1.,0.,0.));
#13405=DIRECTION('',(0.,1.,0.));
#13406=DIRECTION('',(1.,0.,0.));
#13407=DIRECTION('',(0.,1.,0.));
#13408=DIRECTION('',(1.,0.,0.));
#13409=DIRECTION('',(0.,1.,0.));
#13410=DIRECTION('',(1.,0.,0.));
#13411=DIRECTION('',(0.,1.,0.));
#13412=DIRECTION('',(1.,0.,0.));
#13413=DIRECTION('',(0.,1.,0.));
#13414=DIRECTION('',(0.,0.,1.));
#13415=DIRECTION('',(-1.,1.22464679914735E-16,0.));
#13416=DIRECTION('',(0.,-1.22464679914735E-16,-1.));
#13417=DIRECTION('',(0.342020143325669,0.939692620785908,-1.15079156022785E-16));
#13418=DIRECTION('',(0.,-1.22464679914735E-16,-1.));
#13419=DIRECTION('',(0.342020143325669,0.939692620785908,-1.15079156022785E-16));
#13420=DIRECTION('',(0.,-1.22464679914735E-16,-1.));
#13421=DIRECTION('',(0.342020143325669,0.939692620785908,-1.15079156022785E-16));
#13422=DIRECTION('',(0.,1.22464679914735E-16,-1.));
#13423=DIRECTION('',(-0.342020143325669,-0.939692620785908,-1.15079156022785E-16));
#13424=DIRECTION('',(0.,1.22464679914735E-16,-1.));
#13425=DIRECTION('',(-0.342020143325669,-0.939692620785908,-1.15079156022785E-16));
#13426=DIRECTION('',(0.,1.22464679914735E-16,-1.));
#13427=DIRECTION('',(-0.342020143325669,-0.939692620785908,-1.15079156022785E-16));
#13428=DIRECTION('',(0.,1.22464679914735E-16,-1.));
#13429=DIRECTION('',(-0.342020143325669,-0.939692620785908,-1.15079156022785E-16));
#13430=DIRECTION('',(0.,0.,1.));
#13431=DIRECTION('',(-0.984807753012208,0.17364817766693,0.));
#13432=DIRECTION('',(0.,0.,1.));
#13433=DIRECTION('',(-0.984807753012208,0.17364817766693,0.));
#13434=DIRECTION('',(0.,0.,1.));
#13435=DIRECTION('',(-0.984807753012208,0.17364817766693,0.));
#13436=DIRECTION('',(0.,0.,1.));
#13437=DIRECTION('',(0.984807753012208,-0.17364817766693,0.));
#13438=DIRECTION('',(0.,0.,1.));
#13439=DIRECTION('',(0.984807753012208,-0.17364817766693,0.));
#13440=DIRECTION('',(0.,0.,1.));
#13441=DIRECTION('',(0.984807753012208,-0.17364817766693,0.));
#13442=DIRECTION('',(0.,0.,1.));
#13443=DIRECTION('',(0.984807753012208,-0.17364817766693,0.));
#13444=DIRECTION('',(0.,0.,1.));
#13445=DIRECTION('',(0.64278760968654,0.766044443118978,0.));
#13446=DIRECTION('',(0.,0.,1.));
#13447=DIRECTION('',(-1.,1.22464679914735E-16,0.));
#13448=CARTESIAN_POINT('',(0.,0.,0.));
#13449=CARTESIAN_POINT('',(0.,0.,0.));
#13450=CARTESIAN_POINT('Origin',(-20.,-66.,30.));
#13451=CARTESIAN_POINT('',(-21.6686463164215,-66.0003916927953,25.7714803633902));
#13452=CARTESIAN_POINT('',(-21.6665334720122,-65.9985218171631,25.5785196366098));
#13453=CARTESIAN_POINT('',(-21.666,-66.,30.));
#13454=CARTESIAN_POINT('',(-20.7699020406705,-67.4774325188554,25.));
#13455=CARTESIAN_POINT('Ctrl Pts',(-21.6665334720122,-65.9985218171631,
25.5785196366098));
#13456=CARTESIAN_POINT('Ctrl Pts',(-21.6675831226457,-65.8847144663257,
25.5709016210591));
#13457=CARTESIAN_POINT('Ctrl Pts',(-21.6569164284924,-65.7711020348436,
25.5632836055085));
#13458=CARTESIAN_POINT('Ctrl Pts',(-21.6338086330613,-65.6600764397889,
25.5556655899578));
#13459=CARTESIAN_POINT('Ctrl Pts',(-21.5214416026058,-65.1201886578488,
25.5186212172939));
#13460=CARTESIAN_POINT('Ctrl Pts',(-21.1148901954472,-64.6414696458604,
25.4815768446301));
#13461=CARTESIAN_POINT('Ctrl Pts',(-20.6004654912914,-64.4430320689214,
25.4445324719662));
#13462=CARTESIAN_POINT('Ctrl Pts',(-20.0860407871355,-64.2445944919823,
25.4074880993024));
#13463=CARTESIAN_POINT('Ctrl Pts',(-19.4637427859824,-64.3264383500926,
25.3704437266385));
#13464=CARTESIAN_POINT('Ctrl Pts',(-19.0178170303308,-64.6510266230413,
25.3333993539747));
#13465=CARTESIAN_POINT('Ctrl Pts',(-18.5718912746792,-64.9756148959899,
25.2963549813108));
#13466=CARTESIAN_POINT('Ctrl Pts',(-18.3023377645291,-65.5429475837768,
25.259310608647));
#13467=CARTESIAN_POINT('Ctrl Pts',(-18.3335864161634,-66.0935813146395,
25.2222662359831));
#13468=CARTESIAN_POINT('Ctrl Pts',(-18.3648350677978,-66.6442150455023,
25.1852218633193));
#13469=CARTESIAN_POINT('Ctrl Pts',(-18.6968858812165,-67.1781498194408,
25.1481774906554));
#13470=CARTESIAN_POINT('Ctrl Pts',(-19.1753375331628,-67.4504541256366,
25.1111331179916));
#13471=CARTESIAN_POINT('Ctrl Pts',(-19.653789185109,-67.7227584318323,25.0740887453277));
#13472=CARTESIAN_POINT('Ctrl Pts',(-20.2786416755828,-67.7334322702853,
25.0370443726639));
#13473=CARTESIAN_POINT('Ctrl Pts',(-20.7699020406704,-67.4774325188554,
25.));
#13474=CARTESIAN_POINT('',(-21.3370260554501,-65.0009970088504,25.));
#13475=CARTESIAN_POINT('Origin',(-20.,-66.,25.));
#13476=CARTESIAN_POINT('',(-21.6645215840113,-66.0012211302689,25.0714803633902));
#13477=CARTESIAN_POINT('Ctrl Pts',(-21.3370274731509,-65.0009958365549,
25.));
#13478=CARTESIAN_POINT('Ctrl Pts',(-21.5489927408181,-65.2854500014782,
25.0238267877967));
#13479=CARTESIAN_POINT('Ctrl Pts',(-21.6621689009854,-65.6440627477619,
25.0476535755935));
#13480=CARTESIAN_POINT('Ctrl Pts',(-21.6645215840113,-66.0012211302689,
25.0714803633902));
#13481=CARTESIAN_POINT('',(-21.666,-66.,24.));
#13482=CARTESIAN_POINT('',(-21.666,-66.,30.));
#13483=CARTESIAN_POINT('Origin',(-20.,-66.,24.));
#13484=CARTESIAN_POINT('Ctrl Pts',(-21.6645215840113,-66.0012211302689,
25.0714803633902));
#13485=CARTESIAN_POINT('Ctrl Pts',(-21.6657549943118,-66.188463875268,25.0839717212025));
#13486=CARTESIAN_POINT('Ctrl Pts',(-21.6365290935638,-66.3753068952287,
25.0964630790149));
#13487=CARTESIAN_POINT('Ctrl Pts',(-21.5751098549791,-66.5508551556528,
25.1089544368272));
#13488=CARTESIAN_POINT('Ctrl Pts',(-21.3929649515153,-67.0714611039685,
25.1459988094911));
#13489=CARTESIAN_POINT('Ctrl Pts',(-20.9276865865547,-67.492732078676,25.1830431821549));
#13490=CARTESIAN_POINT('Ctrl Pts',(-20.3917115249228,-67.6221189802502,
25.2200875548188));
#13491=CARTESIAN_POINT('Ctrl Pts',(-19.8557364632908,-67.7515058818244,
25.2571319274826));
#13492=CARTESIAN_POINT('Ctrl Pts',(-19.2490647049875,-67.5890087102653,
25.2941763001465));
#13493=CARTESIAN_POINT('Ctrl Pts',(-18.8495628612421,-67.2088726273032,
25.3312206728103));
#13494=CARTESIAN_POINT('Ctrl Pts',(-18.4500610174968,-66.8287365443411,
25.3682650454742));
#13495=CARTESIAN_POINT('Ctrl Pts',(-18.2577290883093,-66.230961549976,25.405309418138));
#13496=CARTESIAN_POINT('Ctrl Pts',(-18.3604608102357,-65.6891597965066,
25.4423537908019));
#13497=CARTESIAN_POINT('Ctrl Pts',(-18.4631925321622,-65.1473580430372,
25.4793981634657));
#13498=CARTESIAN_POINT('Ctrl Pts',(-18.8609879052027,-64.6615295304635,
25.5164425361296));
#13499=CARTESIAN_POINT('Ctrl Pts',(-19.3718686901783,-64.453969580922,25.5534869087934));
#13500=CARTESIAN_POINT('Ctrl Pts',(-19.8827494751539,-64.2464096313805,
25.5905312814573));
#13501=CARTESIAN_POINT('Ctrl Pts',(-20.5067156720646,-64.3171182448712,
25.6275756541212));
#13502=CARTESIAN_POINT('Ctrl Pts',(-20.9581975997172,-64.6337524970504,
25.664620026785));
#13503=CARTESIAN_POINT('Ctrl Pts',(-21.3923212132001,-64.9382129799389,
25.7002401389867));
#13504=CARTESIAN_POINT('Ctrl Pts',(-21.6669687399304,-65.4700522183443,
25.7358602511885));
#13505=CARTESIAN_POINT('Ctrl Pts',(-21.6686463164215,-66.0003916927953,
25.7714803633902));
#13506=CARTESIAN_POINT('Origin',(-20.,-66.,30.));
#13507=CARTESIAN_POINT('',(-21.6655732814929,-65.9984874577248,26.4714803633902));
#13508=CARTESIAN_POINT('',(-21.6632974926259,-66.0000402088307,26.2785196366098));
#13509=CARTESIAN_POINT('',(-21.666,-66.,30.));
#13510=CARTESIAN_POINT('Ctrl Pts',(-21.6632974926259,-66.0000402088307,
26.2785196366098));
#13511=CARTESIAN_POINT('Ctrl Pts',(-21.6632374792194,-65.7195428093862,
26.2598345237089));
#13512=CARTESIAN_POINT('Ctrl Pts',(-21.5960668066056,-65.4390182789714,
26.241149410808));
#13513=CARTESIAN_POINT('Ctrl Pts',(-21.4619469193729,-65.1953423902613,
26.2224642979072));
#13514=CARTESIAN_POINT('Ctrl Pts',(-21.1960460864137,-64.7122401217089,
26.1854199252433));
#13515=CARTESIAN_POINT('Ctrl Pts',(-20.6669981929564,-64.3739731854776,
26.1483755525794));
#13516=CARTESIAN_POINT('Ctrl Pts',(-20.1169101847181,-64.3353398464244,
26.1113311799156));
#13517=CARTESIAN_POINT('Ctrl Pts',(-19.5668221764797,-64.2967065073713,
26.0742868072517));
#13518=CARTESIAN_POINT('Ctrl Pts',(-18.9956940534603,-64.5577067654963,
26.0372424345879));
#13519=CARTESIAN_POINT('Ctrl Pts',(-18.6648768742022,-64.9989004546789,
26.000198061924));
#13520=CARTESIAN_POINT('Ctrl Pts',(-18.3340596949442,-65.4400941438616,
25.9631536892602));
#13521=CARTESIAN_POINT('Ctrl Pts',(-18.2435534594475,-66.0614812641019,
25.9261093165963));
#13522=CARTESIAN_POINT('Ctrl Pts',(-18.4347923709177,-66.5787054554592,
25.8890649439325));
#13523=CARTESIAN_POINT('Ctrl Pts',(-18.6260312823879,-67.0959296468164,
25.8520205712686));
#13524=CARTESIAN_POINT('Ctrl Pts',(-19.099015340825,-67.5089909092908,25.8149761986048));
#13525=CARTESIAN_POINT('Ctrl Pts',(-19.6372642986701,-67.6288590661524,
25.7779318259409));
#13526=CARTESIAN_POINT('Ctrl Pts',(-20.1755132565153,-67.7487272230141,
25.7408874532771));
#13527=CARTESIAN_POINT('Ctrl Pts',(-20.7790271137684,-67.5754022742632,
25.7038430806132));
#13528=CARTESIAN_POINT('Ctrl Pts',(-21.1716927155188,-67.1882115239419,
25.6667987079494));
#13529=CARTESIAN_POINT('Ctrl Pts',(-21.4836083289379,-66.880644882356,25.6373723508362));
#13530=CARTESIAN_POINT('Ctrl Pts',(-21.6624789522782,-66.4381291828313,
25.607945993723));
#13531=CARTESIAN_POINT('Ctrl Pts',(-21.6665334720122,-65.9985218171631,
25.5785196366098));
#13532=CARTESIAN_POINT('Ctrl Pts',(-21.6686463164215,-66.0003916927953,
25.7714803633902));
#13533=CARTESIAN_POINT('Ctrl Pts',(-21.6687133938595,-66.0215971718989,
25.7729046238523));
#13534=CARTESIAN_POINT('Ctrl Pts',(-21.6683440528391,-66.0428002532123,
25.7743288843144));
#13535=CARTESIAN_POINT('Ctrl Pts',(-21.66753103807,-66.0639863052831,25.7757531447765));
#13536=CARTESIAN_POINT('Ctrl Pts',(-21.6463848903759,-66.6150259704687,
25.8127975174404));
#13537=CARTESIAN_POINT('Ctrl Pts',(-21.3250949365933,-67.1545454099721,
25.8498418901043));
#13538=CARTESIAN_POINT('Ctrl Pts',(-20.8506821176263,-67.4356536157318,
25.8868862627681));
#13539=CARTESIAN_POINT('Ctrl Pts',(-20.3762692986592,-67.7167618214914,
25.923930635432));
#13540=CARTESIAN_POINT('Ctrl Pts',(-19.7487336145077,-67.7394587935073,
25.9609750080958));
#13541=CARTESIAN_POINT('Ctrl Pts',(-19.2552515883631,-67.4933560924105,
25.9980193807597));
#13542=CARTESIAN_POINT('Ctrl Pts',(-18.7617695622185,-67.2472533913136,
26.0350637534235));
#13543=CARTESIAN_POINT('Ctrl Pts',(-18.4023411940809,-66.732351017104,26.0721081260874));
#13544=CARTESIAN_POINT('Ctrl Pts',(-18.3414460505489,-66.1842793614378,
26.1091524987512));
#13545=CARTESIAN_POINT('Ctrl Pts',(-18.2805509070169,-65.6362077057716,
26.1461968714151));
#13546=CARTESIAN_POINT('Ctrl Pts',(-18.5181889880905,-65.0549667686488,
26.1832412440789));
#13547=CARTESIAN_POINT('Ctrl Pts',(-18.9456133982649,-64.7065433741402,
26.2202856167428));
#13548=CARTESIAN_POINT('Ctrl Pts',(-19.3730378084393,-64.3581199796316,
26.2573299894066));
#13549=CARTESIAN_POINT('Ctrl Pts',(-19.9902485477144,-64.2425141277373,
26.2943743620705));
#13550=CARTESIAN_POINT('Ctrl Pts',(-20.5147973501738,-64.4126295658445,
26.3314187347344));
#13551=CARTESIAN_POINT('Ctrl Pts',(-21.0393461526331,-64.5827450039518,
26.3684631073982));
#13552=CARTESIAN_POINT('Ctrl Pts',(-21.4712330182765,-65.0385817320607,
26.4055074800621));
#13553=CARTESIAN_POINT('Ctrl Pts',(-21.6128182612061,-65.5715397750152,
26.4425518527259));
#13554=CARTESIAN_POINT('Ctrl Pts',(-21.649673613454,-65.7102714394179,26.452194689614));
#13555=CARTESIAN_POINT('Ctrl Pts',(-21.6668585011999,-65.8542287449032,
26.4618375265021));
#13556=CARTESIAN_POINT('Ctrl Pts',(-21.6655732814929,-65.9984874577248,
26.4714803633902));
#13557=CARTESIAN_POINT('Origin',(-20.,-66.,30.));
#13558=CARTESIAN_POINT('',(-21.6634529485587,-66.0005281517982,27.1714803633902));
#13559=CARTESIAN_POINT('',(-21.6666334680486,-66.0014645810993,26.9785196366098));
#13560=CARTESIAN_POINT('',(-21.666,-66.,30.));
#13561=CARTESIAN_POINT('Ctrl Pts',(-21.6666334680486,-66.0014645810993,
26.9785196366098));
#13562=CARTESIAN_POINT('Ctrl Pts',(-21.6625547837736,-65.5570900696918,
26.9487674263587));
#13563=CARTESIAN_POINT('Ctrl Pts',(-21.4793116087742,-65.1097459698003,
26.9190152161076));
#13564=CARTESIAN_POINT('Ctrl Pts',(-21.1612403596529,-64.8015501984858,
26.8892630058565));
#13565=CARTESIAN_POINT('Ctrl Pts',(-20.765210962621,-64.417816724245,26.8522186331926));
#13566=CARTESIAN_POINT('Ctrl Pts',(-20.1601622836896,-64.2498000723804,
26.8151742605288));
#13567=CARTESIAN_POINT('Ctrl Pts',(-19.6229765727187,-64.3743879797908,
26.7781298878649));
#13568=CARTESIAN_POINT('Ctrl Pts',(-19.0857908617477,-64.4989758872013,
26.7410855152011));
#13569=CARTESIAN_POINT('Ctrl Pts',(-18.6164681187371,-64.9161683538868,
26.7040411425372));
#13570=CARTESIAN_POINT('Ctrl Pts',(-18.4297795332059,-65.4350498759485,
26.6669967698734));
#13571=CARTESIAN_POINT('Ctrl Pts',(-18.2430909476747,-65.9539313980101,
26.6299523972095));
#13572=CARTESIAN_POINT('Ctrl Pts',(-18.3390365196228,-66.5745019754479,
26.5929080245457));
#13573=CARTESIAN_POINT('Ctrl Pts',(-18.6737099340405,-67.0127763409396,
26.5558636518818));
#13574=CARTESIAN_POINT('Ctrl Pts',(-19.0083833484582,-67.4510507064314,
26.518819279218));
#13575=CARTESIAN_POINT('Ctrl Pts',(-19.5817846053455,-67.7070288599771,
26.4817749065541));
#13576=CARTESIAN_POINT('Ctrl Pts',(-20.1315134729593,-67.663570077923,26.4447305338903));
#13577=CARTESIAN_POINT('Ctrl Pts',(-20.6812423405732,-67.6201112958688,
26.4076861612264));
#13578=CARTESIAN_POINT('Ctrl Pts',(-21.2072988189137,-67.2772155782147,
26.3706417885626));
#13579=CARTESIAN_POINT('Ctrl Pts',(-21.4689501718534,-66.7917989189509,
26.3335974158987));
#13580=CARTESIAN_POINT('Ctrl Pts',(-21.5986250674048,-66.5512255227818,
26.3152381561357));
#13581=CARTESIAN_POINT('Ctrl Pts',(-21.6633564594476,-66.275645962275,26.2968788963728));
#13582=CARTESIAN_POINT('Ctrl Pts',(-21.6632974926259,-66.0000402088307,
26.2785196366098));
#13583=CARTESIAN_POINT('Ctrl Pts',(-21.6655732814929,-65.9984874577248,
26.4714803633902));
#13584=CARTESIAN_POINT('Ctrl Pts',(-21.6619211411332,-66.4084197552654,
26.498881899166));
#13585=CARTESIAN_POINT('Ctrl Pts',(-21.5091236946976,-66.8207859038016,
26.5262834349417));
#13586=CARTESIAN_POINT('Ctrl Pts',(-21.2347245419387,-67.1225935870211,
26.5536849707175));
#13587=CARTESIAN_POINT('Ctrl Pts',(-20.8637619595262,-67.5306099982724,
26.5907293433813));
#13588=CARTESIAN_POINT('Ctrl Pts',(-20.2705531744855,-67.7365634629749,
26.6277737160452));
#13589=CARTESIAN_POINT('Ctrl Pts',(-19.7265622622826,-67.6462055929746,
26.664818088709));
#13590=CARTESIAN_POINT('Ctrl Pts',(-19.1825713500797,-67.5558477229742,
26.7018624613729));
#13591=CARTESIAN_POINT('Ctrl Pts',(-18.6877983107146,-67.1691785182711,
26.7389068340367));
#13592=CARTESIAN_POINT('Ctrl Pts',(-18.4686609933462,-66.6631454313498,
26.7759512067006));
#13593=CARTESIAN_POINT('Ctrl Pts',(-18.2495236759778,-66.1571123444284,
26.8129955793644));
#13594=CARTESIAN_POINT('Ctrl Pts',(-18.306022080606,-65.5317153752889,26.8500399520283));
#13595=CARTESIAN_POINT('Ctrl Pts',(-18.6123014407894,-65.0731484772605,
26.8870843246922));
#13596=CARTESIAN_POINT('Ctrl Pts',(-18.9185808009729,-64.6145815792321,
26.924128697356));
#13597=CARTESIAN_POINT('Ctrl Pts',(-19.4746411167116,-64.3228447523148,
26.9611730700199));
#13598=CARTESIAN_POINT('Ctrl Pts',(-20.0260182366421,-64.3314425135629,
26.9982174426837));
#13599=CARTESIAN_POINT('Ctrl Pts',(-20.5773953565726,-64.3400402748111,
27.0352618153476));
#13600=CARTESIAN_POINT('Ctrl Pts',(-21.124089280695,-64.6489726242249,27.0723061880114));
#13601=CARTESIAN_POINT('Ctrl Pts',(-21.4159221143717,-65.1168660371111,
27.1093505606753));
#13602=CARTESIAN_POINT('Ctrl Pts',(-21.5790734477433,-65.3784453571158,
27.1300604949136));
#13603=CARTESIAN_POINT('Ctrl Pts',(-21.6625691491406,-65.6897072078986,
27.1507704291519));
#13604=CARTESIAN_POINT('Ctrl Pts',(-21.6634529485587,-66.0005281517982,
27.1714803633902));
#13605=CARTESIAN_POINT('Origin',(-20.,-66.,30.));
#13606=CARTESIAN_POINT('',(-21.667507987647,-66.0012330299472,27.8714803633902));
#13607=CARTESIAN_POINT('',(-21.668061697955,-65.9990409238289,27.6785196366098));
#13608=CARTESIAN_POINT('',(-21.666,-66.,30.));
#13609=CARTESIAN_POINT('Ctrl Pts',(-21.668061697955,-65.9990409238289,27.6785196366098));
#13610=CARTESIAN_POINT('Ctrl Pts',(-21.6684477978651,-65.9427845343911,
27.6747447016723));
#13611=CARTESIAN_POINT('Ctrl Pts',(-21.6658484802025,-65.8865642454305,
27.6709697667349));
#13612=CARTESIAN_POINT('Ctrl Pts',(-21.6601461398808,-65.8306604734177,
27.6671948317974));
#13613=CARTESIAN_POINT('Ctrl Pts',(-21.6041876602164,-65.2820628954279,
27.6301504591336));
#13614=CARTESIAN_POINT('Ctrl Pts',(-21.2494086074079,-64.7639458475939,
27.5931060864697));
#13615=CARTESIAN_POINT('Ctrl Pts',(-20.7581628574682,-64.5134098873652,
27.5560617138059));
#13616=CARTESIAN_POINT('Ctrl Pts',(-20.2669171075285,-64.2628739271364,
27.519017341142));
#13617=CARTESIAN_POINT('Ctrl Pts',(-19.6392046604576,-64.2799190545128,
27.4819729684782));
#13618=CARTESIAN_POINT('Ctrl Pts',(-19.1622790863643,-64.5567450839289,
27.4449285958143));
#13619=CARTESIAN_POINT('Ctrl Pts',(-18.6853535122711,-64.8335711133449,
27.4078842231505));
#13620=CARTESIAN_POINT('Ctrl Pts',(-18.3592148111555,-65.3701780448006,
27.3708398504866));
#13621=CARTESIAN_POINT('Ctrl Pts',(-18.3331104688645,-65.9210039858079,
27.3337954778227));
#13622=CARTESIAN_POINT('Ctrl Pts',(-18.3070061265735,-66.4718299268152,
27.2967511051589));
#13623=CARTESIAN_POINT('Ctrl Pts',(-18.580936143107,-67.0368748773742,27.259706732495));
#13624=CARTESIAN_POINT('Ctrl Pts',(-19.0295447562574,-67.3575631487953,
27.2226623598312));
#13625=CARTESIAN_POINT('Ctrl Pts',(-19.4781533694078,-67.6782514202164,
27.1856179871673));
#13626=CARTESIAN_POINT('Ctrl Pts',(-20.1014405791751,-67.7545830124997,
27.1485736145035));
#13627=CARTESIAN_POINT('Ctrl Pts',(-20.6141778837267,-67.5516270855043,
27.1115292418396));
#13628=CARTESIAN_POINT('Ctrl Pts',(-21.1269151882782,-67.3486711585089,
27.0744848691758));
#13629=CARTESIAN_POINT('Ctrl Pts',(-21.529102587614,-66.8664277122347,27.0374404965119));
#13630=CARTESIAN_POINT('Ctrl Pts',(-21.6366912297157,-66.3255808407892,
27.0003961238481));
#13631=CARTESIAN_POINT('Ctrl Pts',(-21.6578699890131,-66.2191154603979,
26.9931039614353));
#13632=CARTESIAN_POINT('Ctrl Pts',(-21.6676331392633,-66.1103792157407,
26.9858117990226));
#13633=CARTESIAN_POINT('Ctrl Pts',(-21.6666334680486,-66.0014645810993,
26.9785196366098));
#13634=CARTESIAN_POINT('Ctrl Pts',(-21.6634529485587,-66.0005281517982,
27.1714803633902));
#13635=CARTESIAN_POINT('Ctrl Pts',(-21.6641500230646,-66.2456803338898,
27.1878148018157));
#13636=CARTESIAN_POINT('Ctrl Pts',(-21.6134553249685,-66.4905582336354,
27.2041492402413));
#13637=CARTESIAN_POINT('Ctrl Pts',(-21.5099183448232,-66.7105685223684,
27.2204836786668));
#13638=CARTESIAN_POINT('Ctrl Pts',(-21.2751099983669,-67.2095231183808,
27.2575280513307));
#13639=CARTESIAN_POINT('Ctrl Pts',(-20.7685215622234,-67.580577834047,27.2945724239945));
#13640=CARTESIAN_POINT('Ctrl Pts',(-20.2219778753094,-67.6539307287216,
27.3316167966584));
#13641=CARTESIAN_POINT('Ctrl Pts',(-19.6754341883954,-67.7272836233961,
27.3686611693222));
#13642=CARTESIAN_POINT('Ctrl Pts',(-19.0889352507107,-67.5029346970789,
27.4057055419861));
#13643=CARTESIAN_POINT('Ctrl Pts',(-18.7308745178381,-67.0835504338329,
27.4427499146499));
#13644=CARTESIAN_POINT('Ctrl Pts',(-18.3728137849654,-66.6641661705869,
27.4797942873138));
#13645=CARTESIAN_POINT('Ctrl Pts',(-18.2431912569046,-66.049746570412,27.5168386599777));
#13646=CARTESIAN_POINT('Ctrl Pts',(-18.4013247536879,-65.5214621338897,
27.5538830326415));
#13647=CARTESIAN_POINT('Ctrl Pts',(-18.5594582504713,-64.9931776973674,
27.5909274053054));
#13648=CARTESIAN_POINT('Ctrl Pts',(-19.0053477720987,-64.5510284244976,
27.6279717779692));
#13649=CARTESIAN_POINT('Ctrl Pts',(-19.5349454983304,-64.3973505240179,
27.6650161506331));
#13650=CARTESIAN_POINT('Ctrl Pts',(-20.064543224562,-64.2436726235382,27.7020605232969));
#13651=CARTESIAN_POINT('Ctrl Pts',(-20.6778491553978,-64.3784660954486,
27.7391048959608));
#13652=CARTESIAN_POINT('Ctrl Pts',(-21.0942024272058,-64.7400467942635,
27.7761492686246));
#13653=CARTESIAN_POINT('Ctrl Pts',(-21.4513544078936,-65.0502143166643,
27.8079263002132));
#13654=CARTESIAN_POINT('Ctrl Pts',(-21.6635811543817,-65.5272604795206,
27.8397033318017));
#13655=CARTESIAN_POINT('Ctrl Pts',(-21.667507987647,-66.0012330299472,27.8714803633902));
#13656=CARTESIAN_POINT('Origin',(-20.,-66.,30.));
#13657=CARTESIAN_POINT('',(-21.6672880470512,-65.9986896255742,28.5714803633902));
#13658=CARTESIAN_POINT('',(-21.6637335962722,-65.999144500325,28.3785196366098));
#13659=CARTESIAN_POINT('',(-21.666,-66.,30.));
#13660=CARTESIAN_POINT('Ctrl Pts',(-21.6637335962722,-65.999144500325,28.3785196366098));
#13661=CARTESIAN_POINT('Ctrl Pts',(-21.6647696506054,-65.7764847271083,
28.3636776043221));
#13662=CARTESIAN_POINT('Ctrl Pts',(-21.6232171112865,-65.5541957879046,
28.3488355720345));
#13663=CARTESIAN_POINT('Ctrl Pts',(-21.5372474702476,-65.3506685773165,
28.3339935397468));
#13664=CARTESIAN_POINT('Ctrl Pts',(-21.3226750074813,-64.8426830339538,
28.2969491670829));
#13665=CARTESIAN_POINT('Ctrl Pts',(-20.8314033075768,-64.451574904792,28.2599047944191));
#13666=CARTESIAN_POINT('Ctrl Pts',(-20.2882479685347,-64.3563229666671,
28.2228604217552));
#13667=CARTESIAN_POINT('Ctrl Pts',(-19.7450926294927,-64.2610710285423,
28.1858160490913));
#13668=CARTESIAN_POINT('Ctrl Pts',(-19.1500536513131,-64.4616752814544,
28.1487716764275));
#13669=CARTESIAN_POINT('Ctrl Pts',(-18.7754325806809,-64.8663352714203,
28.1117273037637));
#13670=CARTESIAN_POINT('Ctrl Pts',(-18.4008115100487,-65.2709952613862,
28.0746829310998));
#13671=CARTESIAN_POINT('Ctrl Pts',(-18.2466083469639,-65.8797109884059,
28.037638558436));
#13672=CARTESIAN_POINT('Ctrl Pts',(-18.3833894935089,-66.4139221563812,
28.0005941857721));
#13673=CARTESIAN_POINT('Ctrl Pts',(-18.5201706400539,-66.9481333243564,
27.9635498131082));
#13674=CARTESIAN_POINT('Ctrl Pts',(-18.9479360962286,-67.4078399332872,
27.9265054404444));
#13675=CARTESIAN_POINT('Ctrl Pts',(-19.4709319710131,-67.5826711919994,
27.8894610677805));
#13676=CARTESIAN_POINT('Ctrl Pts',(-19.9939278457975,-67.7575024507116,
27.8524166951167));
#13677=CARTESIAN_POINT('Ctrl Pts',(-20.6121541391916,-67.6474583592052,
27.8153723224528));
#13678=CARTESIAN_POINT('Ctrl Pts',(-21.0426983326285,-67.3028972593792,
27.778327949789));
#13679=CARTESIAN_POINT('Ctrl Pts',(-21.429368755205,-66.9934479900496,27.7450585120626));
#13680=CARTESIAN_POINT('Ctrl Pts',(-21.6646589037003,-66.494842434616,27.7117890743362));
#13681=CARTESIAN_POINT('Ctrl Pts',(-21.668061697955,-65.9990409238289,27.6785196366098));
#13682=CARTESIAN_POINT('Ctrl Pts',(-21.667507987647,-66.0012330299472,27.8714803633902));
#13683=CARTESIAN_POINT('Ctrl Pts',(-21.668158897097,-66.0797984263558,27.8767477044656));
#13684=CARTESIAN_POINT('Ctrl Pts',(-21.6630865222461,-66.1582793716597,
27.8820150455409));
#13685=CARTESIAN_POINT('Ctrl Pts',(-21.6520022273457,-66.2359018296592,
27.8872823866162));
#13686=CARTESIAN_POINT('Ctrl Pts',(-21.5740481428971,-66.7818082405207,
27.9243267592801));
#13687=CARTESIAN_POINT('Ctrl Pts',(-21.1987393612196,-67.2852531365244,
27.9613711319439));
#13688=CARTESIAN_POINT('Ctrl Pts',(-20.6978245668292,-67.5158502255527,
27.9984155046077));
#13689=CARTESIAN_POINT('Ctrl Pts',(-20.1969097724387,-67.7464473145809,
28.0354598772716));
#13690=CARTESIAN_POINT('Ctrl Pts',(-19.5703889653353,-67.7041965966336,
28.0725042499355));
#13691=CARTESIAN_POINT('Ctrl Pts',(-19.1049703966511,-67.4084328317332,
28.1095486225993));
#13692=CARTESIAN_POINT('Ctrl Pts',(-18.6395518279668,-67.1126690668328,
28.1465929952632));
#13693=CARTESIAN_POINT('Ctrl Pts',(-18.3352354977017,-66.5633922549793,
28.183637367927));
#13694=CARTESIAN_POINT('Ctrl Pts',(-18.3312825474759,-66.0119622749373,
28.2206817405908));
#13695=CARTESIAN_POINT('Ctrl Pts',(-18.3273295972502,-65.4605322948953,
28.2577261132547));
#13696=CARTESIAN_POINT('Ctrl Pts',(-18.6237400270638,-64.9069491466648,
28.2947704859186));
#13697=CARTESIAN_POINT('Ctrl Pts',(-19.0848705909317,-64.6045433732873,
28.3318148585824));
#13698=CARTESIAN_POINT('Ctrl Pts',(-19.5460011547996,-64.3021375999098,
28.3688592312463));
#13699=CARTESIAN_POINT('Ctrl Pts',(-20.1718518527218,-64.2509092013851,
28.4059036039101));
#13700=CARTESIAN_POINT('Ctrl Pts',(-20.6760210887083,-64.4743013010429,
28.442947976574));
#13701=CARTESIAN_POINT('Ctrl Pts',(-21.1801903246949,-64.6976934007006,
28.4799923492378));
#13702=CARTESIAN_POINT('Ctrl Pts',(-21.5626780987458,-65.1957059985407,
28.5170367219017));
#13703=CARTESIAN_POINT('Ctrl Pts',(-21.6484504781688,-65.7404387289994,
28.5540810945655));
#13704=CARTESIAN_POINT('Ctrl Pts',(-21.6618792086344,-65.8257233982873,
28.5598808508404));
#13705=CARTESIAN_POINT('Ctrl Pts',(-21.6680349141495,-65.9121532615772,
28.5656806071153));
#13706=CARTESIAN_POINT('Ctrl Pts',(-21.6672880470512,-65.9986896255742,
28.5714803633902));
#13707=CARTESIAN_POINT('Origin',(-20.,-66.,30.));
#13708=CARTESIAN_POINT('',(-21.6633862072226,-65.9995968836612,29.2714803633902));
#13709=CARTESIAN_POINT('',(-21.6649409508278,-66.0014219187278,29.0785196366098));
#13710=CARTESIAN_POINT('',(-21.666,-66.,30.));
#13711=CARTESIAN_POINT('Ctrl Pts',(-21.6649409508278,-66.0014219187278,
29.0785196366098));
#13712=CARTESIAN_POINT('Ctrl Pts',(-21.6617887517993,-65.6134426418904,
29.0526105069719));
#13713=CARTESIAN_POINT('Ctrl Pts',(-21.5266091317759,-65.2234833383847,
29.026701377334));
#13714=CARTESIAN_POINT('Ctrl Pts',(-21.2788296086732,-64.9279198195793,
29.0007922476961));
#13715=CARTESIAN_POINT('Ctrl Pts',(-20.9245592367783,-64.5053288144204,
28.9637478750323));
#13716=CARTESIAN_POINT('Ctrl Pts',(-20.3401039506114,-64.2757085402715,
28.9267035023684));
#13717=CARTESIAN_POINT('Ctrl Pts',(-19.7929219910902,-64.3441377534661,
28.8896591297046));
#13718=CARTESIAN_POINT('Ctrl Pts',(-19.2457400315691,-64.4125669666608,
28.8526147570407));
#13719=CARTESIAN_POINT('Ctrl Pts',(-18.7358313986938,-64.7790456671989,
28.8155703843769));
#13720=CARTESIAN_POINT('Ctrl Pts',(-18.4965403177724,-65.2758659894837,
28.778526011713));
#13721=CARTESIAN_POINT('Ctrl Pts',(-18.2572492368509,-65.7726863117686,
28.7414816390492));
#13722=CARTESIAN_POINT('Ctrl Pts',(-18.2885757078835,-66.3998482558001,
28.7044372663853));
#13723=CARTESIAN_POINT('Ctrl Pts',(-18.576184121226,-66.8703501735627,28.6673928937214));
#13724=CARTESIAN_POINT('Ctrl Pts',(-18.8637925345685,-67.3408520913253,
28.6303485210576));
#13725=CARTESIAN_POINT('Ctrl Pts',(-19.4076828902209,-67.654693982819,28.5933041483937));
#13726=CARTESIAN_POINT('Ctrl Pts',(-19.9589602577799,-67.6682556221481,
28.5562597757299));
#13727=CARTESIAN_POINT('Ctrl Pts',(-20.5102376253389,-67.6818172614771,
28.519215403066));
#13728=CARTESIAN_POINT('Ctrl Pts',(-21.0689020048045,-67.3950986486416,
28.4821710304022));
#13729=CARTESIAN_POINT('Ctrl Pts',(-21.3792975817233,-66.9393078634422,
28.4451266577383));
#13730=CARTESIAN_POINT('Ctrl Pts',(-21.565331458246,-66.6661321710056,28.4229243173621));
#13731=CARTESIAN_POINT('Ctrl Pts',(-21.6621837525239,-66.3322234195205,
28.400721976986));
#13732=CARTESIAN_POINT('Ctrl Pts',(-21.6637335962722,-65.999144500325,28.3785196366098));
#13733=CARTESIAN_POINT('Ctrl Pts',(-21.6672880470512,-65.9986896255742,
28.5714803633902));
#13734=CARTESIAN_POINT('Ctrl Pts',(-21.6632645028067,-66.4648808530385,
28.6027249797792));
#13735=CARTESIAN_POINT('Ctrl Pts',(-21.4589128498261,-66.934162969427,28.6339695961681));
#13736=CARTESIAN_POINT('Ctrl Pts',(-21.1121531076304,-67.2441368484079,
28.6652142125571));
#13737=CARTESIAN_POINT('Ctrl Pts',(-20.7010263728738,-67.6116493742805,
28.7022585852209));
#13738=CARTESIAN_POINT('Ctrl Pts',(-20.0897159185654,-67.7552215629484,
28.7393029578848));
#13739=CARTESIAN_POINT('Ctrl Pts',(-19.557969439069,-67.6091519554042,28.7763473305487));
#13740=CARTESIAN_POINT('Ctrl Pts',(-19.0262229595727,-67.46308234786,28.8133917032125));
#13741=CARTESIAN_POINT('Ctrl Pts',(-18.5740404548885,-67.0273709441037,
28.8504360758764));
#13742=CARTESIAN_POINT('Ctrl Pts',(-18.4083495380249,-66.5014078572109,
28.8874804485402));
#13743=CARTESIAN_POINT('Ctrl Pts',(-18.2426586211614,-65.9754447703182,
28.9245248212041));
#13744=CARTESIAN_POINT('Ctrl Pts',(-18.3634592921185,-65.3592300002889,
28.9615691938679));
#13745=CARTESIAN_POINT('Ctrl Pts',(-18.7154707865322,-64.9347555528772,
28.9986135665318));
#13746=CARTESIAN_POINT('Ctrl Pts',(-19.0674822809459,-64.5102811054654,
29.0356579391956));
#13747=CARTESIAN_POINT('Ctrl Pts',(-19.6507045988162,-64.2775469806712,
29.0727023118595));
#13748=CARTESIAN_POINT('Ctrl Pts',(-20.1982437297823,-64.3430568941632,
29.1097466845233));
#13749=CARTESIAN_POINT('Ctrl Pts',(-20.7457828607485,-64.4085668076551,
29.1467910571872));
#13750=CARTESIAN_POINT('Ctrl Pts',(-21.2576388048104,-64.7723207594334,
29.183835429851));
#13751=CARTESIAN_POINT('Ctrl Pts',(-21.4995762087385,-65.2678577825561,
29.2208798025149));
#13752=CARTESIAN_POINT('Ctrl Pts',(-21.6097339057125,-65.4934831565009,
29.23774665614));
#13753=CARTESIAN_POINT('Ctrl Pts',(-21.6639343505905,-65.7464286935643,
29.2546135097651));
#13754=CARTESIAN_POINT('Ctrl Pts',(-21.6633862072226,-65.9995968836612,
29.2714803633902));
#13755=CARTESIAN_POINT('Origin',(-20.,-66.,30.));
#13756=CARTESIAN_POINT('',(-21.6658101117288,-66.0015225986475,29.9714803633902));
#13757=CARTESIAN_POINT('',(-21.6687601732843,-66.0000189542795,29.7785196366098));
#13758=CARTESIAN_POINT('',(-21.666,-66.,30.));
#13759=CARTESIAN_POINT('Ctrl Pts',(-21.6687600689797,-66.0000189535633,
29.7785196366098));
#13760=CARTESIAN_POINT('Ctrl Pts',(-21.6686675101817,-65.4495889757353,
29.7415434096217));
#13761=CARTESIAN_POINT('Ctrl Pts',(-21.3695595260236,-64.8990728100273,
29.7045671826336));
#13762=CARTESIAN_POINT('Ctrl Pts',(-20.9076739098537,-64.5996824807776,
29.6675909556455));
#13763=CARTESIAN_POINT('Ctrl Pts',(-20.4449370573627,-64.2997403873821,
29.6305465829816));
#13764=CARTESIAN_POINT('Ctrl Pts',(-19.8188220349343,-64.2518506127082,
29.5935022103178));
#13765=CARTESIAN_POINT('Ctrl Pts',(-19.3158513986555,-64.4779284601082,
29.5564578376539));
#13766=CARTESIAN_POINT('Ctrl Pts',(-18.8128807623766,-64.7040063075082,
29.5194134649901));
#13767=CARTESIAN_POINT('Ctrl Pts',(-18.4330545122472,-65.2040517769822,
29.4823690923262));
#13768=CARTESIAN_POINT('Ctrl Pts',(-18.3501886152343,-65.7492342208998,
29.4453247196624));
#13769=CARTESIAN_POINT('Ctrl Pts',(-18.2673227182214,-66.2944166648174,
29.4082803469985));
#13770=CARTESIAN_POINT('Ctrl Pts',(-18.4814171743249,-66.8847360831788,
29.3712359743347));
#13771=CARTESIAN_POINT('Ctrl Pts',(-18.894498147094,-67.2500506927688,29.3341916016708));
#13772=CARTESIAN_POINT('Ctrl Pts',(-19.3075791198632,-67.6153653023587,
29.297147229007));
#13773=CARTESIAN_POINT('Ctrl Pts',(-19.9196466092979,-67.7556751031773,
29.2601028563431));
#13774=CARTESIAN_POINT('Ctrl Pts',(-20.4506064868622,-67.6067715690999,
29.2230584836792));
#13775=CARTESIAN_POINT('Ctrl Pts',(-20.9815663644265,-67.4578680350225,
29.1860141110154));
#13776=CARTESIAN_POINT('Ctrl Pts',(-21.4314186301202,-67.0197511660492,
29.1489697383515));
#13777=CARTESIAN_POINT('Ctrl Pts',(-21.5943020341556,-66.4929118634782,
29.1119253656877));
#13778=CARTESIAN_POINT('Ctrl Pts',(-21.6432634865546,-66.3345481702125,
29.1007901226617));
#13779=CARTESIAN_POINT('Ctrl Pts',(-21.6662957050299,-66.1681679112409,
29.0896548796358));
#13780=CARTESIAN_POINT('Ctrl Pts',(-21.6649409508278,-66.0014219187278,
29.0785196366098));
#13781=CARTESIAN_POINT('Ctrl Pts',(-21.6633862072226,-65.9995968836612,
29.2714803633902));
#13782=CARTESIAN_POINT('Ctrl Pts',(-21.6627304729945,-66.3024575172582,
29.291657882429));
#13783=CARTESIAN_POINT('Ctrl Pts',(-21.5837245035949,-66.6056367877023,
29.3118354014677));
#13784=CARTESIAN_POINT('Ctrl Pts',(-21.4284375187128,-66.8627440451906,
29.3320129205065));
#13785=CARTESIAN_POINT('Ctrl Pts',(-21.1433425609645,-67.334773190235,29.3690572931703));
#13786=CARTESIAN_POINT('Ctrl Pts',(-20.6011337816736,-67.6515113858566,
29.4061016658341));
#13787=CARTESIAN_POINT('Ctrl Pts',(-20.0499365888083,-67.6680130003919,
29.443146038498));
#13788=CARTESIAN_POINT('Ctrl Pts',(-19.498739395943,-67.6845146149272,29.4801904111618));
#13789=CARTESIAN_POINT('Ctrl Pts',(-18.9385537895033,-67.4007796483764,
29.5172347838257));
#13790=CARTESIAN_POINT('Ctrl Pts',(-18.6257317273414,-66.9466508052827,
29.5542791564896));
#13791=CARTESIAN_POINT('Ctrl Pts',(-18.3129096651795,-66.4925219621889,
29.5913235291534));
#13792=CARTESIAN_POINT('Ctrl Pts',(-18.2474511472954,-65.8679992425523,
29.6283679018173));
#13793=CARTESIAN_POINT('Ctrl Pts',(-18.4593112796838,-65.358876533366,29.6654122744811));
#13794=CARTESIAN_POINT('Ctrl Pts',(-18.6711714120723,-64.8497538241797,
29.702456647145));
#13795=CARTESIAN_POINT('Ctrl Pts',(-19.1603501947334,-64.4560311254436,
29.7395010198088));
#13796=CARTESIAN_POINT('Ctrl Pts',(-19.7029897897767,-64.3578836924866,
29.7765453924727));
#13797=CARTESIAN_POINT('Ctrl Pts',(-20.2456293848201,-64.2597362595296,
29.8135897651365));
#13798=CARTESIAN_POINT('Ctrl Pts',(-20.8417297922457,-64.4571640923516,
29.8506341378004));
#13799=CARTESIAN_POINT('Ctrl Pts',(-21.2185037344739,-64.8598203293115,
29.8876785104643));
#13800=CARTESIAN_POINT('Ctrl Pts',(-21.5026166529591,-65.1634502405319,
29.9156124614396));
#13801=CARTESIAN_POINT('Ctrl Pts',(-21.6620166986301,-65.5837766199149,
29.9435464124149));
#13802=CARTESIAN_POINT('Ctrl Pts',(-21.6658101117288,-66.0015225986475,
29.9714803633902));
#13803=CARTESIAN_POINT('Origin',(-20.,-66.,30.));
#13804=CARTESIAN_POINT('',(-21.6685541439151,-65.9994693779326,30.6714803633902));
#13805=CARTESIAN_POINT('',(-21.6649962084657,-65.998566115082,30.4785196366098));
#13806=CARTESIAN_POINT('',(-21.666,-66.,30.));
#13807=CARTESIAN_POINT('Ctrl Pts',(-21.6649962084657,-65.998566115082,30.4785196366098));
#13808=CARTESIAN_POINT('Ctrl Pts',(-21.6663489160884,-65.8338748640736,
30.4675206849354));
#13809=CARTESIAN_POINT('Ctrl Pts',(-21.6438880711133,-65.6695444194489,
30.4565217332609));
#13810=CARTESIAN_POINT('Ctrl Pts',(-21.5961003017824,-65.5129426030537,
30.4455227815864));
#13811=CARTESIAN_POINT('Ctrl Pts',(-21.4351515142742,-64.985509060469,30.4084784089226));
#13812=CARTESIAN_POINT('Ctrl Pts',(-20.9869101831435,-64.5457441677195,
30.3714340362587));
#13813=CARTESIAN_POINT('Ctrl Pts',(-20.4565003628192,-64.3948929942162,
30.3343896635948));
#13814=CARTESIAN_POINT('Ctrl Pts',(-19.9260905424949,-64.2440418207129,
30.297345290931));
#13815=CARTESIAN_POINT('Ctrl Pts',(-19.313512232977,-64.3821043664557,30.2603009182671));
#13816=CARTESIAN_POINT('Ctrl Pts',(-18.8990933241246,-64.7459004934683,
30.2232565456033));
#13817=CARTESIAN_POINT('Ctrl Pts',(-18.4846744152722,-65.1096966204808,
30.1862121729394));
#13818=CARTESIAN_POINT('Ctrl Pts',(-18.2684149070852,-65.6992263287631,
30.1491678002756));
#13819=CARTESIAN_POINT('Ctrl Pts',(-18.3492794064557,-66.2447092219737,
30.1121234276117));
#13820=CARTESIAN_POINT('Ctrl Pts',(-18.4301439058262,-66.7901921151842,
30.0750790549479));
#13821=CARTESIAN_POINT('Ctrl Pts',(-18.8081324127541,-67.2916281933229,
30.038034682284));
#13822=CARTESIAN_POINT('Ctrl Pts',(-19.310269947728,-67.5195504388677,30.0009903096202));
#13823=CARTESIAN_POINT('Ctrl Pts',(-19.8124074827018,-67.7474726844124,
29.9639459369563));
#13824=CARTESIAN_POINT('Ctrl Pts',(-20.4386940457216,-67.7018810973633,
29.9269015642924));
#13825=CARTESIAN_POINT('Ctrl Pts',(-20.9025285803499,-67.4036392851875,
29.8898571916286));
#13826=CARTESIAN_POINT('Ctrl Pts',(-21.3672163705614,-67.1048488366504,
29.852744673289));
#13827=CARTESIAN_POINT('Ctrl Pts',(-21.6688529689417,-66.5524777713161,
29.8156321549494));
#13828=CARTESIAN_POINT('Ctrl Pts',(-21.6687600689797,-66.0000189535633,
29.7785196366098));
#13829=CARTESIAN_POINT('Ctrl Pts',(-21.6658101117288,-66.0015225986475,
29.9714803633902));
#13830=CARTESIAN_POINT('Ctrl Pts',(-21.667047301305,-66.1377669139721,29.9805907850787));
#13831=CARTESIAN_POINT('Ctrl Pts',(-21.651732877632,-66.2737367564617,29.9897012067673));
#13832=CARTESIAN_POINT('Ctrl Pts',(-21.6187951015409,-66.405294277785,29.9988116284558));
#13833=CARTESIAN_POINT('Ctrl Pts',(-21.4848650493489,-66.940227348201,30.0358560011196));
#13834=CARTESIAN_POINT('Ctrl Pts',(-21.0595574679341,-67.4022088479354,
30.0729003737835));
#13835=CARTESIAN_POINT('Ctrl Pts',(-20.5375014765234,-67.5798269510023,
30.1099447464474));
#13836=CARTESIAN_POINT('Ctrl Pts',(-20.0154454851128,-67.7574450540693,
30.1469891191112));
#13837=CARTESIAN_POINT('Ctrl Pts',(-19.3966410837063,-67.6506997604689,
30.1840334917751));
#13838=CARTESIAN_POINT('Ctrl Pts',(-18.9642653443397,-67.3084398172795,
30.2210778644389));
#13839=CARTESIAN_POINT('Ctrl Pts',(-18.531889604973,-66.9661798740901,30.2581222371028));
#13840=CARTESIAN_POINT('Ctrl Pts',(-18.2859425276461,-66.3884052813118,
30.2951666097666));
#13841=CARTESIAN_POINT('Ctrl Pts',(-18.3389743351351,-65.839517063093,30.3322109824305));
#13842=CARTESIAN_POINT('Ctrl Pts',(-18.392006142624,-65.2906288448743,30.3692553550943));
#13843=CARTESIAN_POINT('Ctrl Pts',(-18.7440168349289,-64.7706270012152,
30.4062997277582));
#13844=CARTESIAN_POINT('Ctrl Pts',(-19.2339193917479,-64.5174746093107,
30.443344100422));
#13845=CARTESIAN_POINT('Ctrl Pts',(-19.723821948567,-64.2643222174062,30.4803884730859));
#13846=CARTESIAN_POINT('Ctrl Pts',(-20.3516163699004,-64.2780192772562,
30.5174328457497));
#13847=CARTESIAN_POINT('Ctrl Pts',(-20.830011573672,-64.5522977447179,30.5544772184136));
#13848=CARTESIAN_POINT('Ctrl Pts',(-21.3084067774437,-64.8265762121797,
30.5915215910775));
#13849=CARTESIAN_POINT('Ctrl Pts',(-21.6374027636536,-65.3614360872531,
30.6285659637413));
#13850=CARTESIAN_POINT('Ctrl Pts',(-21.6664444944342,-65.9121149651648,
30.6656103364052));
#13851=CARTESIAN_POINT('Ctrl Pts',(-21.667978472302,-65.9412017030505,30.6675670120668));
#13852=CARTESIAN_POINT('Ctrl Pts',(-21.6686755990056,-65.9703325748355,
30.6695236877285));
#13853=CARTESIAN_POINT('Ctrl Pts',(-21.6685541439151,-65.9994693779326,
30.6714803633902));
#13854=CARTESIAN_POINT('Origin',(-20.,-66.,30.));
#13855=CARTESIAN_POINT('',(-21.6642459804044,-65.9988133681836,31.3714803633902));
#13856=CARTESIAN_POINT('',(-21.663702450327,-66.0008273570352,31.1785196366098));
#13857=CARTESIAN_POINT('',(-21.666,-66.,30.));
#13858=CARTESIAN_POINT('Ctrl Pts',(-21.663702450327,-66.0008273570352,31.1785196366098));
#13859=CARTESIAN_POINT('Ctrl Pts',(-21.6622144391999,-65.6697775666387,
31.1564535875851));
#13860=CARTESIAN_POINT('Ctrl Pts',(-21.5666298198028,-65.3379360420718,
31.1343875385604));
#13861=CARTESIAN_POINT('Ctrl Pts',(-21.3827355870193,-65.065760535162,31.1123214895357));
#13862=CARTESIAN_POINT('Ctrl Pts',(-21.0740148693979,-64.6088336563782,
31.0752771168719));
#13863=CARTESIAN_POINT('Ctrl Pts',(-20.5164065201483,-64.3200666557085,
31.038232744208));
#13864=CARTESIAN_POINT('Ctrl Pts',(-19.9650830935122,-64.3316049955387,
31.0011883715442));
#13865=CARTESIAN_POINT('Ctrl Pts',(-19.4137596668761,-64.3431433353688,
30.9641439988803));
#13866=CARTESIAN_POINT('Ctrl Pts',(-18.8687211628537,-64.6549870156988,
30.9270996262165));
#13867=CARTESIAN_POINT('Ctrl Pts',(-18.5793879271388,-65.1244302313857,
30.8900552535526));
#13868=CARTESIAN_POINT('Ctrl Pts',(-18.2900546914239,-65.5938734470727,
30.8530108808888));
#13869=CARTESIAN_POINT('Ctrl Pts',(-18.2564267240166,-66.2209161981167,
30.8159665082249));
#13870=CARTESIAN_POINT('Ctrl Pts',(-18.4938928445943,-66.7186113815589,
30.7789221355611));
#13871=CARTESIAN_POINT('Ctrl Pts',(-18.7313589651721,-67.2163065650011,
30.7418777628972));
#13872=CARTESIAN_POINT('Ctrl Pts',(-19.2399191737349,-67.5846541808414,
30.7048333902334));
#13873=CARTESIAN_POINT('Ctrl Pts',(-19.7868463104771,-67.655091111061,30.6677890175695));
#13874=CARTESIAN_POINT('Ctrl Pts',(-20.3337734472193,-67.7255280412805,
30.6307446449057));
#13875=CARTESIAN_POINT('Ctrl Pts',(-20.9190675121408,-67.4980542858792,
30.5937002722418));
#13876=CARTESIAN_POINT('Ctrl Pts',(-21.2748864226587,-67.0767663119687,
30.5566558995779));
#13877=CARTESIAN_POINT('Ctrl Pts',(-21.5250581128238,-66.7805641671022,
30.5306104785886));
#13878=CARTESIAN_POINT('Ctrl Pts',(-21.6617930086926,-66.3885535514064,
30.5045650575992));
#13879=CARTESIAN_POINT('Ctrl Pts',(-21.6649962084657,-65.998566115082,30.4785196366098));
#13880=CARTESIAN_POINT('Ctrl Pts',(-21.6685541439151,-65.9994693779326,
30.6714803633902));
#13881=CARTESIAN_POINT('Ctrl Pts',(-21.666376174669,-66.5219593024021,30.7065680603924));
#13882=CARTESIAN_POINT('Ctrl Pts',(-21.4009689693529,-67.0463565435816,
30.7416557573945));
#13883=CARTESIAN_POINT('Ctrl Pts',(-20.9776818232741,-67.3523680286141,
30.7767434543967));
#13884=CARTESIAN_POINT('Ctrl Pts',(-20.530789945982,-67.6754443334016,30.8137878270606));
#13885=CARTESIAN_POINT('Ctrl Pts',(-19.9079187160463,-67.7550990622266,
30.8508321997244));
#13886=CARTESIAN_POINT('Ctrl Pts',(-19.3941062662719,-67.5548806435889,
30.8878765723883));
#13887=CARTESIAN_POINT('Ctrl Pts',(-18.8802938164976,-67.3546622249512,
30.9249209450521));
#13888=CARTESIAN_POINT('Ctrl Pts',(-18.4755401468847,-66.8745706588508,
30.961965317716));
#13889=CARTESIAN_POINT('Ctrl Pts',(-18.3650685021226,-66.3343052940453,
30.9990096903798));
#13890=CARTESIAN_POINT('Ctrl Pts',(-18.2545968573606,-65.7940399292398,
31.0360540630437));
#13891=CARTESIAN_POINT('Ctrl Pts',(-18.4384072374494,-65.1936007657291,
31.0730984357075));
#13892=CARTESIAN_POINT('Ctrl Pts',(-18.8323843951074,-64.8077605812633,
31.1101428083714));
#13893=CARTESIAN_POINT('Ctrl Pts',(-19.2263615527654,-64.4219203967975,
31.1471871810353));
#13894=CARTESIAN_POINT('Ctrl Pts',(-19.8305054879926,-64.2506791913767,
31.1842315536991));
#13895=CARTESIAN_POINT('Ctrl Pts',(-20.3683480465923,-64.3724003105954,
31.221275926363));
#13896=CARTESIAN_POINT('Ctrl Pts',(-20.9061906051919,-64.4941214298141,
31.2583202990268));
#13897=CARTESIAN_POINT('Ctrl Pts',(-21.377731787164,-64.9088048736724,31.2953646716906));
#13898=CARTESIAN_POINT('Ctrl Pts',(-21.567185067798,-65.4266833373701,31.3324090443545));
#13899=CARTESIAN_POINT('Ctrl Pts',(-21.6337915817138,-65.6087550279923,
31.3454328173664));
#13900=CARTESIAN_POINT('Ctrl Pts',(-21.665531173842,-65.8035819366461,31.3584565903783));
#13901=CARTESIAN_POINT('Ctrl Pts',(-21.6642459804044,-65.9988133681836,
31.3714803633902));
#13902=CARTESIAN_POINT('Origin',(-20.,-66.,30.));
#13903=CARTESIAN_POINT('',(-21.664269144494,-66.0011975491416,32.0714803633902));
#13904=CARTESIAN_POINT('',(-21.6680158191842,-66.0009873428354,31.8785196366098));
#13905=CARTESIAN_POINT('',(-21.666,-66.,30.));
#13906=CARTESIAN_POINT('Ctrl Pts',(-21.6680158191842,-66.0009873428354,
31.8785196366098));
#13907=CARTESIAN_POINT('Ctrl Pts',(-21.6645484604468,-65.5071812065553,
31.8453864902349));
#13908=CARTESIAN_POINT('Ctrl Pts',(-21.4314257512534,-65.010531043531,31.81225334386));
#13909=CARTESIAN_POINT('Ctrl Pts',(-21.0474729911752,-64.7009382562677,
31.7791201974851));
#13910=CARTESIAN_POINT('Ctrl Pts',(-20.618196249126,-64.3547993639436,31.7420758248213));
#13911=CARTESIAN_POINT('Ctrl Pts',(-20.0003779851722,-64.2424871003486,
31.7050314521574));
#13912=CARTESIAN_POINT('Ctrl Pts',(-19.4767439954439,-64.4153977675876,
31.6679870794935));
#13913=CARTESIAN_POINT('Ctrl Pts',(-18.9531100057157,-64.5883084348267,
31.6309427068297));
#13914=CARTESIAN_POINT('Ctrl Pts',(-18.523660290213,-65.0464420328999,31.5938983341659));
#13915=CARTESIAN_POINT('Ctrl Pts',(-18.384919490238,-65.5801476113475,31.556853961502));
#13916=CARTESIAN_POINT('Ctrl Pts',(-18.246178690263,-66.1138531897951,31.5198095888381));
#13917=CARTESIAN_POINT('Ctrl Pts',(-18.3981468058157,-66.7231307486171,
31.4827652161743));
#13918=CARTESIAN_POINT('Ctrl Pts',(-18.7712802365157,-67.129162886431,31.4457208435104));
#13919=CARTESIAN_POINT('Ctrl Pts',(-19.1444136672158,-67.535195024245,31.4086764708466));
#13920=CARTESIAN_POINT('Ctrl Pts',(-19.7387124130632,-67.737981741051,31.3716320981827));
#13921=CARTESIAN_POINT('Ctrl Pts',(-20.2822136722728,-67.6447238444348,
31.3345877255189));
#13922=CARTESIAN_POINT('Ctrl Pts',(-20.8257149314825,-67.5514659478186,
31.297543352855));
#13923=CARTESIAN_POINT('Ctrl Pts',(-21.3184187040544,-67.1621634377803,
31.2604989801912));
#13924=CARTESIAN_POINT('Ctrl Pts',(-21.534854047344,-66.6549688043121,31.2234546075273));
#13925=CARTESIAN_POINT('Ctrl Pts',(-21.6223663571936,-66.4498924371922,
31.2084762838881));
#13926=CARTESIAN_POINT('Ctrl Pts',(-21.6647125048327,-66.2255422978791,
31.193497960249));
#13927=CARTESIAN_POINT('Ctrl Pts',(-21.663702450327,-66.0008273570352,31.1785196366098));
#13928=CARTESIAN_POINT('Ctrl Pts',(-21.6642459804044,-65.9988133681836,
31.3714803633902));
#13929=CARTESIAN_POINT('Ctrl Pts',(-21.661875613767,-66.3588915154422,31.3955009630422));
#13930=CARTESIAN_POINT('Ctrl Pts',(-21.5471653402657,-66.7203457219942,
31.4195215626941));
#13931=CARTESIAN_POINT('Ctrl Pts',(-21.3316726311519,-67.0056883393076,
31.4435421623461));
#13932=CARTESIAN_POINT('Ctrl Pts',(-20.9993415345756,-67.4457413940104,
31.4805865350099));
#13933=CARTESIAN_POINT('Ctrl Pts',(-20.427313962127,-67.704774019879,31.5176309076738));
#13934=CARTESIAN_POINT('Ctrl Pts',(-19.8773609883515,-67.6642477896035,
31.5546752803376));
#13935=CARTESIAN_POINT('Ctrl Pts',(-19.327408014576,-67.623721559328,31.5917196530015));
#13936=CARTESIAN_POINT('Ctrl Pts',(-18.7995296394736,-67.2836364729084,
31.6287640256653));
#13937=CARTESIAN_POINT('Ctrl Pts',(-18.5352933960363,-66.7996221586996,
31.6658083983292));
#13938=CARTESIAN_POINT('Ctrl Pts',(-18.271057152599,-66.3156078444908,31.7028527709931));
#13939=CARTESIAN_POINT('Ctrl Pts',(-18.2704630408269,-65.6876643024928,
31.7398971436569));
#13940=CARTESIAN_POINT('Ctrl Pts',(-18.5337829379588,-65.2031508553324,
31.7769415163207));
#13941=CARTESIAN_POINT('Ctrl Pts',(-18.7971028350908,-64.7186374081719,
31.8139858889846));
#13942=CARTESIAN_POINT('Ctrl Pts',(-19.3243367411268,-64.377554055849,31.8510302616485));
#13943=CARTESIAN_POINT('Ctrl Pts',(-19.8742120448026,-64.3359872528416,
31.8880746343123));
#13944=CARTESIAN_POINT('Ctrl Pts',(-20.4240873484785,-64.2944204498342,
31.9251190069762));
#13945=CARTESIAN_POINT('Ctrl Pts',(-20.9966040497942,-64.5523701961424,
31.96216337964));
#13946=CARTESIAN_POINT('Ctrl Pts',(-21.3297672392087,-64.9917936114538,
31.9992077523039));
#13947=CARTESIAN_POINT('Ctrl Pts',(-21.5464314888222,-65.2775615100873,
32.023298622666));
#13948=CARTESIAN_POINT('Ctrl Pts',(-21.6618678224006,-65.6400786537288,
32.0473894930281));
#13949=CARTESIAN_POINT('Ctrl Pts',(-21.664269144494,-66.0011975491416,32.0714803633902));
#13950=CARTESIAN_POINT('Origin',(-20.,-66.,30.));
#13951=CARTESIAN_POINT('',(-21.6685680182217,-66.0005124578236,32.7714803633902));
#13952=CARTESIAN_POINT('',(-21.666694799795,-65.9985455596449,32.5785196366098));
#13953=CARTESIAN_POINT('',(-21.666,-66.,30.));
#13954=CARTESIAN_POINT('Ctrl Pts',(-21.666694799795,-65.9985455596449,32.5785196366098));
#13955=CARTESIAN_POINT('Ctrl Pts',(-21.6676729868231,-65.8916766829262,
32.5713637655485));
#13956=CARTESIAN_POINT('Ctrl Pts',(-21.6582744615622,-65.7849791688801,
32.5642078944873));
#13957=CARTESIAN_POINT('Ctrl Pts',(-21.6378751056044,-65.6804280680173,
32.557052023426));
#13958=CARTESIAN_POINT('Ctrl Pts',(-21.5322721206239,-65.1391899839851,
32.5200076507622));
#13959=CARTESIAN_POINT('Ctrl Pts',(-21.1318572715651,-64.6554737443548,
32.4829632780983));
#13960=CARTESIAN_POINT('Ctrl Pts',(-20.6198682734443,-64.4506374198246,
32.4459189054345));
#13961=CARTESIAN_POINT('Ctrl Pts',(-20.1078792753236,-64.2458010952945,
32.4088745327706));
#13962=CARTESIAN_POINT('Ctrl Pts',(-19.4843161281408,-64.3198446858643,
32.3718301601067));
#13963=CARTESIAN_POINT('Ctrl Pts',(-19.0345335996503,-64.6388843873256,
32.3347857874429));
#13964=CARTESIAN_POINT('Ctrl Pts',(-18.5847510711598,-64.9579240887869,
32.2977414147791));
#13965=CARTESIAN_POINT('Ctrl Pts',(-18.3087491613615,-65.5219599011395,
32.2606970421152));
#13966=CARTESIAN_POINT('Ctrl Pts',(-18.3328317758437,-66.0728779365345,
32.2236526694514));
#13967=CARTESIAN_POINT('Ctrl Pts',(-18.3569143903258,-66.6237959719295,
32.1866082967875));
#13968=CARTESIAN_POINT('Ctrl Pts',(-18.6810815290885,-67.1615962303668,
32.1495639241236));
#13969=CARTESIAN_POINT('Ctrl Pts',(-19.1569879298867,-67.4401707297795,
32.1125195514598));
#13970=CARTESIAN_POINT('Ctrl Pts',(-19.6328943306849,-67.7187452291921,
32.0754751787959));
#13971=CARTESIAN_POINT('Ctrl Pts',(-20.2605399935188,-67.7380939695802,
32.0384308061321));
#13972=CARTESIAN_POINT('Ctrl Pts',(-20.7527019111292,-67.4893625865627,
32.0013864334682));
#13973=CARTESIAN_POINT('Ctrl Pts',(-21.2448638287396,-67.2406312035451,
31.9643420608044));
#13974=CARTESIAN_POINT('Ctrl Pts',(-21.6015420011265,-66.7238196971218,
31.9272976881405));
#13975=CARTESIAN_POINT('Ctrl Pts',(-21.6595134772477,-66.1754311833835,
31.8902533154767));
#13976=CARTESIAN_POINT('Ctrl Pts',(-21.6656342331172,-66.1175311187514,
31.8863420891877));
#13977=CARTESIAN_POINT('Ctrl Pts',(-21.6684251260605,-66.0592790462557,
31.8824308628988));
#13978=CARTESIAN_POINT('Ctrl Pts',(-21.6680158191842,-66.0009873428354,
31.8785196366098));
#13979=CARTESIAN_POINT('Ctrl Pts',(-21.664269144494,-66.0011975491416,32.0714803633902));
#13980=CARTESIAN_POINT('Ctrl Pts',(-21.6655603195657,-66.1953688004339,
32.084433865692));
#13981=CARTESIAN_POINT('Ctrl Pts',(-21.6341714670255,-66.3891357982996,
32.0973873679937));
#13982=CARTESIAN_POINT('Ctrl Pts',(-21.5682671171625,-66.5703501394802,
32.1103408702954));
#13983=CARTESIAN_POINT('Ctrl Pts',(-21.3797941281882,-67.0885861678804,
32.1473852429593));
#13984=CARTESIAN_POINT('Ctrl Pts',(-20.9090384727262,-67.504161140366,32.1844296156231));
#13985=CARTESIAN_POINT('Ctrl Pts',(-20.3714272030969,-67.6268997710916,
32.221473988287));
#13986=CARTESIAN_POINT('Ctrl Pts',(-19.8338159334676,-67.7496384018173,
32.2585183609508));
#13987=CARTESIAN_POINT('Ctrl Pts',(-19.229349049671,-67.579540690783,32.2955627336147));
#13988=CARTESIAN_POINT('Ctrl Pts',(-18.8346424935248,-67.1944466980488,
32.3326071062786));
#13989=CARTESIAN_POINT('Ctrl Pts',(-18.4399359373785,-66.8093527053147,
32.3696514789424));
#13990=CARTESIAN_POINT('Ctrl Pts',(-18.2549897088826,-66.2092624308807,
32.4066958516062));
#13991=CARTESIAN_POINT('Ctrl Pts',(-18.3644388419032,-65.6687889939883,
32.4437402242701));
#13992=CARTESIAN_POINT('Ctrl Pts',(-18.4738879749238,-65.1283155570959,
32.4807845969339));
#13993=CARTESIAN_POINT('Ctrl Pts',(-18.8777324694608,-64.6474589577452,
32.5178289695978));
#13994=CARTESIAN_POINT('Ctrl Pts',(-19.3911651372318,-64.4462686389668,
32.5548733422617));
#13995=CARTESIAN_POINT('Ctrl Pts',(-19.9045978050028,-64.2450783201884,
32.5919177149255));
#13996=CARTESIAN_POINT('Ctrl Pts',(-20.5276186460077,-64.3235542819823,
32.6289620875894));
#13997=CARTESIAN_POINT('Ctrl Pts',(-20.9751210624724,-64.6457843798355,
32.6660064602532));
#13998=CARTESIAN_POINT('Ctrl Pts',(-21.399835381487,-64.9516056034546,32.7011644279656));
#13999=CARTESIAN_POINT('Ctrl Pts',(-21.6664519287834,-65.4769877413138,
32.7363223956779));
#14000=CARTESIAN_POINT('Ctrl Pts',(-21.6685680182217,-66.0005124578236,
32.7714803633902));
#14001=CARTESIAN_POINT('Origin',(-20.,-66.,30.));
#14002=CARTESIAN_POINT('',(-21.665778632213,-65.9984780340856,33.4714803633902));
#14003=CARTESIAN_POINT('',(-21.6632991006019,-65.9999263102654,33.2785196366098));
#14004=CARTESIAN_POINT('',(-21.666,-66.,30.));
#14005=CARTESIAN_POINT('Ctrl Pts',(-21.6632991006019,-65.9999263102654,
33.2785196366098));
#14006=CARTESIAN_POINT('Ctrl Pts',(-21.6634070404292,-65.7263673499551,
33.2602966681983));
#14007=CARTESIAN_POINT('Ctrl Pts',(-21.5996813808277,-65.4528557432902,
33.2420736997869));
#14008=CARTESIAN_POINT('Ctrl Pts',(-21.4718465072752,-65.2135974693183,
33.2238507313754));
#14009=CARTESIAN_POINT('Ctrl Pts',(-21.2119787081117,-64.7272237642339,
33.1868063587115));
#14010=CARTESIAN_POINT('Ctrl Pts',(-20.687183619355,-64.3823997995165,33.1497619860477));
#14011=CARTESIAN_POINT('Ctrl Pts',(-20.1376178014656,-64.3369238075172,
33.1127176133838));
#14012=CARTESIAN_POINT('Ctrl Pts',(-19.5880519835761,-64.2914478155178,
33.07567324072));
#14013=CARTESIAN_POINT('Ctrl Pts',(-19.0137154365539,-64.5453197962364,
33.0386288680561));
#14014=CARTESIAN_POINT('Ctrl Pts',(-18.67743586716,-64.9823629351308,33.0015844953922));
#14015=CARTESIAN_POINT('Ctrl Pts',(-18.3411562977662,-65.4194060740252,
32.9645401227284));
#14016=CARTESIAN_POINT('Ctrl Pts',(-18.2429337060008,-66.0396203710956,
32.9274957500646));
#14017=CARTESIAN_POINT('Ctrl Pts',(-18.427716682852,-66.5591835583106,32.8904513774007));
#14018=CARTESIAN_POINT('Ctrl Pts',(-18.6124996597033,-67.0787467455257,
32.8534070047369));
#14019=CARTESIAN_POINT('Ctrl Pts',(-19.0802882051712,-67.4976588228855,
32.816362632073));
#14020=CARTESIAN_POINT('Ctrl Pts',(-19.6170130748635,-67.6242173796775,
32.7793182594091));
#14021=CARTESIAN_POINT('Ctrl Pts',(-20.1537379445558,-67.7507759364695,
32.7422738867453));
#14022=CARTESIAN_POINT('Ctrl Pts',(-20.7593991384724,-67.5849809726938,
32.7052295140814));
#14023=CARTESIAN_POINT('Ctrl Pts',(-21.1568341749797,-67.2027035265888,
32.6681851414176));
#14024=CARTESIAN_POINT('Ctrl Pts',(-21.4774965825568,-66.8942707137504,
32.638296639815));
#14025=CARTESIAN_POINT('Ctrl Pts',(-21.6626091274417,-66.4449133834543,
32.6084081382124));
#14026=CARTESIAN_POINT('Ctrl Pts',(-21.666694799795,-65.9985455596449,32.5785196366098));
#14027=CARTESIAN_POINT('Ctrl Pts',(-21.6685680182217,-66.0005124578236,
32.7714803633902));
#14028=CARTESIAN_POINT('Ctrl Pts',(-21.6686815572529,-66.0286022389381,
32.7733667683417));
#14029=CARTESIAN_POINT('Ctrl Pts',(-21.6680336333681,-66.0566866727747,
32.7752531732933));
#14030=CARTESIAN_POINT('Ctrl Pts',(-21.6666078109475,-66.0847315576818,
32.7771395782448));
#14031=CARTESIAN_POINT('Ctrl Pts',(-21.6386081510336,-66.6354644037626,
32.8141839509086));
#14032=CARTESIAN_POINT('Ctrl Pts',(-21.3106248392815,-67.1709458620117,
32.8512283235725));
#14033=CARTESIAN_POINT('Ctrl Pts',(-20.8327494937987,-67.4461290789448,
32.8882726962363));
#14034=CARTESIAN_POINT('Ctrl Pts',(-20.3548741483159,-67.7213122958779,
32.9253170689002));
#14035=CARTESIAN_POINT('Ctrl Pts',(-19.7271067691025,-67.7361972714949,
32.962361441564));
#14036=CARTESIAN_POINT('Ctrl Pts',(-19.2367260632258,-67.4839723480544,
32.9994058142279));
#14037=CARTESIAN_POINT('Ctrl Pts',(-18.7463453573491,-67.2317474246138,
33.0364501868918));
#14038=CARTESIAN_POINT('Ctrl Pts',(-18.3933513248091,-66.7124126021157,
33.0734945595556));
#14039=CARTESIAN_POINT('Ctrl Pts',(-18.3392809817557,-66.1636257156765,
33.1105389322195));
#14040=CARTESIAN_POINT('Ctrl Pts',(-18.2852106387023,-65.6148388292373,
33.1475833048833));
#14041=CARTESIAN_POINT('Ctrl Pts',(-18.5300639851355,-65.036599878857,33.1846276775472));
#14042=CARTESIAN_POINT('Ctrl Pts',(-18.9617913110511,-64.6935223879976,
33.221672050211));
#14043=CARTESIAN_POINT('Ctrl Pts',(-19.3935186369667,-64.3504448971382,
33.2587164228749));
#14044=CARTESIAN_POINT('Ctrl Pts',(-20.0121199423648,-64.2425288657996,
33.2957607955387));
#14045=CARTESIAN_POINT('Ctrl Pts',(-20.5345110959589,-64.4191587934175,
33.3328051682026));
#14046=CARTESIAN_POINT('Ctrl Pts',(-21.056902249553,-64.5957887210355,33.3698495408664));
#14047=CARTESIAN_POINT('Ctrl Pts',(-21.4830832513432,-65.05696460761,33.4068939135303));
#14048=CARTESIAN_POINT('Ctrl Pts',(-21.6180252877123,-65.5916432921331,
33.4439382861941));
#14049=CARTESIAN_POINT('Ctrl Pts',(-21.6514679198442,-65.7241525015422,
33.4531189785928));
#14050=CARTESIAN_POINT('Ctrl Pts',(-21.6670227959202,-65.8611762171652,
33.4622996709915));
#14051=CARTESIAN_POINT('Ctrl Pts',(-21.665778632213,-65.9984780340856,33.4714803633902));
#14052=CARTESIAN_POINT('Origin',(-20.,-66.,30.));
#14053=CARTESIAN_POINT('',(-21.6633939784266,-66.0004198226392,34.1714803633902));
#14054=CARTESIAN_POINT('',(-21.6664243436945,-66.0014929634474,33.9785196366098));
#14055=CARTESIAN_POINT('',(-21.666,-66.,30.));
#14056=CARTESIAN_POINT('Ctrl Pts',(-21.6664243436945,-66.0014929634474,
33.9785196366098));
#14057=CARTESIAN_POINT('Ctrl Pts',(-21.6623854969713,-65.56387976128,33.9492295708481));
#14058=CARTESIAN_POINT('Ctrl Pts',(-21.4853949308404,-65.1233755126288,
33.9199395050864));
#14059=CARTESIAN_POINT('Ctrl Pts',(-21.1760642722398,-64.8160937930611,
33.8906494393247));
#14060=CARTESIAN_POINT('Ctrl Pts',(-20.7848408353656,-64.4274617351793,
33.8536050666609));
#14061=CARTESIAN_POINT('Ctrl Pts',(-20.1819298910283,-64.2519287056668,
33.816560693997));
#14062=CARTESIAN_POINT('Ctrl Pts',(-19.6432353511812,-64.3698220749688,
33.7795163213332));
#14063=CARTESIAN_POINT('Ctrl Pts',(-19.1045408113341,-64.4877154442707,
33.7424719486693));
#14064=CARTESIAN_POINT('Ctrl Pts',(-18.6300626759773,-64.8990352123871,
33.7054275760055));
#14065=CARTESIAN_POINT('Ctrl Pts',(-18.4369314781643,-65.4155533578892,
33.6683832033416));
#14066=CARTESIAN_POINT('Ctrl Pts',(-18.2438002803514,-65.9320715033912,
33.6313388306778));
#14067=CARTESIAN_POINT('Ctrl Pts',(-18.3320160200823,-66.553788026279,33.5942944580139));
#14068=CARTESIAN_POINT('Ctrl Pts',(-18.6612094384485,-66.9961932108407,
33.5572500853501));
#14069=CARTESIAN_POINT('Ctrl Pts',(-18.9904028568147,-67.4385983954023,
33.5202057126862));
#14070=CARTESIAN_POINT('Ctrl Pts',(-19.5605739538163,-67.7016922416377,
33.4831613400223));
#14071=CARTESIAN_POINT('Ctrl Pts',(-20.1108012147773,-67.6650778276609,
33.4461169673585));
#14072=CARTESIAN_POINT('Ctrl Pts',(-20.6610284757384,-67.628463413684,33.4090725946946));
#14073=CARTESIAN_POINT('Ctrl Pts',(-21.191311900659,-67.2921407394949,33.3720282220308));
#14074=CARTESIAN_POINT('Ctrl Pts',(-21.458983358334,-66.8100176796745,33.334983849367));
#14075=CARTESIAN_POINT('Ctrl Pts',(-21.5949811455672,-66.5650619048632,
33.3161624451146));
#14076=CARTESIAN_POINT('Ctrl Pts',(-21.6631876160688,-66.2824688501306,
33.2973410408622));
#14077=CARTESIAN_POINT('Ctrl Pts',(-21.6632991006019,-65.9999263102654,
33.2785196366098));
#14078=CARTESIAN_POINT('Ctrl Pts',(-21.665778632213,-65.9984780340856,33.4714803633902));
#14079=CARTESIAN_POINT('Ctrl Pts',(-21.6620025575742,-66.4151932185574,
33.4993440436554));
#14080=CARTESIAN_POINT('Ctrl Pts',(-21.5034836506645,-66.8344701079231,
33.5272077239205));
#14081=CARTESIAN_POINT('Ctrl Pts',(-21.2206590512588,-67.1378719231945,
33.5550714041857));
#14082=CARTESIAN_POINT('Ctrl Pts',(-20.8446477074886,-67.5412403872612,
33.5921157768495));
#14083=CARTESIAN_POINT('Ctrl Pts',(-20.2489219490002,-67.7397958329229,
33.6291601495134));
#14084=CARTESIAN_POINT('Ctrl Pts',(-19.7060976064966,-67.642675382864,33.6662045221772));
#14085=CARTESIAN_POINT('Ctrl Pts',(-19.1632732639931,-67.5455549328051,
33.7032488948411));
#14086=CARTESIAN_POINT('Ctrl Pts',(-18.6733503374743,-67.1527585870256,
33.740293267505));
#14087=CARTESIAN_POINT('Ctrl Pts',(-18.4605272000038,-66.64403767922,33.7773376401688));
#14088=CARTESIAN_POINT('Ctrl Pts',(-18.2477040625333,-66.1353167714144,
33.8143820128327));
#14089=CARTESIAN_POINT('Ctrl Pts',(-18.3119807141111,-65.5106713015827,
33.8514263854965));
#14090=CARTESIAN_POINT('Ctrl Pts',(-18.6239428934263,-65.055951338178,33.8884707581604));
#14091=CARTESIAN_POINT('Ctrl Pts',(-18.9359050727415,-64.6012313747734,
33.9255151308242));
#14092=CARTESIAN_POINT('Ctrl Pts',(-19.4955527797942,-64.3164369177958,
33.9625595034881));
#14093=CARTESIAN_POINT('Ctrl Pts',(-20.0467802112671,-64.3318954984015,
33.9996038761519));
#14094=CARTESIAN_POINT('Ctrl Pts',(-20.59800764274,-64.3473540790071,34.0366482488158));
#14095=CARTESIAN_POINT('Ctrl Pts',(-21.1408147986332,-64.6630656971959,
34.0736926214796));
#14096=CARTESIAN_POINT('Ctrl Pts',(-21.4268024396972,-65.1345545373491,
34.1107369941435));
#14097=CARTESIAN_POINT('Ctrl Pts',(-21.5831181554361,-65.3922618817548,
34.1309847838924));
#14098=CARTESIAN_POINT('Ctrl Pts',(-21.6627085390352,-65.6965079757682,
34.1512325736413));
#14099=CARTESIAN_POINT('Ctrl Pts',(-21.6633939784266,-66.0004198226392,
34.1714803633902));
#14100=CARTESIAN_POINT('Origin',(-20.,-66.,30.));
#14101=CARTESIAN_POINT('',(-21.6673174954184,-66.0013023234915,34.8714803633902));
#14102=CARTESIAN_POINT('',(-21.668208945928,-65.9991411290017,34.6785196366098));
#14103=CARTESIAN_POINT('',(-21.666,-66.,30.));
#14104=CARTESIAN_POINT('Ctrl Pts',(-21.668208945928,-65.9991411290017,34.6785196366098));
#14105=CARTESIAN_POINT('Ctrl Pts',(-21.6685189954827,-65.9497833734107,
34.6752068461617));
#14106=CARTESIAN_POINT('Ctrl Pts',(-21.6665182740216,-65.9004511060839,
34.6718940557137));
#14107=CARTESIAN_POINT('Ctrl Pts',(-21.6621249449702,-65.851332844456,34.6685812652657));
#14108=CARTESIAN_POINT('Ctrl Pts',(-21.6129977450565,-65.302081324664,34.6315368926018));
#14109=CARTESIAN_POINT('Ctrl Pts',(-21.2646936610931,-64.7795895453484,
34.594492519938));
#14110=CARTESIAN_POINT('Ctrl Pts',(-20.7766036652056,-64.5229598163238,
34.5574481472741));
#14111=CARTESIAN_POINT('Ctrl Pts',(-20.2885136693181,-64.2663300872993,
34.5204037746103));
#14112=CARTESIAN_POINT('Ctrl Pts',(-19.6606377615066,-64.2755624085656,
34.4833594019464));
#14113=CARTESIAN_POINT('Ctrl Pts',(-19.1803042290292,-64.5464319940161,
34.4463150292825));
#14114=CARTESIAN_POINT('Ctrl Pts',(-18.6999706965518,-64.8173015794665,
34.4092706566187));
#14115=CARTESIAN_POINT('Ctrl Pts',(-18.3671795394086,-65.349808429101,34.3722262839548));
#14116=CARTESIAN_POINT('Ctrl Pts',(-18.3342225828221,-65.9002668758333,
34.335181911291));
#14117=CARTESIAN_POINT('Ctrl Pts',(-18.3012656262355,-66.4507253225656,
34.2981375386271));
#14118=CARTESIAN_POINT('Ctrl Pts',(-18.5681428702056,-67.0191353663957,
34.2610931659633));
#14119=CARTESIAN_POINT('Ctrl Pts',(-19.0127260145093,-67.3453814116786,
34.2240487932994));
#14120=CARTESIAN_POINT('Ctrl Pts',(-19.457309158813,-67.6716274569616,34.1870044206356));
#14121=CARTESIAN_POINT('Ctrl Pts',(-20.0795982034502,-67.7557095036974,
34.1499600479717));
#14122=CARTESIAN_POINT('Ctrl Pts',(-20.5948214457436,-67.5591499392339,
34.1129156753078));
#14123=CARTESIAN_POINT('Ctrl Pts',(-21.110044688037,-67.3625903747704,34.075871302644));
#14124=CARTESIAN_POINT('Ctrl Pts',(-21.5182021279864,-66.8853891991076,
34.0388269299801));
#14125=CARTESIAN_POINT('Ctrl Pts',(-21.6325128832557,-66.3459230681507,
34.0017825573163));
#14126=CARTESIAN_POINT('Ctrl Pts',(-21.6564409623358,-66.2329994135725,
33.9940282504141));
#14127=CARTESIAN_POINT('Ctrl Pts',(-21.6674935955452,-66.1173475027186,
33.986273943512));
#14128=CARTESIAN_POINT('Ctrl Pts',(-21.6664243436945,-66.0014929634474,
33.9785196366098));
#14129=CARTESIAN_POINT('Ctrl Pts',(-21.6633939784266,-66.0004198226392,
34.1714803633902));
#14130=CARTESIAN_POINT('Ctrl Pts',(-21.6639625856531,-66.2525303294208,
34.1882769463052));
#14131=CARTESIAN_POINT('Ctrl Pts',(-21.6102323157922,-66.5044108221688,
34.2050735292201));
#14132=CARTESIAN_POINT('Ctrl Pts',(-21.5009589145427,-66.7293033613947,
34.2218701121351));
#14133=CARTESIAN_POINT('Ctrl Pts',(-21.2599596220895,-67.2252972831696,
34.2589144847989));
#14134=CARTESIAN_POINT('Ctrl Pts',(-20.7487929109483,-67.5900190646018,
34.2959588574628));
#14135=CARTESIAN_POINT('Ctrl Pts',(-20.2013787183707,-67.6565649760457,
34.3330032301266));
#14136=CARTESIAN_POINT('Ctrl Pts',(-19.6539645257931,-67.7231108874895,
34.3700476027905));
#14137=CARTESIAN_POINT('Ctrl Pts',(-19.070302851779,-67.4914809289449,34.4070919754543));
#14138=CARTESIAN_POINT('Ctrl Pts',(-18.7174887835078,-67.0676732583278,
34.4441363481182));
#14139=CARTESIAN_POINT('Ctrl Pts',(-18.3646747152366,-66.6438655877108,
34.481180720782));
#14140=CARTESIAN_POINT('Ctrl Pts',(-18.2427082527083,-66.0278802050213,
34.5182250934459));
#14141=CARTESIAN_POINT('Ctrl Pts',(-18.4074036119675,-65.501604681277,34.5552694661097));
#14142=CARTESIAN_POINT('Ctrl Pts',(-18.5720989712267,-64.9753291575327,
34.5923138387736));
#14143=CARTESIAN_POINT('Ctrl Pts',(-19.0234561522734,-64.5387634927337,
34.6293582114374));
#14144=CARTESIAN_POINT('Ctrl Pts',(-19.5549253011755,-64.3916876550998,
34.6664025841013));
#14145=CARTESIAN_POINT('Ctrl Pts',(-20.0863944500777,-64.244611817466,34.7034469567651));
#14146=CARTESIAN_POINT('Ctrl Pts',(-20.6979755668353,-64.3870258069973,
34.740491329429));
#14147=CARTESIAN_POINT('Ctrl Pts',(-21.1097969476086,-64.7537603158085,
34.7775357020928));
#14148=CARTESIAN_POINT('Ctrl Pts',(-21.4579237781244,-65.0637736569165,
34.808850589192));
#14149=CARTESIAN_POINT('Ctrl Pts',(-21.6633042078259,-65.5340843001723,
34.8401654762911));
#14150=CARTESIAN_POINT('Ctrl Pts',(-21.6673174954184,-66.0013023234915,
34.8714803633902));
#14151=CARTESIAN_POINT('Origin',(-20.,-66.,30.));
#14152=CARTESIAN_POINT('',(-21.6674773009859,-65.998786811783,35.5714803633902));
#14153=CARTESIAN_POINT('',(-21.6638441630143,-65.999055839902,35.3785196366098));
#14154=CARTESIAN_POINT('',(-21.666,-66.,30.));
#14155=CARTESIAN_POINT('',(-18.7309291201477,-64.9206413469514,36.));
#14156=CARTESIAN_POINT('Ctrl Pts',(-21.6674773009859,-65.998786811783,35.5714803633902));
#14157=CARTESIAN_POINT('Ctrl Pts',(-21.6635425730949,-66.4716252930546,
35.6031871242686));
#14158=CARTESIAN_POINT('Ctrl Pts',(-21.4523796956911,-66.9474486915342,
35.634893885147));
#14159=CARTESIAN_POINT('Ctrl Pts',(-21.0965955086794,-67.2577323833415,
35.6666006460253));
#14160=CARTESIAN_POINT('Ctrl Pts',(-20.6809175382262,-67.6202501679528,
35.7036450186892));
#14161=CARTESIAN_POINT('Ctrl Pts',(-20.0678278060009,-67.7568020473594,
35.740689391353));
#14162=CARTESIAN_POINT('Ctrl Pts',(-19.5379530745693,-67.6038093166544,
35.7777337640169));
#14163=CARTESIAN_POINT('Ctrl Pts',(-19.0080783431377,-67.4508165859494,
35.8147781366807));
#14164=CARTESIAN_POINT('Ctrl Pts',(-18.5614186124997,-67.0082792451327,
35.8518225093446));
#14165=CARTESIAN_POINT('Ctrl Pts',(-18.4024070521432,-66.4812299699562,
35.8888668820084));
#14166=CARTESIAN_POINT('Ctrl Pts',(-18.2433954917868,-65.9541806947796,
35.9259112546723));
#14167=CARTESIAN_POINT('Ctrl Pts',(-18.372032101712,-65.3426194852432,35.9629556273362));
#14168=CARTESIAN_POINT('Ctrl Pts',(-18.7309291201477,-64.9206413469514,
36.));
#14169=CARTESIAN_POINT('',(-21.2714721999681,-64.9187950709037,36.));
#14170=CARTESIAN_POINT('Origin',(-20.,-66.,36.));
#14171=CARTESIAN_POINT('Ctrl Pts',(-21.2714736587042,-64.9187939493416,
36.));
#14172=CARTESIAN_POINT('Ctrl Pts',(-20.9206574088577,-64.5073240780818,
35.9636818543909));
#14173=CARTESIAN_POINT('Ctrl Pts',(-20.3507903997101,-64.2812824034869,
35.9273637087819));
#14174=CARTESIAN_POINT('Ctrl Pts',(-19.8134508486065,-64.3418046038641,
35.8910455631728));
#14175=CARTESIAN_POINT('Ctrl Pts',(-19.2653665165382,-64.4035370218501,
35.854001190509));
#14176=CARTESIAN_POINT('Ctrl Pts',(-18.7511235035973,-64.7634083085501,
35.8169568178451));
#14177=CARTESIAN_POINT('Ctrl Pts',(-18.5057149290944,-65.2571540728335,
35.7799124451812));
#14178=CARTESIAN_POINT('Ctrl Pts',(-18.2603063545915,-65.7508998371168,
35.7428680725174));
#14179=CARTESIAN_POINT('Ctrl Pts',(-18.2837322185265,-66.3785200789834,
35.7058236998535));
#14180=CARTESIAN_POINT('Ctrl Pts',(-18.565439975346,-66.8525938141442,35.6687793271897));
#14181=CARTESIAN_POINT('Ctrl Pts',(-18.8471477321655,-67.3266675493049,
35.6317349545258));
#14182=CARTESIAN_POINT('Ctrl Pts',(-19.3871373818695,-67.6471947777599,
35.594690581862));
#14183=CARTESIAN_POINT('Ctrl Pts',(-19.9382149975217,-67.6676009890549,
35.5576462091981));
#14184=CARTESIAN_POINT('Ctrl Pts',(-20.4892926131739,-67.68800720035,35.5206018365343));
#14185=CARTESIAN_POINT('Ctrl Pts',(-21.0514581947743,-67.4082923944853,
35.4835574638704));
#14186=CARTESIAN_POINT('Ctrl Pts',(-21.367495855437,-66.9564068860944,35.4465130912066));
#14187=CARTESIAN_POINT('Ctrl Pts',(-21.5608539895331,-66.6799343336008,
35.423848606341));
#14188=CARTESIAN_POINT('Ctrl Pts',(-21.6620806326978,-66.3390142228699,
35.4011841214754));
#14189=CARTESIAN_POINT('Ctrl Pts',(-21.6638441630143,-65.999055839902,35.3785196366098));
#14190=CARTESIAN_POINT('Origin',(-20.,-66.,37.5459252805377));
#14191=CARTESIAN_POINT('',(-22.0554079541519,-65.9981768930466,25.3540747194623));
#14192=CARTESIAN_POINT('',(-22.0529266054906,-66.0015060728813,25.2959252805377));
#14193=CARTESIAN_POINT('',(-22.05475,-65.9999999999998,37.5459252805377));
#14194=CARTESIAN_POINT('',(-18.1825721112405,-65.0413794120407,25.));
#14195=CARTESIAN_POINT('Ctrl Pts',(-22.0529266054906,-66.0015060728812,
25.2959252805377));
#14196=CARTESIAN_POINT('Ctrl Pts',(-22.0499364984145,-65.5475810030442,
25.2713722656862));
#14197=CARTESIAN_POINT('Ctrl Pts',(-21.6783088984842,-64.4040177540137,
25.2097748781708));
#14198=CARTESIAN_POINT('Ctrl Pts',(-19.7840052970778,-63.5820406376141,
25.1111331179915));
#14199=CARTESIAN_POINT('Ctrl Pts',(-18.5013225746365,-64.4370673526013,
25.0370443726639));
#14200=CARTESIAN_POINT('Ctrl Pts',(-18.1825721112405,-65.0413794120407,
25.));
#14201=CARTESIAN_POINT('',(-17.9429020987956,-66.0754554248319,25.));
#14202=CARTESIAN_POINT('Origin',(-20.,-66.,25.));
#14203=CARTESIAN_POINT('Ctrl Pts',(-22.0554079541519,-65.9981768930466,
25.3540747194623));
#14204=CARTESIAN_POINT('Ctrl Pts',(-22.0567025337672,-65.8578133551516,
25.3464567039117));
#14205=CARTESIAN_POINT('Ctrl Pts',(-21.9795742048134,-65.0363088793791,
25.3017943156971));
#14206=CARTESIAN_POINT('Ctrl Pts',(-20.8736249251117,-63.7340407352631,
25.2200875548188));
#14207=CARTESIAN_POINT('Ctrl Pts',(-18.5861500435499,-64.0348865828967,
25.109680663882));
#14208=CARTESIAN_POINT('Ctrl Pts',(-17.9193181381118,-65.408977698993,25.0363181456091));
#14209=CARTESIAN_POINT('Ctrl Pts',(-17.9428998377409,-66.0754556195432,
25.));
#14210=CARTESIAN_POINT('Origin',(-20.,-66.,37.5459252805377));
#14211=CARTESIAN_POINT('',(-22.0514168805361,-66.0000495912933,26.0540747194623));
#14212=CARTESIAN_POINT('',(-22.058013816727,-66.0004830916995,25.9959252805377));
#14213=CARTESIAN_POINT('',(-22.05475,-65.9999999999998,37.5459252805377));
#14214=CARTESIAN_POINT('Ctrl Pts',(-22.058013816727,-66.0004830916995,25.9959252805377));
#14215=CARTESIAN_POINT('Ctrl Pts',(-22.0559447889388,-65.3463924343595,
25.9603051683359));
#14216=CARTESIAN_POINT('Ctrl Pts',(-21.3649311801284,-64.0082840748463,
25.8876406834704));
#14217=CARTESIAN_POINT('Ctrl Pts',(-19.0858252946999,-63.7500130051076,
25.7779318259409));
#14218=CARTESIAN_POINT('Ctrl Pts',(-17.6139704758136,-65.5475930823177,
25.6667987079494));
#14219=CARTESIAN_POINT('Ctrl Pts',(-18.3256043860741,-67.7593785018947,
25.5556655899578));
#14220=CARTESIAN_POINT('Ctrl Pts',(-20.570308099232,-68.3606229135291,25.4445324719662));
#14221=CARTESIAN_POINT('Ctrl Pts',(-21.9115055060277,-67.1462798849558,
25.3579523688262));
#14222=CARTESIAN_POINT('Ctrl Pts',(-22.0544478238668,-66.2324406648902,
25.30841663835));
#14223=CARTESIAN_POINT('Ctrl Pts',(-22.0529266054906,-66.0015060728812,
25.2959252805377));
#14224=CARTESIAN_POINT('Ctrl Pts',(-22.0514168805361,-66.0000495912932,
26.0540747194623));
#14225=CARTESIAN_POINT('Ctrl Pts',(-22.0513428634009,-65.6540999925487,
26.0353896065614));
#14226=CARTESIAN_POINT('Ctrl Pts',(-21.8042540993797,-64.6221844734596,
25.9796601209967));
#14227=CARTESIAN_POINT('Ctrl Pts',(-20.1701400827706,-63.5773513899392,
25.8868862627681));
#14228=CARTESIAN_POINT('Ctrl Pts',(-18.0569488868988,-64.5430601781429,
25.7757531447766));
#14229=CARTESIAN_POINT('Ctrl Pts',(-17.7220730992874,-66.842211172105,25.664620026785));
#14230=CARTESIAN_POINT('Ctrl Pts',(-19.4721283107045,-68.3705502400566,
25.5534869087934));
#14231=CARTESIAN_POINT('Ctrl Pts',(-21.55207742503,-67.7732034363132,25.4499718063526));
#14232=CARTESIAN_POINT('Ctrl Pts',(-22.0504073392519,-66.540363708537,25.3835010765755));
#14233=CARTESIAN_POINT('Ctrl Pts',(-22.0554079541519,-65.9981768930466,
25.3540747194623));
#14234=CARTESIAN_POINT('Origin',(-20.,-66.,37.5459252805377));
#14235=CARTESIAN_POINT('',(-22.0555312835971,-66.0018063313406,26.7540747194623));
#14236=CARTESIAN_POINT('',(-22.0542237095723,-65.9981345160623,26.6959252805377));
#14237=CARTESIAN_POINT('',(-22.05475,-65.9999999999998,37.5459252805377));
#14238=CARTESIAN_POINT('Ctrl Pts',(-22.0542237095723,-65.9981345160623,
26.6959252805377));
#14239=CARTESIAN_POINT('Ctrl Pts',(-22.0558088267349,-65.8202139937513,
26.6862824436496));
#14240=CARTESIAN_POINT('Ctrl Pts',(-21.9531907694769,-64.9605855088004,
26.6395952340976));
#14241=CARTESIAN_POINT('Ctrl Pts',(-20.7492058643109,-63.6898348017937,
26.5558636518818));
#14242=CARTESIAN_POINT('Ctrl Pts',(-18.465507605261,-64.1175799233661,26.4447305338903));
#14243=CARTESIAN_POINT('Ctrl Pts',(-17.5862395732934,-66.2681888349264,
26.3335974158987));
#14244=CARTESIAN_POINT('Ctrl Pts',(-18.9161353225687,-68.1733430727544,
26.2224642979071));
#14245=CARTESIAN_POINT('Ctrl Pts',(-21.2380361875332,-68.089363595114,26.1113311799156));
#14246=CARTESIAN_POINT('Ctrl Pts',(-22.0457930405706,-66.7329547828402,
26.0358181741258));
#14247=CARTESIAN_POINT('Ctrl Pts',(-22.0580965462382,-66.0266367280669,
25.9973495409998));
#14248=CARTESIAN_POINT('Ctrl Pts',(-22.058013816727,-66.0004830916995,25.9959252805377));
#14249=CARTESIAN_POINT('Ctrl Pts',(-22.0555312835971,-66.0018063313406,
26.7540747194623));
#14250=CARTESIAN_POINT('Ctrl Pts',(-22.0505008655215,-65.4537399884148,
26.7243225092112));
#14251=CARTESIAN_POINT('Ctrl Pts',(-21.5431051312739,-64.2150554479046,
26.6575259262963));
#14252=CARTESIAN_POINT('Ctrl Pts',(-19.4513023285576,-63.6341803621276,
26.5536849707175));
#14253=CARTESIAN_POINT('Ctrl Pts',(-17.7147940941022,-65.1778050096466,
26.4425518527259));
#14254=CARTESIAN_POINT('Ctrl Pts',(-18.0697955898292,-67.4739347707333,
26.3314187347343));
#14255=CARTESIAN_POINT('Ctrl Pts',(-20.1913974492333,-68.4210616212703,
26.2202856167428));
#14256=CARTESIAN_POINT('Ctrl Pts',(-21.8105645272037,-67.3656512612381,
26.1278376116521));
#14257=CARTESIAN_POINT('Ctrl Pts',(-22.0514896068728,-66.3399661110351,
26.0724339792253));
#14258=CARTESIAN_POINT('Ctrl Pts',(-22.0514168805361,-66.0000495912932,
26.0540747194623));
#14259=CARTESIAN_POINT('Origin',(-20.,-66.,37.5459252805377));
#14260=CARTESIAN_POINT('',(-22.0572927814363,-65.9988171297943,27.4540747194623));
#14261=CARTESIAN_POINT('',(-22.051608611075,-66.0006513925013,27.3959252805377));
#14262=CARTESIAN_POINT('',(-22.05475,-65.9999999999998,37.5459252805377));
#14263=CARTESIAN_POINT('Ctrl Pts',(-22.051608611075,-66.0006513925013,27.3959252805377));
#14264=CARTESIAN_POINT('Ctrl Pts',(-22.0505185829512,-65.6173024522387,
27.3752153462994));
#14265=CARTESIAN_POINT('Ctrl Pts',(-21.7633388641963,-64.5467312818546,
27.3174610393972));
#14266=CARTESIAN_POINT('Ctrl Pts',(-20.0378654071592,-63.5716800778574,
27.2226623598312));
#14267=CARTESIAN_POINT('Ctrl Pts',(-17.9804255504411,-64.6511150930585,
27.1115292418396));
#14268=CARTESIAN_POINT('Ctrl Pts',(-17.7713797576864,-66.9651026482916,
27.0003961238481));
#14269=CARTESIAN_POINT('Ctrl Pts',(-19.602054852468,-68.3957903104112,26.8892630058565));
#14270=CARTESIAN_POINT('Ctrl Pts',(-21.6064981577545,-67.699876740124,26.787772724753));
#14271=CARTESIAN_POINT('Ctrl Pts',(-22.0497193665927,-66.5037217839924,
26.7233268163134));
#14272=CARTESIAN_POINT('Ctrl Pts',(-22.0542237095723,-65.9981345160623,
26.6959252805377));
#14273=CARTESIAN_POINT('Ctrl Pts',(-22.0572927814363,-65.9988171297943,
27.4540747194623));
#14274=CARTESIAN_POINT('Ctrl Pts',(-22.0577689751881,-65.9294336866987,
27.4502997845249));
#14275=CARTESIAN_POINT('Ctrl Pts',(-22.0231033120199,-65.1796547626522,
27.4094804769235));
#14276=CARTESIAN_POINT('Ctrl Pts',(-21.1033854005481,-63.836504637639,27.3316167966584));
#14277=CARTESIAN_POINT('Ctrl Pts',(-18.7808305074767,-63.8995721204905,
27.2204836786668));
#14278=CARTESIAN_POINT('Ctrl Pts',(-17.5741075252728,-65.8850338715259,
27.1093505606753));
#14279=CARTESIAN_POINT('Ctrl Pts',(-18.5876568076359,-67.9757171467262,
26.9982174426837));
#14280=CARTESIAN_POINT('Ctrl Pts',(-20.8938381898737,-68.2581463290383,
26.8870843246921));
#14281=CARTESIAN_POINT('Ctrl Pts',(-21.98355270846,-66.951522387647,26.8057034169517));
#14282=CARTESIAN_POINT('Ctrl Pts',(-22.0567642214294,-66.1361354703139,
26.7613668818751));
#14283=CARTESIAN_POINT('Ctrl Pts',(-22.0555312835971,-66.0018063313406,
26.7540747194623));
#14284=CARTESIAN_POINT('Origin',(-20.,-66.,37.5459252805377));
#14285=CARTESIAN_POINT('',(-22.0519547460626,-65.9989448751757,28.1540747194623));
#14286=CARTESIAN_POINT('',(-22.0566098665172,-66.0015207492701,28.0959252805377));
#14287=CARTESIAN_POINT('',(-22.05475,-65.9999999999998,37.5459252805377));
#14288=CARTESIAN_POINT('Ctrl Pts',(-22.0566098665172,-66.0015207492701,
28.0959252805377));
#14289=CARTESIAN_POINT('Ctrl Pts',(-22.0517667328726,-65.4169498621218,
28.0641482489492));
#14290=CARTESIAN_POINT('Ctrl Pts',(-21.4848825853714,-64.1426999769185,
27.9953268446968));
#14291=CARTESIAN_POINT('Ctrl Pts',(-19.3231871724393,-63.667598701565,27.8894610677806));
#14292=CARTESIAN_POINT('Ctrl Pts',(-17.6733825603793,-65.3035642809691,
27.778327949789));
#14293=CARTESIAN_POINT('Ctrl Pts',(-18.152989804436,-67.5769352415803,27.6671948317974));
#14294=CARTESIAN_POINT('Ctrl Pts',(-20.3230534758781,-68.4070330021147,
27.5560617138059));
#14295=CARTESIAN_POINT('Ctrl Pts',(-21.8481481825977,-67.2899652950944,
27.4656385300526));
#14296=CARTESIAN_POINT('Ctrl Pts',(-22.0524683432725,-66.3030082029172,
27.4122597189632));
#14297=CARTESIAN_POINT('Ctrl Pts',(-22.051608611075,-66.0006513925013,27.3959252805377));
#14298=CARTESIAN_POINT('Ctrl Pts',(-22.0519547460626,-65.9989448751757,
28.1540747194623));
#14299=CARTESIAN_POINT('Ctrl Pts',(-22.0532325567715,-65.7243289273863,
28.1392326871747));
#14300=CARTESIAN_POINT('Ctrl Pts',(-21.8740722613233,-64.7658952750654,
28.0873462822231));
#14301=CARTESIAN_POINT('Ctrl Pts',(-20.4194990521396,-63.6078896201836,
27.9984155046077));
#14302=CARTESIAN_POINT('Ctrl Pts',(-18.2178369745624,-64.3501313764944,
27.8872823866162));
#14303=CARTESIAN_POINT('Ctrl Pts',(-17.6472806432027,-66.6023978352466,
27.7761492686246));
#14304=CARTESIAN_POINT('Ctrl Pts',(-19.2300256691482,-68.3033260850074,
27.665016150633));
#14305=CARTESIAN_POINT('Ctrl Pts',(-21.439781925539,-67.909990145913,27.557657967579));
#14306=CARTESIAN_POINT('Ctrl Pts',(-22.053095967814,-66.6103106197642,27.4873441571887));
#14307=CARTESIAN_POINT('Ctrl Pts',(-22.0572927814363,-65.9988171297943,
27.4540747194623));
#14308=CARTESIAN_POINT('Origin',(-20.,-66.,37.5459252805377));
#14309=CARTESIAN_POINT('',(-22.0534438287596,-66.0017537139889,28.8540747194623));
#14310=CARTESIAN_POINT('',(-22.0563386042488,-65.9983838584325,28.7959252805377));
#14311=CARTESIAN_POINT('',(-22.05475,-65.9999999999998,37.5459252805377));
#14312=CARTESIAN_POINT('Ctrl Pts',(-22.0563386042488,-65.9983838584325,
28.7959252805377));
#14313=CARTESIAN_POINT('Ctrl Pts',(-22.0572597478083,-65.8916548104596,
28.7901255242628));
#14314=CARTESIAN_POINT('Ctrl Pts',(-22.001175176898,-65.1041931970662,28.747281395324));
#14315=CARTESIAN_POINT('Ctrl Pts',(-20.9838411260118,-63.7795883131318,
28.6673928937215));
#14316=CARTESIAN_POINT('Ctrl Pts',(-18.6681747606656,-63.9691349251399,
28.5562597757299));
#14317=CARTESIAN_POINT('Ctrl Pts',(-17.5714472744839,-66.0174091877327,
28.4451266577383));
#14318=CARTESIAN_POINT('Ctrl Pts',(-18.6974268296081,-68.0497498764889,
28.3339935397468));
#14319=CARTESIAN_POINT('Ctrl Pts',(-21.0155726190361,-68.2060788009229,
28.2228604217552));
#14320=CARTESIAN_POINT('Ctrl Pts',(-22.0071593704442,-66.8759492827429,
28.1435043353522));
#14321=CARTESIAN_POINT('Ctrl Pts',(-22.0574126613506,-66.0984188574757,
28.101192621613));
#14322=CARTESIAN_POINT('Ctrl Pts',(-22.0566098665172,-66.0015207492701,
28.0959252805377));
#14323=CARTESIAN_POINT('Ctrl Pts',(-22.0534438287596,-66.0017537139889,
28.8540747194623));
#14324=CARTESIAN_POINT('Ctrl Pts',(-22.0495560850897,-65.5232420578776,
28.8281655898244));
#14325=CARTESIAN_POINT('Ctrl Pts',(-21.644456045474,-64.3546300343245,28.7652120875227));
#14326=CARTESIAN_POINT('Ctrl Pts',(-19.6986309083236,-63.5901559812818,
28.6652142125571));
#14327=CARTESIAN_POINT('Ctrl Pts',(-17.8119536633046,-64.9461381720334,
28.5540810945656));
#14328=CARTESIAN_POINT('Ctrl Pts',(-17.9278625462951,-67.2666561873374,
28.4429479765739));
#14329=CARTESIAN_POINT('Ctrl Pts',(-19.9402731854491,-68.4278806048883,
28.3318148585824));
#14330=CARTESIAN_POINT('Ctrl Pts',(-21.7312864923139,-67.5086939343413,
28.2355237728785));
#14331=CARTESIAN_POINT('Ctrl Pts',(-22.0500432566018,-66.4097455409721,
28.1762770598385));
#14332=CARTESIAN_POINT('Ctrl Pts',(-22.0519547460626,-65.9989448751757,
28.1540747194623));
#14333=CARTESIAN_POINT('Origin',(-20.,-66.,37.5459252805377));
#14334=CARTESIAN_POINT('',(-22.05815424133,-66.0000233771342,29.5540747194623));
#14335=CARTESIAN_POINT('',(-22.0515262960928,-65.9995028191493,29.4959252805377));
#14336=CARTESIAN_POINT('',(-22.05475,-65.9999999999998,37.5459252805377));
#14337=CARTESIAN_POINT('Ctrl Pts',(-22.0515262960928,-65.9995028191493,
29.4959252805377));
#14338=CARTESIAN_POINT('Ctrl Pts',(-22.0522023450635,-65.6872595186681,
29.4790584269126));
#14339=CARTESIAN_POINT('Ctrl Pts',(-21.8385380384052,-64.6901194966521,
29.4251472006236));
#14340=CARTESIAN_POINT('Ctrl Pts',(-20.2885122041186,-63.5885829625528,
29.3341916016708));
#14341=CARTESIAN_POINT('Ctrl Pts',(-18.1305721243274,-64.4497062091094,
29.2230584836793));
#14342=CARTESIAN_POINT('Ctrl Pts',(-17.6836060163159,-66.729719352058,29.1119253656877));
#14343=CARTESIAN_POINT('Ctrl Pts',(-19.3566948545509,-68.3418646225293,
29.0007922476961));
#14344=CARTESIAN_POINT('Ctrl Pts',(-21.5005207642192,-67.8383663168731,
28.8954588859795));
#14345=CARTESIAN_POINT('Ctrl Pts',(-22.0513761927624,-66.5733577027495,
28.8271698969266));
#14346=CARTESIAN_POINT('Ctrl Pts',(-22.0563386042488,-65.9983838584325,
28.7959252805377));
#14347=CARTESIAN_POINT('Ctrl Pts',(-22.0581541126866,-66.0000233762508,
29.5540747194623));
#14348=CARTESIAN_POINT('Ctrl Pts',(-22.0580399559099,-65.3211542304274,
29.5170984924742));
#14349=CARTESIAN_POINT('Ctrl Pts',(-21.3195544042373,-63.961952016278,29.4430778928223));
#14350=CARTESIAN_POINT('Ctrl Pts',(-19.004330572597,-63.784867065997,29.3320129205064));
#14351=CARTESIAN_POINT('Ctrl Pts',(-17.5989620477711,-65.6350503104176,
29.2208798025149));
#14352=CARTESIAN_POINT('Ctrl Pts',(-18.391117960758,-67.8192498750237,29.1097466845233));
#14353=CARTESIAN_POINT('Ctrl Pts',(-20.6557860410391,-68.3384003490309,
28.9986135665318));
#14354=CARTESIAN_POINT('Ctrl Pts',(-21.9322057879489,-67.0952788496883,
28.9133895781781));
#14355=CARTESIAN_POINT('Ctrl Pts',(-22.0551147058285,-66.2074087728823,
28.8652099624883));
#14356=CARTESIAN_POINT('Ctrl Pts',(-22.0534438287596,-66.0017537139889,
28.8540747194623));
#14357=CARTESIAN_POINT('Origin',(-20.,-66.,37.5459252805377));
#14358=CARTESIAN_POINT('',(-22.0535119803991,-65.9982315275897,30.2540747194623));
#14359=CARTESIAN_POINT('',(-22.0545158025659,-66.0018778868973,30.1959252805377));
#14360=CARTESIAN_POINT('',(-22.05475,-65.9999999999998,37.5459252805377));
#14361=CARTESIAN_POINT('Ctrl Pts',(-22.0545158025659,-66.0018778868973,
30.1959252805377));
#14362=CARTESIAN_POINT('Ctrl Pts',(-22.0498372217949,-65.4866536673289,
30.1679913295624));
#14363=CARTESIAN_POINT('Ctrl Pts',(-21.5925294629705,-64.2807662177915,
30.1030130059232));
#14364=CARTESIAN_POINT('Ctrl Pts',(-19.5677488993405,-63.6101610082697,
30.0009903096201));
#14365=CARTESIAN_POINT('Ctrl Pts',(-17.7577727222585,-65.0669468100008,
29.8898571916286));
#14366=CARTESIAN_POINT('Ctrl Pts',(-17.9999712029712,-67.3776996158348,
29.7787240736371));
#14367=CARTESIAN_POINT('Ctrl Pts',(-20.072674759091,-68.4275275075284,29.6675909556455));
#14368=CARTESIAN_POINT('Ctrl Pts',(-21.7743809927857,-67.4334540389223,
29.573324691279));
#14369=CARTESIAN_POINT('Ctrl Pts',(-22.0507175506515,-66.3730339637372,
29.5161027995764));
#14370=CARTESIAN_POINT('Ctrl Pts',(-22.0515262960928,-65.9995028191493,
29.4959252805377));
#14371=CARTESIAN_POINT('Ctrl Pts',(-22.0535119803991,-65.9982315275897,
30.2540747194623));
#14372=CARTESIAN_POINT('Ctrl Pts',(-22.0551803333329,-65.7951106704412,
30.2430757677879));
#14373=CARTESIAN_POINT('Ctrl Pts',(-21.9341785310365,-64.9098242979182,
30.1950324434496));
#14374=CARTESIAN_POINT('Ctrl Pts',(-20.6643636396598,-63.6640221580101,
30.1099447464473));
#14375=CARTESIAN_POINT('Ctrl Pts',(-18.3978055097405,-64.1748577207922,
29.9988116284558));
#14376=CARTESIAN_POINT('Ctrl Pts',(-17.5976388390673,-66.3561353344053,
29.8876785104642));
#14377=CARTESIAN_POINT('Ctrl Pts',(-18.9962076588936,-68.2114638726205,
29.7765453924727));
#14378=CARTESIAN_POINT('Ctrl Pts',(-21.313486738182,-68.0427736322436,29.6654122744811));
#14379=CARTESIAN_POINT('Ctrl Pts',(-22.0575867329659,-66.6826457097529,
29.5912553834776));
#14380=CARTESIAN_POINT('Ctrl Pts',(-22.0581543230729,-66.0012745043528,
29.554142865138));
#14381=CARTESIAN_POINT('Ctrl Pts',(-22.0581541126866,-66.0000233762508,
29.5540747194623));
#14382=CARTESIAN_POINT('Origin',(-20.,-66.,37.5459252805377));
#14383=CARTESIAN_POINT('',(-22.0519163324186,-66.0010204152869,30.9540747194623));
#14384=CARTESIAN_POINT('',(-22.0579001363803,-65.9993455608086,30.8959252805377));
#14385=CARTESIAN_POINT('',(-22.05475,-65.9999999999998,37.5459252805377));
#14386=CARTESIAN_POINT('Ctrl Pts',(-22.0579001363803,-65.9993455608086,
30.8959252805377));
#14387=CARTESIAN_POINT('Ctrl Pts',(-22.058049932207,-65.9634098788375,30.893968604876));
#14388=CARTESIAN_POINT('Ctrl Pts',(-22.0409122080377,-65.2472748593686,
30.8549675565505));
#14389=CARTESIAN_POINT('Ctrl Pts',(-21.207949773882,-63.8930997260919,30.778922135561));
#14390=CARTESIAN_POINT('Ctrl Pts',(-18.8850915735795,-63.8424201935705,
30.6677890175695));
#14391=CARTESIAN_POINT('Ctrl Pts',(-17.582641447505,-65.766442621407,30.556655899578));
#14392=CARTESIAN_POINT('Ctrl Pts',(-18.4926530149794,-67.9042259548608,
30.4455227815864));
#14393=CARTESIAN_POINT('Ctrl Pts',(-20.7822478717438,-68.2991867448226,
30.3343896635948));
#14394=CARTESIAN_POINT('Ctrl Pts',(-21.9603524673483,-67.0194951717011,
30.2511904965786));
#14395=CARTESIAN_POINT('Ctrl Pts',(-22.0560416820867,-66.1699139054527,
30.2050357022262));
#14396=CARTESIAN_POINT('Ctrl Pts',(-22.0545158025659,-66.0018778868973,
30.1959252805377));
#14397=CARTESIAN_POINT('Ctrl Pts',(-22.0519163324186,-66.0010204152869,
30.9540747194623));
#14398=CARTESIAN_POINT('Ctrl Pts',(-22.0500811038091,-65.5927223619752,
30.9320086704376));
#14399=CARTESIAN_POINT('Ctrl Pts',(-21.7342815688762,-64.4963597903545,
30.8728982487491));
#14400=CARTESIAN_POINT('Ctrl Pts',(-19.9491839985917,-63.5719165463332,
30.7767434543967));
#14401=CARTESIAN_POINT('Ctrl Pts',(-17.9325251760105,-64.7257475226081,
30.6656103364052));
#14402=CARTESIAN_POINT('Ctrl Pts',(-17.8081006873606,-67.0458245202808,
30.5544772184136));
#14403=CARTESIAN_POINT('Ctrl Pts',(-19.6897887219546,-68.4087217537406,
30.443344100422));
#14404=CARTESIAN_POINT('Ctrl Pts',(-21.6410622563722,-67.6503619047499,
30.3432099341049));
#14405=CARTESIAN_POINT('Ctrl Pts',(-22.0495613353008,-66.4792199338248,
30.2801201404517));
#14406=CARTESIAN_POINT('Ctrl Pts',(-22.0535119803991,-65.9982315275897,
30.2540747194623));
#14407=CARTESIAN_POINT('Origin',(-20.,-66.,37.5459252805377));
#14408=CARTESIAN_POINT('',(-22.0572361971601,-66.0012177327075,31.6540747194623));
#14409=CARTESIAN_POINT('',(-22.0525866916182,-65.9985364755553,31.5959252805377));
#14410=CARTESIAN_POINT('',(-22.05475,-65.9999999999998,37.5459252805377));
#14411=CARTESIAN_POINT('Ctrl Pts',(-22.0525866916182,-65.9985364755553,
31.5959252805377));
#14412=CARTESIAN_POINT('Ctrl Pts',(-22.0541717763817,-65.7577490902302,
31.5829015075258));
#14413=CARTESIAN_POINT('Ctrl Pts',(-21.9036809516229,-64.8339923497498,
31.53283336185));
#14414=CARTESIAN_POINT('Ctrl Pts',(-20.5360719702046,-63.63128763604,31.4457208435104));
#14415=CARTESIAN_POINT('Ctrl Pts',(-18.3007212782933,-64.2648852353891,
31.3345877255189));
#14416=CARTESIAN_POINT('Ctrl Pts',(-17.6206173554466,-66.4865281607617,
31.2234546075273));
#14417=CARTESIAN_POINT('Ctrl Pts',(-19.1182180804836,-68.2628813638435,
31.1123214895358));
#14418=CARTESIAN_POINT('Ctrl Pts',(-21.3822834251028,-67.9733455779535,
31.0031450472058));
#14419=CARTESIAN_POINT('Ctrl Pts',(-22.0552139525217,-66.6437550279776,
30.9310129775398));
#14420=CARTESIAN_POINT('Ctrl Pts',(-22.0579001363803,-65.9993455608086,
30.8959252805377));
#14421=CARTESIAN_POINT('Ctrl Pts',(-22.0572361971601,-66.0012177327075,
31.6540747194623));
#14422=CARTESIAN_POINT('Ctrl Pts',(-22.0529597533631,-65.3921852245915,
31.6209415730874));
#14423=CARTESIAN_POINT('Ctrl Pts',(-21.4439785259947,-64.0947971370138,
31.5507640540487));
#14424=CARTESIAN_POINT('Ctrl Pts',(-19.2384841459624,-63.6938635929289,
31.4435421623461));
#14425=CARTESIAN_POINT('Ctrl Pts',(-17.6495073099557,-65.3889716553072,
31.3324090443545));
#14426=CARTESIAN_POINT('Ctrl Pts',(-18.2117938983683,-67.6433169085898,
31.221275926363));
#14427=CARTESIAN_POINT('Ctrl Pts',(-20.4107170941006,-68.3936338468077,
31.1101428083714));
#14428=CARTESIAN_POINT('Ctrl Pts',(-21.8717661429505,-67.239207813012,31.0210757394045));
#14429=CARTESIAN_POINT('Ctrl Pts',(-22.0531620764135,-66.2781710903763,
30.9690530431015));
#14430=CARTESIAN_POINT('Ctrl Pts',(-22.0519163324186,-66.0010204152869,
30.9540747194623));
#14431=CARTESIAN_POINT('Origin',(-20.,-66.,37.5459252805377));
#14432=CARTESIAN_POINT('',(-22.0556069266979,-65.9982061756783,32.3540747194623));
#14433=CARTESIAN_POINT('',(-22.0526152608938,-66.0014769892548,32.2959252805377));
#14434=CARTESIAN_POINT('',(-22.05475,-65.9999999999998,37.5459252805377));
#14435=CARTESIAN_POINT('Ctrl Pts',(-22.0526152608939,-66.0014769892548,
32.2959252805377));
#14436=CARTESIAN_POINT('Ctrl Pts',(-22.049653606289,-65.5560934056117,32.2718344101756));
#14437=CARTESIAN_POINT('Ctrl Pts',(-21.6883555136058,-64.4214701158507,
32.2106991671496));
#14438=CARTESIAN_POINT('Ctrl Pts',(-19.8169356466133,-63.578294224532,32.1125195514598));
#14439=CARTESIAN_POINT('Ctrl Pts',(-17.8661543709335,-64.8403128647219,
32.0013864334682));
#14440=CARTESIAN_POINT('Ctrl Pts',(-17.8683526023209,-67.163722815959,31.8902533154767));
#14441=CARTESIAN_POINT('Ctrl Pts',(-19.8215184328882,-68.4220478423468,
31.7791201974851));
#14442=CARTESIAN_POINT('Ctrl Pts',(-21.690001156166,-67.5759383023312,31.6810108525055));
#14443=CARTESIAN_POINT('Ctrl Pts',(-22.0496632157189,-66.4426364593967,
31.6199458801897));
#14444=CARTESIAN_POINT('Ctrl Pts',(-22.0525866916182,-65.9985364755553,
31.5959252805377));
#14445=CARTESIAN_POINT('Ctrl Pts',(-22.0556069266979,-65.9982061756783,
32.3540747194623));
#14446=CARTESIAN_POINT('Ctrl Pts',(-22.0568133671517,-65.8664001586089,
32.3469188484011));
#14447=CARTESIAN_POINT('Ctrl Pts',(-21.9852145475282,-65.0535687993885,
32.302718604676));
#14448=CARTESIAN_POINT('Ctrl Pts',(-20.9021196384422,-63.7451492994194,
32.221473988287));
#14449=CARTESIAN_POINT('Ctrl Pts',(-18.594917279486,-64.0191128067246,32.1103408702954));
#14450=CARTESIAN_POINT('Ctrl Pts',(-17.5737019298616,-66.106062240275,31.9992077523039));
#14451=CARTESIAN_POINT('Ctrl Pts',(-18.7731300721891,-68.0959393369569,
31.8880746343123));
#14452=CARTESIAN_POINT('Ctrl Pts',(-21.095437861579,-68.1675302570873,31.7769415163208));
#14453=CARTESIAN_POINT('Ctrl Pts',(-22.0216974673029,-66.8254194714185,
31.6989415447041));
#14454=CARTESIAN_POINT('Ctrl Pts',(-22.057741013069,-66.0731114167429,31.6579859457513));
#14455=CARTESIAN_POINT('Ctrl Pts',(-22.0572361971601,-66.0012177327075,
31.6540747194623));
#14456=CARTESIAN_POINT('Origin',(-20.,-66.,37.5459252805377));
#14457=CARTESIAN_POINT('',(-22.0514188637225,-65.9999091152567,33.0540747194623));
#14458=CARTESIAN_POINT('',(-22.0579172481639,-66.0006320364424,32.9959252805377));
#14459=CARTESIAN_POINT('',(-22.05475,-65.9999999999998,37.5459252805377));
#14460=CARTESIAN_POINT('Ctrl Pts',(-22.0579172481639,-66.0006320364424,
32.9959252805377));
#14461=CARTESIAN_POINT('Ctrl Pts',(-22.055307383354,-65.3549463154049,32.9607673128254));
#14462=CARTESIAN_POINT('Ctrl Pts',(-21.3800044998465,-64.0242259372538,
32.8885649724492));
#14463=CARTESIAN_POINT('Ctrl Pts',(-19.1139377351588,-63.7387912340402,
32.7793182594091));
#14464=CARTESIAN_POINT('Ctrl Pts',(-17.6197009851889,-65.5179750831086,
32.6681851414176));
#14465=CARTESIAN_POINT('Ctrl Pts',(-18.3040075812308,-67.7383271084264,
32.557052023426));
#14466=CARTESIAN_POINT('Ctrl Pts',(-20.5405531925411,-68.3676937442268,
32.4459189054345));
#14467=CARTESIAN_POINT('Ctrl Pts',(-21.9047825486759,-67.1633756004897,
32.358876657805));
#14468=CARTESIAN_POINT('Ctrl Pts',(-22.0542077230658,-66.2409568083382,
32.3088787828394));
#14469=CARTESIAN_POINT('Ctrl Pts',(-22.0526152608939,-66.0014769892548,
32.2959252805377));
#14470=CARTESIAN_POINT('Ctrl Pts',(-22.0514188637225,-65.9999091152567,
33.0540747194623));
#14471=CARTESIAN_POINT('Ctrl Pts',(-22.0515519905893,-65.6625169941898,
33.0358517510508));
#14472=CARTESIAN_POINT('Ctrl Pts',(-21.8131840852274,-64.6394379208522,
32.9805844099755));
#14473=CARTESIAN_POINT('Ctrl Pts',(-20.2002808122731,-63.5796572308245,
32.8882726962363));
#14474=CARTESIAN_POINT('Ctrl Pts',(-18.0752183512995,-64.5189911786904,
32.7771395782448));
#14475=CARTESIAN_POINT('Ctrl Pts',(-17.7117918139106,-66.8138026917249,
32.6660064602532));
#14476=CARTESIAN_POINT('Ctrl Pts',(-19.442623471414,-68.3637899503476,32.5548733422617));
#14477=CARTESIAN_POINT('Ctrl Pts',(-21.5392921623106,-67.789843471444,32.4508960953313));
#14478=CARTESIAN_POINT('Ctrl Pts',(-22.0505678899225,-66.5487309571744,
32.3839632210649));
#14479=CARTESIAN_POINT('Ctrl Pts',(-22.0556069266979,-65.9982061756783,
32.3540747194623));
#14480=CARTESIAN_POINT('Origin',(-20.,-66.,37.5459252805377));
#14481=CARTESIAN_POINT('',(-22.0552733614683,-66.0018413365206,33.7540747194623));
#14482=CARTESIAN_POINT('',(-22.0544769775149,-65.99812289348,33.6959252805377));
#14483=CARTESIAN_POINT('',(-22.05475,-65.9999999999998,37.5459252805377));
#14484=CARTESIAN_POINT('Ctrl Pts',(-22.0544769775149,-65.99812289348,33.6959252805377));
#14485=CARTESIAN_POINT('Ctrl Pts',(-22.0560114585337,-65.8287826123771,
33.686744588139));
#14486=CARTESIAN_POINT('Ctrl Pts',(-21.9594169044098,-64.9778761409694,
33.6405195230764));
#14487=CARTESIAN_POINT('Ctrl Pts',(-20.7778958486438,-63.6993371678323,
33.5572500853501));
#14488=CARTESIAN_POINT('Ctrl Pts',(-18.4890524532058,-64.0986297225616,
33.4461169673585));
#14489=CARTESIAN_POINT('Ctrl Pts',(-17.5830877228631,-66.2381311930787,
33.334983849367));
#14490=CARTESIAN_POINT('Ctrl Pts',(-18.8891762373197,-68.159685622601,33.2238507313753));
#14491=CARTESIAN_POINT('Ctrl Pts',(-21.2119343809668,-68.1046107660899,
33.1127176133838));
#14492=CARTESIAN_POINT('Ctrl Pts',(-22.0415655539315,-66.7501146853756,
33.0367424631046));
#14493=CARTESIAN_POINT('Ctrl Pts',(-22.0580572807716,-66.0352763808272,
32.9978116854892));
#14494=CARTESIAN_POINT('Ctrl Pts',(-22.0579172481639,-66.0006320364424,
32.9959252805377));
#14495=CARTESIAN_POINT('Ctrl Pts',(-22.0552733614683,-66.0018413365206,
33.7540747194623));
#14496=CARTESIAN_POINT('Ctrl Pts',(-22.0502920767718,-65.4621140092977,
33.7247846537006));
#14497=CARTESIAN_POINT('Ctrl Pts',(-21.5559212661831,-64.2316956472682,
33.6584502152751));
#14498=CARTESIAN_POINT('Ctrl Pts',(-19.4807858227571,-63.6275354235162,
33.5550714041857));
#14499=CARTESIAN_POINT('Ctrl Pts',(-17.7252024818967,-65.1494309100778,
33.4439382861942));
#14500=CARTESIAN_POINT('Ctrl Pts',(-18.0516033664323,-67.4498007037218,
33.3328051682026));
#14501=CARTESIAN_POINT('Ctrl Pts',(-20.1612535373157,-68.4232558307668,
33.221672050211));
#14502=CARTESIAN_POINT('Ctrl Pts',(-21.8015900775427,-67.3829020390902,
33.1287619006309));
#14503=CARTESIAN_POINT('Ctrl Pts',(-22.0512813650165,-66.3483810743131,
33.0728961237147));
#14504=CARTESIAN_POINT('Ctrl Pts',(-22.0514188637225,-65.9999091152567,
33.0540747194623));
#14505=CARTESIAN_POINT('Origin',(-20.,-66.,37.5459252805377));
#14506=CARTESIAN_POINT('',(-22.0574743887429,-65.9989407171765,34.4540747194623));
#14507=CARTESIAN_POINT('',(-22.0515358806555,-66.000517785455,34.3959252805377));
#14508=CARTESIAN_POINT('',(-22.05475,-65.9999999999998,37.5459252805377));
#14509=CARTESIAN_POINT('Ctrl Pts',(-22.0515358806555,-66.000517785455,34.3959252805377));
#14510=CARTESIAN_POINT('Ctrl Pts',(-22.050690498549,-65.6256901339794,34.3756774907888));
#14511=CARTESIAN_POINT('Ctrl Pts',(-21.7729353091241,-64.5639295587311,
34.318385328376));
#14512=CARTESIAN_POINT('Ctrl Pts',(-20.0680811526701,-63.5723393435572,
34.2240487932995));
#14513=CARTESIAN_POINT('Ctrl Pts',(-17.9973678404257,-64.6260873816269,
34.1129156753078));
#14514=CARTESIAN_POINT('Ctrl Pts',(-17.7595423005167,-66.9372943668669,
34.0017825573163));
#14515=CARTESIAN_POINT('Ctrl Pts',(-19.5722718322054,-68.3906526348572,
33.8906494393247));
#14516=CARTESIAN_POINT('Ctrl Pts',(-21.5943860795634,-67.7166817852802,
33.7886970137319));
#14517=CARTESIAN_POINT('Ctrl Pts',(-22.0498197810177,-66.5120757898144,
33.7237889608028));
#14518=CARTESIAN_POINT('Ctrl Pts',(-22.0544769775149,-65.99812289348,33.6959252805377));
#14519=CARTESIAN_POINT('Ctrl Pts',(-22.0574743887429,-65.9989407171765,
34.4540747194623));
#14520=CARTESIAN_POINT('Ctrl Pts',(-22.0578567862954,-65.9380656581726,
34.4507619290143));
#14521=CARTESIAN_POINT('Ctrl Pts',(-22.0277962110148,-65.1968548676797,
34.4104047659024));
#14522=CARTESIAN_POINT('Ctrl Pts',(-21.1302229793561,-63.8504031421106,
34.3330032301266));
#14523=CARTESIAN_POINT('Ctrl Pts',(-18.8070632766386,-63.8845630078765,
34.221870112135));
#14524=CARTESIAN_POINT('Ctrl Pts',(-17.5757260074789,-65.8548543331223,
34.1107369941435));
#14525=CARTESIAN_POINT('Ctrl Pts',(-18.5631798196893,-67.9579885544186,
33.9996038761519));
#14526=CARTESIAN_POINT('Ctrl Pts',(-20.8656679609891,-68.2690946508119,
33.8884707581604));
#14527=CARTESIAN_POINT('Ctrl Pts',(-21.977838232828,-66.968790137621,33.8066277059305));
#14528=CARTESIAN_POINT('Ctrl Pts',(-22.0565921161143,-66.1447297606308,
33.7618290263645));
#14529=CARTESIAN_POINT('Ctrl Pts',(-22.0552733614683,-66.0018413365206,
33.7540747194623));
#14530=CARTESIAN_POINT('Origin',(-20.,-66.,37.5459252805377));
#14531=CARTESIAN_POINT('',(-22.0520911128174,-65.9988355264336,35.1540747194623));
#14532=CARTESIAN_POINT('',(-22.0563749241962,-66.0016062120012,35.0959252805377));
#14533=CARTESIAN_POINT('',(-22.05475,-65.9999999999998,37.5459252805377));
#14534=CARTESIAN_POINT('Ctrl Pts',(-22.0563749241962,-66.0016062120012,
35.0959252805377));
#14535=CARTESIAN_POINT('Ctrl Pts',(-22.0514251626832,-65.4253659758576,
35.0646103934386));
#14536=CARTESIAN_POINT('Ctrl Pts',(-21.4984704660108,-64.1591280998276,
34.9962511336756));
#14537=CARTESIAN_POINT('Ctrl Pts',(-19.3522645237931,-63.6593583355034,
34.8908475012488));
#14538=CARTESIAN_POINT('Ctrl Pts',(-17.6822294077865,-65.2746643974708,
34.7797143832572));
#14539=CARTESIAN_POINT('Ctrl Pts',(-18.1335089795993,-67.5538288003781,
34.6685812652656));
#14540=CARTESIAN_POINT('Ctrl Pts',(-20.2930746903084,-68.4108665986726,
34.5574481472741));
#14541=CARTESIAN_POINT('Ctrl Pts',(-21.8398174471696,-67.3072525302986,
34.4665628190314));
#14542=CARTESIAN_POINT('Ctrl Pts',(-22.0522371685899,-66.3114565992663,
34.4127218634526));
#14543=CARTESIAN_POINT('Ctrl Pts',(-22.0515358806555,-66.000517785455,34.3959252805377));
#14544=CARTESIAN_POINT('Ctrl Pts',(-22.0520911128174,-65.9988355264336,
35.1540747194623));
#14545=CARTESIAN_POINT('Ctrl Pts',(-22.0534711048112,-65.7328124009057,
35.1396948316641));
#14546=CARTESIAN_POINT('Ctrl Pts',(-21.8818113373711,-64.7831882718686,
35.088270571202));
#14547=CARTESIAN_POINT('Ctrl Pts',(-20.4492273324997,-63.61330436034,34.9998019380759));
#14548=CARTESIAN_POINT('Ctrl Pts',(-18.2385100652431,-64.3280768123671,
34.8886688200844));
#14549=CARTESIAN_POINT('Ctrl Pts',(-17.6399645748577,-66.5730756011264,
34.7775357020929));
#14550=CARTESIAN_POINT('Ctrl Pts',(-19.2014229874425,-68.2935648037488,
34.6664025841013));
#14551=CARTESIAN_POINT('Ctrl Pts',(-21.4254342373654,-67.9261851342807,
34.5585822565578));
#14552=CARTESIAN_POINT('Ctrl Pts',(-22.0535807303049,-66.618784347459,34.4878063016781));
#14553=CARTESIAN_POINT('Ctrl Pts',(-22.0574743887429,-65.9989407171765,
34.4540747194623));
#14554=CARTESIAN_POINT('Origin',(-20.,-66.,37.5459252805377));
#14555=CARTESIAN_POINT('',(-22.0526726878338,-66.0023207051531,35.8540747194623));
#14556=CARTESIAN_POINT('',(-22.0565720193282,-65.9985037223956,35.7959252805377));
#14557=CARTESIAN_POINT('',(-22.05475,-65.9999999999998,37.5459252805377));
#14558=CARTESIAN_POINT('',(-20.5301702171886,-67.9851743256717,36.));
#14559=CARTESIAN_POINT('Ctrl Pts',(-20.5301702171885,-67.9851743256717,
36.));
#14560=CARTESIAN_POINT('Ctrl Pts',(-21.190259562418,-67.8088876857537,35.9629556273362));
#14561=CARTESIAN_POINT('Ctrl Pts',(-21.9249294223933,-67.1127898537559,
35.9143138671569));
#14562=CARTESIAN_POINT('Ctrl Pts',(-22.0542897540197,-66.2165895473215,
35.8656721069777));
#14563=CARTESIAN_POINT('Ctrl Pts',(-22.0526726878338,-66.0023207051531,
35.8540747194623));
#14564=CARTESIAN_POINT('',(-19.4686890762993,-67.9887317545258,36.));
#14565=CARTESIAN_POINT('Origin',(-20.,-66.,36.));
#14566=CARTESIAN_POINT('Ctrl Pts',(-19.4686883835207,-67.9887339150381,
36.));
#14567=CARTESIAN_POINT('Ctrl Pts',(-20.1132089071786,-68.1600296783296,
35.9636818543909));
#14568=CARTESIAN_POINT('Ctrl Pts',(-21.4929690160207,-67.8407342776925,
35.8956569479035));
#14569=CARTESIAN_POINT('Ctrl Pts',(-22.0517191488996,-66.5816759129075,
35.8276320414161));
#14570=CARTESIAN_POINT('Ctrl Pts',(-22.0565720193282,-65.9985037223956,
35.7959252805377));
#14571=CARTESIAN_POINT('Origin',(20.,-66.,30.));
#14572=CARTESIAN_POINT('',(18.3313536394157,-66.0003916926001,25.7714803633902));
#14573=CARTESIAN_POINT('',(18.3334666271624,-65.9985218536523,25.5785196366098));
#14574=CARTESIAN_POINT('',(18.334,-66.,30.));
#14575=CARTESIAN_POINT('',(19.2300979593295,-67.4774325188554,25.));
#14576=CARTESIAN_POINT('Ctrl Pts',(18.3334666271624,-65.9985218536523,25.5785196366098));
#14577=CARTESIAN_POINT('Ctrl Pts',(18.3324169745748,-65.8847145132893,25.5709016210591));
#14578=CARTESIAN_POINT('Ctrl Pts',(18.3430836686143,-65.7711020898156,25.5632836055085));
#14579=CARTESIAN_POINT('Ctrl Pts',(18.3661914671125,-65.6600764989809,25.5556655899578));
#14580=CARTESIAN_POINT('Ctrl Pts',(18.478558512482,-65.1201887375622,25.5186212172939));
#14581=CARTESIAN_POINT('Ctrl Pts',(18.8851100097676,-64.6414696565181,25.4815768446301));
#14582=CARTESIAN_POINT('Ctrl Pts',(19.3995346321509,-64.4430321483538,25.4445324719662));
#14583=CARTESIAN_POINT('Ctrl Pts',(19.9139592545342,-64.2445946401895,25.4074880993024));
#14584=CARTESIAN_POINT('Ctrl Pts',(20.5362570020153,-64.326438704905,25.3704437266385));
#14585=CARTESIAN_POINT('Ctrl Pts',(20.9821827720363,-64.6510268476224,25.3333993539747));
#14586=CARTESIAN_POINT('Ctrl Pts',(21.4281085420573,-64.9756149903398,25.2963549813108));
#14587=CARTESIAN_POINT('Ctrl Pts',(21.6976623346182,-65.5429472110592,25.259310608647));
#14588=CARTESIAN_POINT('Ctrl Pts',(21.6664135658646,-66.0935811418539,25.2222662359831));
#14589=CARTESIAN_POINT('Ctrl Pts',(21.635164797111,-66.6442150726486,25.1852218633193));
#14590=CARTESIAN_POINT('Ctrl Pts',(21.3031134670429,-67.1781507135186,25.1481774906554));
#14591=CARTESIAN_POINT('Ctrl Pts',(20.8246618488694,-67.4504550129278,25.1111331179916));
#14592=CARTESIAN_POINT('Ctrl Pts',(20.3462102306959,-67.722759312337,25.0740887453277));
#14593=CARTESIAN_POINT('Ctrl Pts',(19.7213583244171,-67.7334322702853,25.0370443726639));
#14594=CARTESIAN_POINT('Ctrl Pts',(19.2300979593295,-67.4774325188554,25.));
#14595=CARTESIAN_POINT('',(18.6629739733599,-65.0009969633526,25.));
#14596=CARTESIAN_POINT('Origin',(20.,-66.,25.));
#14597=CARTESIAN_POINT('',(18.3354783848229,-66.0012211146297,25.0714803633902));
#14598=CARTESIAN_POINT('Ctrl Pts',(18.6629725546621,-65.0009957901906,25.));
#14599=CARTESIAN_POINT('Ctrl Pts',(18.4510073215875,-65.2854499389498,25.0238267877967));
#14600=CARTESIAN_POINT('Ctrl Pts',(18.3378311125484,-65.6440627071064,25.0476535755935));
#14601=CARTESIAN_POINT('Ctrl Pts',(18.3354783848229,-66.0012211146297,25.0714803633902));
#14602=CARTESIAN_POINT('',(18.334,-66.,24.));
#14603=CARTESIAN_POINT('',(18.334,-66.,30.));
#14604=CARTESIAN_POINT('Origin',(20.,-66.,24.));
#14605=CARTESIAN_POINT('Ctrl Pts',(18.3354783848229,-66.0012211146297,25.0714803633902));
#14606=CARTESIAN_POINT('Ctrl Pts',(18.3342449510884,-66.1884638727438,25.0839717212025));
#14607=CARTESIAN_POINT('Ctrl Pts',(18.363470829549,-66.3753069066835,25.0964630790149));
#14608=CARTESIAN_POINT('Ctrl Pts',(18.4248900596206,-66.5508551769228,25.1089544368272));
#14609=CARTESIAN_POINT('Ctrl Pts',(18.607034937838,-67.0714611543465,25.1459988094911));
#14610=CARTESIAN_POINT('Ctrl Pts',(19.0723133986938,-67.4927321215424,25.1830431821549));
#14611=CARTESIAN_POINT('Ctrl Pts',(19.6082884916208,-67.6221190201672,25.2200875548188));
#14612=CARTESIAN_POINT('Ctrl Pts',(20.1442635845478,-67.751505918792,25.2571319274826));
#14613=CARTESIAN_POINT('Ctrl Pts',(20.7509353095461,-67.5890087488456,25.2941763001465));
#14614=CARTESIAN_POINT('Ctrl Pts',(21.1504371531331,-67.2088726584111,25.3312206728103));
#14615=CARTESIAN_POINT('Ctrl Pts',(21.54993899672,-66.8287365679766,25.3682650454742));
#14616=CARTESIAN_POINT('Ctrl Pts',(21.7422709588957,-66.230961557054,25.405309418138));
#14617=CARTESIAN_POINT('Ctrl Pts',(21.6395392404303,-65.6891597889306,25.4423537908019));
#14618=CARTESIAN_POINT('Ctrl Pts',(21.5368075219649,-65.1473580208071,25.4793981634657));
#14619=CARTESIAN_POINT('Ctrl Pts',(21.1390121228584,-64.6615294954828,25.5164425361296));
#14620=CARTESIAN_POINT('Ctrl Pts',(20.6281313212479,-64.453969540756,25.5534869087934));
#14621=CARTESIAN_POINT('Ctrl Pts',(20.1172505196373,-64.2464095860292,25.5905312814573));
#14622=CARTESIAN_POINT('Ctrl Pts',(19.4932843155229,-64.3171182018999,25.6275756541212));
#14623=CARTESIAN_POINT('Ctrl Pts',(19.0418023782432,-64.6337524622506,25.664620026785));
#14624=CARTESIAN_POINT('Ctrl Pts',(18.6076787555033,-64.9382129529964,25.7002401389867));
#14625=CARTESIAN_POINT('Ctrl Pts',(18.3330312172753,-65.4700522046137,25.7358602511885));
#14626=CARTESIAN_POINT('Ctrl Pts',(18.3313536394157,-66.0003916926001,25.7714803633902));
#14627=CARTESIAN_POINT('Origin',(20.,-66.,30.));
#14628=CARTESIAN_POINT('',(18.3344266756531,-65.9984874576763,26.4714803633902));
#14629=CARTESIAN_POINT('',(18.3367026517093,-66.000040209255,26.2785196366098));
#14630=CARTESIAN_POINT('',(18.334,-66.,30.));
#14631=CARTESIAN_POINT('Ctrl Pts',(18.3367026517093,-66.000040209255,26.2785196366098));
#14632=CARTESIAN_POINT('Ctrl Pts',(18.3367626645399,-65.7195428345507,26.2598345237089));
#14633=CARTESIAN_POINT('Ctrl Pts',(18.4039333309142,-65.4390183287806,26.241149410808));
#14634=CARTESIAN_POINT('Ctrl Pts',(18.5380532069523,-65.1953424610818,26.2224642979072));
#14635=CARTESIAN_POINT('Ctrl Pts',(18.8039540177177,-64.7122402341857,26.1854199252433));
#14636=CARTESIAN_POINT('Ctrl Pts',(19.3330018695053,-64.3739733253295,26.1483755525794));
#14637=CARTESIAN_POINT('Ctrl Pts',(19.8830898278916,-64.3353399906558,26.1113311799156));
#14638=CARTESIAN_POINT('Ctrl Pts',(20.433177786278,-64.296706655982,26.0742868072517));
#14639=CARTESIAN_POINT('Ctrl Pts',(21.0043058512631,-64.5577068954906,26.0372424345879));
#14640=CARTESIAN_POINT('Ctrl Pts',(21.3351230048638,-64.9989005442132,26.000198061924));
#14641=CARTESIAN_POINT('Ctrl Pts',(21.6659401584645,-65.4400941929357,25.9631536892602));
#14642=CARTESIAN_POINT('Ctrl Pts',(21.7564464006808,-66.0614812508722,25.9261093165963));
#14643=CARTESIAN_POINT('Ctrl Pts',(21.5652075003073,-66.578705400814,25.8890649439325));
#14644=CARTESIAN_POINT('Ctrl Pts',(21.3739685999339,-67.0959295507558,25.8520205712686));
#14645=CARTESIAN_POINT('Ctrl Pts',(20.9009845569708,-67.508990792703,25.8149761986048));
#14646=CARTESIAN_POINT('Ctrl Pts',(20.3627356556273,-67.6288589318993,25.7779318259409));
#14647=CARTESIAN_POINT('Ctrl Pts',(19.8244867542837,-67.7487270710955,25.7408874532771));
#14648=CARTESIAN_POINT('Ctrl Pts',(19.2209729945597,-67.575402107541,25.7038430806132));
#14649=CARTESIAN_POINT('Ctrl Pts',(18.8283074114245,-67.188211404867,25.6667987079494));
#14650=CARTESIAN_POINT('Ctrl Pts',(18.5163918127925,-66.88064480113,25.6373723508362));
#14651=CARTESIAN_POINT('Ctrl Pts',(18.3375211544446,-66.4381291788607,25.607945993723));
#14652=CARTESIAN_POINT('Ctrl Pts',(18.3334666271624,-65.9985218536523,25.5785196366098));
#14653=CARTESIAN_POINT('Ctrl Pts',(18.3313536394157,-66.0003916926001,25.7714803633902));
#14654=CARTESIAN_POINT('Ctrl Pts',(18.331286561923,-66.0215971722449,25.7729046238523));
#14655=CARTESIAN_POINT('Ctrl Pts',(18.3316559029049,-66.0428002541,25.7743288843144));
#14656=CARTESIAN_POINT('Ctrl Pts',(18.3324689176524,-66.0639863067127,25.7757531447766));
#14657=CARTESIAN_POINT('Ctrl Pts',(18.3536150647863,-66.6150259859933,25.8127975174404));
#14658=CARTESIAN_POINT('Ctrl Pts',(18.674905029499,-67.1545454397239,25.8498418901043));
#14659=CARTESIAN_POINT('Ctrl Pts',(19.1493178612708,-67.4356536527718,25.8868862627681));
#14660=CARTESIAN_POINT('Ctrl Pts',(19.6237306930425,-67.7167618658197,25.923930635432));
#14661=CARTESIAN_POINT('Ctrl Pts',(20.2512663918733,-67.7394588381849,25.9609750080958));
#14662=CARTESIAN_POINT('Ctrl Pts',(20.7447484303696,-67.4933561307171,25.9980193807597));
#14663=CARTESIAN_POINT('Ctrl Pts',(21.2382304688658,-67.2472534232492,26.0350637534235));
#14664=CARTESIAN_POINT('Ctrl Pts',(21.5976588470276,-66.7323510359483,26.0721081260874));
#14665=CARTESIAN_POINT('Ctrl Pts',(21.6585539923065,-66.1842793662227,26.1091524987512));
#14666=CARTESIAN_POINT('Ctrl Pts',(21.7194491375853,-65.636207696497,26.1461968714151));
#14667=CARTESIAN_POINT('Ctrl Pts',(21.4818110499811,-65.0549667443465,26.1832412440789));
#14668=CARTESIAN_POINT('Ctrl Pts',(21.0543866287213,-64.7065433408633,26.2202856167428));
#14669=CARTESIAN_POINT('Ctrl Pts',(20.6269622074615,-64.3581199373801,26.2573299894066));
#14670=CARTESIAN_POINT('Ctrl Pts',(20.0097514525462,-64.2425140825642,26.2943743620705));
#14671=CARTESIAN_POINT('Ctrl Pts',(19.4852026366556,-64.4126295250552,26.3314187347344));
#14672=CARTESIAN_POINT('Ctrl Pts',(18.960653820765,-64.5827449675462,26.3684631073982));
#14673=CARTESIAN_POINT('Ctrl Pts',(18.5287669438991,-65.0385817073442,26.4055074800621));
#14674=CARTESIAN_POINT('Ctrl Pts',(18.3871816973018,-65.5715397639926,26.4425518527259));
#14675=CARTESIAN_POINT('Ctrl Pts',(18.3503263440991,-65.7102714319599,26.452194689614));
#14676=CARTESIAN_POINT('Ctrl Pts',(18.3331414559104,-65.8542287411456,26.4618375265021));
#14677=CARTESIAN_POINT('Ctrl Pts',(18.3344266756531,-65.9984874576763,26.4714803633902));
#14678=CARTESIAN_POINT('Origin',(20.,-66.,30.));
#14679=CARTESIAN_POINT('',(18.3365470086803,-66.0005281518116,27.1714803633902));
#14680=CARTESIAN_POINT('',(18.3333666774615,-66.0014645809704,26.9785196366098));
#14681=CARTESIAN_POINT('',(18.334,-66.,30.));
#14682=CARTESIAN_POINT('Ctrl Pts',(18.3333666774615,-66.0014645809704,26.9785196366098));
#14683=CARTESIAN_POINT('Ctrl Pts',(18.3374453613588,-65.5570901083669,26.9487674263587));
#14684=CARTESIAN_POINT('Ctrl Pts',(18.5206885203257,-65.1097460475429,26.9190152161076));
#14685=CARTESIAN_POINT('Ctrl Pts',(18.8387597416989,-64.8015503031277,26.8892630058565));
#14686=CARTESIAN_POINT('Ctrl Pts',(19.2347891041815,-64.4178168623791,26.8522186331927));
#14687=CARTESIAN_POINT('Ctrl Pts',(19.8398377304009,-64.2498002251426,26.8151742605288));
#14688=CARTESIAN_POINT('Ctrl Pts',(20.3770233944236,-64.374388121695,26.7781298878649));
#14689=CARTESIAN_POINT('Ctrl Pts',(20.9142090584462,-64.4989760182474,26.7410855152011));
#14690=CARTESIAN_POINT('Ctrl Pts',(21.3835317602721,-64.9161684485887,26.7040411425372));
#14691=CARTESIAN_POINT('Ctrl Pts',(21.5702203295955,-65.435049925312,26.6669967698734));
#14692=CARTESIAN_POINT('Ctrl Pts',(21.7569088989189,-65.9539314020353,26.6299523972095));
#14693=CARTESIAN_POINT('Ctrl Pts',(21.6609633357398,-66.5745019251406,26.5929080245457));
#14694=CARTESIAN_POINT('Ctrl Pts',(21.3262899503724,-67.0127762524406,26.5558636518818));
#14695=CARTESIAN_POINT('Ctrl Pts',(20.9916165650051,-67.4510505797406,26.518819279218));
#14696=CARTESIAN_POINT('Ctrl Pts',(20.4182153574495,-67.7070287112352,26.4817749065541));
#14697=CARTESIAN_POINT('Ctrl Pts',(19.8684865381395,-67.6635699328358,26.4447305338903));
#14698=CARTESIAN_POINT('Ctrl Pts',(19.3187577188295,-67.6201111544364,26.4076861612264));
#14699=CARTESIAN_POINT('Ctrl Pts',(18.7927012877651,-67.2772154661431,26.3706417885626));
#14700=CARTESIAN_POINT('Ctrl Pts',(18.5310499571044,-66.7917988495284,26.3335974158987));
#14701=CARTESIAN_POINT('Ctrl Pts',(18.4013750725946,-66.5512254744963,26.3152381561357));
#14702=CARTESIAN_POINT('Ctrl Pts',(18.3366436854535,-66.2756459383905,26.2968788963728));
#14703=CARTESIAN_POINT('Ctrl Pts',(18.3367026517093,-66.000040209255,26.2785196366098));
#14704=CARTESIAN_POINT('Ctrl Pts',(18.3344266756531,-65.9984874576763,26.4714803633902));
#14705=CARTESIAN_POINT('Ctrl Pts',(18.3380788161142,-66.4084197657567,26.498881899166));
#14706=CARTESIAN_POINT('Ctrl Pts',(18.4908762665155,-66.8207859249028,26.5262834349417));
#14707=CARTESIAN_POINT('Ctrl Pts',(18.7652754263391,-67.1225936158832,26.5536849707175));
#14708=CARTESIAN_POINT('Ctrl Pts',(19.1362380183026,-67.5306100376265,26.5907293433813));
#14709=CARTESIAN_POINT('Ctrl Pts',(19.7294468185584,-67.7365635076143,26.6277737160452));
#14710=CARTESIAN_POINT('Ctrl Pts',(20.2734377447371,-67.6462056352892,26.664818088709));
#14711=CARTESIAN_POINT('Ctrl Pts',(20.8174286709158,-67.5558477629641,26.7018624613729));
#14712=CARTESIAN_POINT('Ctrl Pts',(21.3122017230173,-67.1691785483262,26.7389068340367));
#14713=CARTESIAN_POINT('Ctrl Pts',(21.5313390460231,-66.6631454483979,26.7759512067006));
#14714=CARTESIAN_POINT('Ctrl Pts',(21.7504763690289,-66.1571123484697,26.8129955793644));
#14715=CARTESIAN_POINT('Ctrl Pts',(21.693977962939,-65.5317153632511,26.8500399520283));
#14716=CARTESIAN_POINT('Ctrl Pts',(21.3876985948801,-65.0731484534342,26.8870843246922));
#14717=CARTESIAN_POINT('Ctrl Pts',(21.0814192268212,-64.6145815436172,26.924128697356));
#14718=CARTESIAN_POINT('Ctrl Pts',(20.5253588967934,-64.322844709202,26.9611730700199));
#14719=CARTESIAN_POINT('Ctrl Pts',(19.9739817626904,-64.3314424706716,26.9982174426837));
#14720=CARTESIAN_POINT('Ctrl Pts',(19.4226046285874,-64.3400402321411,27.0352618153476));
#14721=CARTESIAN_POINT('Ctrl Pts',(18.8759106904092,-64.6489725894954,27.0723061880114));
#14722=CARTESIAN_POINT('Ctrl Pts',(18.5840778492301,-65.1168660144091,27.1093505606753));
#14723=CARTESIAN_POINT('Ctrl Pts',(18.4209265116641,-65.3784453411378,27.1300604949136));
#14724=CARTESIAN_POINT('Ctrl Pts',(18.3374308081207,-65.689707199922,27.1507704291519));
#14725=CARTESIAN_POINT('Ctrl Pts',(18.3365470086803,-66.0005281518116,27.1714803633902));
#14726=CARTESIAN_POINT('Origin',(20.,-66.,30.));
#14727=CARTESIAN_POINT('',(18.3324919694882,-66.0012330299788,27.8714803633902));
#14728=CARTESIAN_POINT('',(18.3319384476764,-65.9990409239126,27.6785196366098));
#14729=CARTESIAN_POINT('',(18.334,-66.,30.));
#14730=CARTESIAN_POINT('Ctrl Pts',(18.3319384476764,-65.9990409239126,27.6785196366098));
#14731=CARTESIAN_POINT('Ctrl Pts',(18.3315523477999,-65.9427845393862,27.6747447016724));
#14732=CARTESIAN_POINT('Ctrl Pts',(18.3341516652356,-65.886564255334,27.6709697667349));
#14733=CARTESIAN_POINT('Ctrl Pts',(18.3398540050594,-65.8306604882018,27.6671948317974));
#14734=CARTESIAN_POINT('Ctrl Pts',(18.395812479838,-65.2820629581077,27.6301504591336));
#14735=CARTESIAN_POINT('Ctrl Pts',(18.7505915016711,-64.7639459555085,27.5931060864697));
#14736=CARTESIAN_POINT('Ctrl Pts',(19.241837208723,-64.5134100171528,27.5560617138058));
#14737=CARTESIAN_POINT('Ctrl Pts',(19.7330829157748,-64.262874078797,27.519017341142));
#14738=CARTESIAN_POINT('Ctrl Pts',(20.3607953080454,-64.2799192046846,27.4819729684782));
#14739=CARTESIAN_POINT('Ctrl Pts',(20.8377208404994,-64.5567452099326,27.4449285958143));
#14740=CARTESIAN_POINT('Ctrl Pts',(21.3146463729533,-64.8335712151806,27.4078842231505));
#14741=CARTESIAN_POINT('Ctrl Pts',(21.6407850455905,-65.370178099789,27.3708398504866));
#14742=CARTESIAN_POINT('Ctrl Pts',(21.6668893856045,-65.9210039927054,27.3337954778227));
#14743=CARTESIAN_POINT('Ctrl Pts',(21.6929937256185,-66.4718298856219,27.2967511051589));
#14744=CARTESIAN_POINT('Ctrl Pts',(21.4190637330094,-67.0368747868466,27.259706732495));
#14745=CARTESIAN_POINT('Ctrl Pts',(20.970455159021,-67.3575630302712,27.2226623598312));
#14746=CARTESIAN_POINT('Ctrl Pts',(20.5218465850326,-67.6782512736958,27.1856179871673));
#14747=CARTESIAN_POINT('Ctrl Pts',(19.898559429665,-67.7545828593205,27.1485736145035));
#14748=CARTESIAN_POINT('Ctrl Pts',(19.3858221698857,-67.5516269500416,27.1115292418396));
#14749=CARTESIAN_POINT('Ctrl Pts',(18.8730849101064,-67.3486710407626,27.0744848691758));
#14750=CARTESIAN_POINT('Ctrl Pts',(18.4708975459154,-66.8664276365802,27.0374404965119));
#14751=CARTESIAN_POINT('Ctrl Pts',(18.3633089131928,-66.3255808123586,27.0003961238481));
#14752=CARTESIAN_POINT('Ctrl Pts',(18.3421301557416,-66.2191154412634,26.9931039614353));
#14753=CARTESIAN_POINT('Ctrl Pts',(18.3323670063393,-66.1103792061011,26.9858117990226));
#14754=CARTESIAN_POINT('Ctrl Pts',(18.3333666774615,-66.0014645809704,26.9785196366098));
#14755=CARTESIAN_POINT('Ctrl Pts',(18.3365470086803,-66.0005281518116,27.1714803633902));
#14756=CARTESIAN_POINT('Ctrl Pts',(18.3358499341568,-66.2456803402052,27.1878148018157));
#14757=CARTESIAN_POINT('Ctrl Pts',(18.3865446335564,-66.4905582462458,27.2041492402413));
#14758=CARTESIAN_POINT('Ctrl Pts',(18.4900816163634,-66.7105685406344,27.2204836786668));
#14759=CARTESIAN_POINT('Ctrl Pts',(18.7248899688559,-67.209523149473,27.2575280513307));
#14760=CARTESIAN_POINT('Ctrl Pts',(19.231478418021,-67.5805778746772,27.2945724239945));
#14761=CARTESIAN_POINT('Ctrl Pts',(19.7780221189842,-67.6539307712373,27.3316167966584));
#14762=CARTESIAN_POINT('Ctrl Pts',(20.3245658199475,-67.7272836677973,27.3686611693222));
#14763=CARTESIAN_POINT('Ctrl Pts',(20.911064772709,-67.5029347357133,27.4057055419861));
#14764=CARTESIAN_POINT('Ctrl Pts',(21.2691255147861,-67.0835504616866,27.4427499146499));
#14765=CARTESIAN_POINT('Ctrl Pts',(21.6271862568631,-66.66416618766,27.4797942873138));
#14766=CARTESIAN_POINT('Ctrl Pts',(21.7568087882558,-66.0497465716907,27.5168386599777));
#14767=CARTESIAN_POINT('Ctrl Pts',(21.5986752874074,-65.5214621215884,27.5538830326415));
#14768=CARTESIAN_POINT('Ctrl Pts',(21.4405417865591,-64.993177671486,27.5909274053054));
#14769=CARTESIAN_POINT('Ctrl Pts',(20.9946522534698,-64.5510283872504,27.6279717779692));
#14770=CARTESIAN_POINT('Ctrl Pts',(20.4650545136244,-64.3973504828203,27.6650161506331));
#14771=CARTESIAN_POINT('Ctrl Pts',(19.935456773779,-64.2436725783903,27.7020605232969));
#14772=CARTESIAN_POINT('Ctrl Pts',(19.3221508271775,-64.3784660537657,27.7391048959608));
#14773=CARTESIAN_POINT('Ctrl Pts',(18.9057975446667,-64.7400467618753,27.7761492686246));
#14774=CARTESIAN_POINT('Ctrl Pts',(18.548645554798,-65.0502142922492,27.8079263002132));
#14775=CARTESIAN_POINT('Ctrl Pts',(18.3364188028544,-65.5272604673683,27.8397033318017));
#14776=CARTESIAN_POINT('Ctrl Pts',(18.3324919694882,-66.0012330299788,27.8714803633902));
#14777=CARTESIAN_POINT('Origin',(20.,-66.,30.));
#14778=CARTESIAN_POINT('',(18.3327119100896,-65.9986896255405,28.5714803633902));
#14779=CARTESIAN_POINT('',(18.3362665489809,-65.9991445003998,28.3785196366098));
#14780=CARTESIAN_POINT('',(18.334,-66.,30.));
#14781=CARTESIAN_POINT('Ctrl Pts',(18.3362665489809,-65.9991445003998,28.3785196366098));
#14782=CARTESIAN_POINT('Ctrl Pts',(18.3352304947382,-65.7764847466224,28.3636776043221));
#14783=CARTESIAN_POINT('Ctrl Pts',(18.3767830304293,-65.5541958268257,28.3488355720344));
#14784=CARTESIAN_POINT('Ctrl Pts',(18.4627526639626,-65.3506686340066,28.3339935397468));
#14785=CARTESIAN_POINT('Ctrl Pts',(18.6773251079956,-64.8426831349939,28.2969491670829));
#14786=CARTESIAN_POINT('Ctrl Pts',(19.1685967650093,-64.451575039978,28.2599047944191));
#14787=CARTESIAN_POINT('Ctrl Pts',(19.7117520566309,-64.3563231101692,28.2228604217552));
#14788=CARTESIAN_POINT('Ctrl Pts',(20.2549073482526,-64.2610711803603,28.1858160490914));
#14789=CARTESIAN_POINT('Ctrl Pts',(20.849946274482,-64.4616754157586,28.1487716764275));
#14790=CARTESIAN_POINT('Ctrl Pts',(21.2245673124077,-64.8663353703955,28.1117273037637));
#14791=CARTESIAN_POINT('Ctrl Pts',(21.5991883503334,-65.2709953250324,28.0746829310998));
#14792=CARTESIAN_POINT('Ctrl Pts',(21.7533914999553,-65.8797109989079,28.0376385584359));
#14793=CARTESIAN_POINT('Ctrl Pts',(21.6166103653521,-66.4139221202436,28.0005941857721));
#14794=CARTESIAN_POINT('Ctrl Pts',(21.4798292307489,-66.9481332415792,27.9635498131082));
#14795=CARTESIAN_POINT('Ctrl Pts',(21.0520638119205,-67.407839810375,27.9265054404444));
#14796=CARTESIAN_POINT('Ctrl Pts',(20.5290679827964,-67.5826710538235,27.8894610677805));
#14797=CARTESIAN_POINT('Ctrl Pts',(20.0060721536723,-67.757502297272,27.8524166951167));
#14798=CARTESIAN_POINT('Ctrl Pts',(19.3878459142524,-67.6474582153731,27.8153723224528));
#14799=CARTESIAN_POINT('Ctrl Pts',(18.9573017584045,-67.3028971456291,27.778327949789));
#14800=CARTESIAN_POINT('Ctrl Pts',(18.5706313695867,-66.9934479033162,27.7450585120626));
#14801=CARTESIAN_POINT('Ctrl Pts',(18.3353412416341,-66.4948423914134,27.7117890743362));
#14802=CARTESIAN_POINT('Ctrl Pts',(18.3319384476764,-65.9990409239126,27.6785196366098));
#14803=CARTESIAN_POINT('Ctrl Pts',(18.3324919694882,-66.0012330299788,27.8714803633902));
#14804=CARTESIAN_POINT('Ctrl Pts',(18.3318410600215,-66.079798428407,27.8767477044655));
#14805=CARTESIAN_POINT('Ctrl Pts',(18.3369134350028,-66.1582793757284,27.8820150455408));
#14806=CARTESIAN_POINT('Ctrl Pts',(18.3479977301881,-66.2359018357232,27.8872823866162));
#14807=CARTESIAN_POINT('Ctrl Pts',(18.4259518166406,-66.7818082606177,27.92432675928));
#14808=CARTESIAN_POINT('Ctrl Pts',(18.8012606079657,-67.285253169563,27.9613711319439));
#14809=CARTESIAN_POINT('Ctrl Pts',(19.3021754152326,-67.515850264519,27.9984155046078));
#14810=CARTESIAN_POINT('Ctrl Pts',(19.8030902224995,-67.746447359475,28.0354598772716));
#14811=CARTESIAN_POINT('Ctrl Pts',(20.4296110457082,-67.7041966404415,28.0725042499354));
#14812=CARTESIAN_POINT('Ctrl Pts',(20.8950296263565,-67.4084328679382,28.1095486225993));
#14813=CARTESIAN_POINT('Ctrl Pts',(21.3604482070047,-67.112669095435,28.1465929952631));
#14814=CARTESIAN_POINT('Ctrl Pts',(21.6647645450926,-66.5633922694618,28.183637367927));
#14815=CARTESIAN_POINT('Ctrl Pts',(21.66871749542,-66.0119622752448,28.2206817405909));
#14816=CARTESIAN_POINT('Ctrl Pts',(21.6726704457474,-65.4605322810278,28.2577261132547));
#14817=CARTESIAN_POINT('Ctrl Pts',(21.3762600083143,-64.906949118567,28.2947704859186));
#14818=CARTESIAN_POINT('Ctrl Pts',(20.9151294325926,-64.6045433374158,28.3318148585824));
#14819=CARTESIAN_POINT('Ctrl Pts',(20.4539988568709,-64.3021375562647,28.3688592312463));
#14820=CARTESIAN_POINT('Ctrl Pts',(19.8281481428606,-64.2509091564231,28.4059036039101));
#14821=CARTESIAN_POINT('Ctrl Pts',(19.3239788939139,-64.4743012618234,28.442947976574));
#14822=CARTESIAN_POINT('Ctrl Pts',(18.8198096449673,-64.6976933672236,28.4799923492378));
#14823=CARTESIAN_POINT('Ctrl Pts',(18.4373218610842,-65.1957059778656,28.5170367219017));
#14824=CARTESIAN_POINT('Ctrl Pts',(18.3515494794562,-65.7404387223271,28.5540810945655));
#14825=CARTESIAN_POINT('Ctrl Pts',(18.3381207486454,-65.8257233938074,28.5598808508404));
#14826=CARTESIAN_POINT('Ctrl Pts',(18.3319650429721,-65.912153259319,28.5656806071153));
#14827=CARTESIAN_POINT('Ctrl Pts',(18.3327119100896,-65.9986896255405,28.5714803633902));
#14828=CARTESIAN_POINT('Origin',(20.,-66.,30.));
#14829=CARTESIAN_POINT('',(18.3366137500186,-65.9995968836509,29.2714803633902));
#14830=CARTESIAN_POINT('',(18.3350591945307,-66.0014219186036,29.0785196366098));
#14831=CARTESIAN_POINT('',(18.334,-66.,30.));
#14832=CARTESIAN_POINT('Ctrl Pts',(18.3350591945307,-66.0014219186036,29.0785196366098));
#14833=CARTESIAN_POINT('Ctrl Pts',(18.338211393284,-65.613442675639,29.0526105069719));
#14834=CARTESIAN_POINT('Ctrl Pts',(18.4733910015055,-65.2234834061788,29.026701377334));
#14835=CARTESIAN_POINT('Ctrl Pts',(18.7211705029757,-64.9279199131777,29.0007922476961));
#14836=CARTESIAN_POINT('Ctrl Pts',(19.0754408439409,-64.5053289449133,28.9637478750323));
#14837=CARTESIAN_POINT('Ctrl Pts',(19.6598960790816,-64.2757086908116,28.9267035023684));
#14838=CARTESIAN_POINT('Ctrl Pts',(20.2070779908308,-64.344137898032,28.8896591297046));
#14839=CARTESIAN_POINT('Ctrl Pts',(20.7542599025799,-64.4125671052524,28.8526147570407));
#14840=CARTESIAN_POINT('Ctrl Pts',(21.2641684909374,-64.779045773795,28.8155703843769));
#14841=CARTESIAN_POINT('Ctrl Pts',(21.5034595509674,-65.2758660527047,28.778526011713));
#14842=CARTESIAN_POINT('Ctrl Pts',(21.7427506109974,-65.7726863316144,28.7414816390492));
#14843=CARTESIAN_POINT('Ctrl Pts',(21.7114241426998,-66.3998482208912,28.7044372663853));
#14844=CARTESIAN_POINT('Ctrl Pts',(21.423815754467,-66.8703500975764,28.6673928937214));
#14845=CARTESIAN_POINT('Ctrl Pts',(21.1362073662343,-67.3408519742616,28.6303485210576));
#14846=CARTESIAN_POINT('Ctrl Pts',(20.5923170580665,-67.6546938383551,28.5933041483937));
#14847=CARTESIAN_POINT('Ctrl Pts',(20.041039738637,-67.6682554765002,28.5562597757299));
#14848=CARTESIAN_POINT('Ctrl Pts',(19.4897624192075,-67.6818171146452,28.519215403066));
#14849=CARTESIAN_POINT('Ctrl Pts',(18.9310980885164,-67.3950985268418,28.4821710304022));
#14850=CARTESIAN_POINT('Ctrl Pts',(18.6207025386969,-66.9393077814354,28.4451266577383));
#14851=CARTESIAN_POINT('Ctrl Pts',(18.434668678416,-66.6661321128486,28.4229243173622));
#14852=CARTESIAN_POINT('Ctrl Pts',(18.3378163925938,-66.3322233905155,28.400721976986));
#14853=CARTESIAN_POINT('Ctrl Pts',(18.3362665489809,-65.9991445003998,28.3785196366098));
#14854=CARTESIAN_POINT('Ctrl Pts',(18.3327119100896,-65.9986896255405,28.5714803633902));
#14855=CARTESIAN_POINT('Ctrl Pts',(18.3367354544376,-66.4648808649886,28.6027249797792));
#14856=CARTESIAN_POINT('Ctrl Pts',(18.5410871126712,-66.9341629934405,28.6339695961681));
#14857=CARTESIAN_POINT('Ctrl Pts',(18.8878468637807,-67.2441368803895,28.6652142125571));
#14858=CARTESIAN_POINT('Ctrl Pts',(19.2989736091057,-67.6116494157094,28.702258585221));
#14859=CARTESIAN_POINT('Ctrl Pts',(19.9102840791284,-67.755221608068,28.7393029578848));
#14860=CARTESIAN_POINT('Ctrl Pts',(20.4420305722938,-67.609151996769,28.7763473305487));
#14861=CARTESIAN_POINT('Ctrl Pts',(20.9737770654591,-67.4630823854699,28.8133917032125));
#14862=CARTESIAN_POINT('Ctrl Pts',(21.4259595817671,-67.0273709705132,28.8504360758764));
#14863=CARTESIAN_POINT('Ctrl Pts',(21.5916505028899,-66.5014078701001,28.8874804485402));
#14864=CARTESIAN_POINT('Ctrl Pts',(21.7573414240127,-65.9754447696869,28.9245248212041));
#14865=CARTESIAN_POINT('Ctrl Pts',(21.6365407499503,-65.3592299838174,28.9615691938679));
#14866=CARTESIAN_POINT('Ctrl Pts',(21.2845292464878,-64.9347555254941,28.9986135665318));
#14867=CARTESIAN_POINT('Ctrl Pts',(20.9325177430254,-64.5102810671709,29.0356579391956));
#14868=CARTESIAN_POINT('Ctrl Pts',(20.3492954101628,-64.277546936394,29.0727023118595));
#14869=CARTESIAN_POINT('Ctrl Pts',(19.8017562651217,-64.3430568515699,29.1097466845233));
#14870=CARTESIAN_POINT('Ctrl Pts',(19.2542171200805,-64.4085667667459,29.1467910571872));
#14871=CARTESIAN_POINT('Ctrl Pts',(18.7423611628609,-64.7723207278747,29.183835429851));
#14872=CARTESIAN_POINT('Ctrl Pts',(18.5004237527135,-65.2678577637357,29.2208798025149));
#14873=CARTESIAN_POINT('Ctrl Pts',(18.3902660529079,-65.4934831434804,29.23774665614));
#14874=CARTESIAN_POINT('Ctrl Pts',(18.3360656066366,-65.746428687046,29.2546135097651));
#14875=CARTESIAN_POINT('Ctrl Pts',(18.3366137500186,-65.9995968836509,29.2714803633902));
#14876=CARTESIAN_POINT('Origin',(20.,-66.,30.));
#14877=CARTESIAN_POINT('',(18.33418984545,-66.0015225986866,29.9714803633902));
#14878=CARTESIAN_POINT('',(18.3312399724094,-66.0000189542779,29.7785196366098));
#14879=CARTESIAN_POINT('',(18.334,-66.,30.));
#14880=CARTESIAN_POINT('Ctrl Pts',(18.3312400767123,-66.0000189535616,29.7785196366098));
#14881=CARTESIAN_POINT('Ctrl Pts',(18.3313326355021,-65.4495890237892,29.7415434096217));
#14882=CARTESIAN_POINT('Ctrl Pts',(18.6304405935465,-64.8990729061442,29.7045671826336));
#14883=CARTESIAN_POINT('Ctrl Pts',(19.0923261693912,-64.599682603033,29.6675909556455));
#14884=CARTESIAN_POINT('Ctrl Pts',(19.5550629814828,-64.2997405358241,29.6305465829816));
#14885=CARTESIAN_POINT('Ctrl Pts',(20.1811779492479,-64.2518507653313,29.5935022103178));
#14886=CARTESIAN_POINT('Ctrl Pts',(20.6841485416147,-64.4779285929935,29.5564578376539));
#14887=CARTESIAN_POINT('Ctrl Pts',(21.1871191339814,-64.7040064206556,29.5194134649901));
#14888=CARTESIAN_POINT('Ctrl Pts',(21.5669453509498,-65.2040518464729,29.4823690923262));
#14889=CARTESIAN_POINT('Ctrl Pts',(21.6498112407281,-65.7492342427931,29.4453247196624));
#14890=CARTESIAN_POINT('Ctrl Pts',(21.7326771305064,-66.2944166391133,29.4082803469985));
#14891=CARTESIAN_POINT('Ctrl Pts',(21.5185826930945,-66.8847360059365,29.3712359743346));
#14892=CARTESIAN_POINT('Ctrl Pts',(21.1055017563896,-67.2500505836325,29.3341916016708));
#14893=CARTESIAN_POINT('Ctrl Pts',(20.6924208196846,-67.6153651613285,29.2971472290069));
#14894=CARTESIAN_POINT('Ctrl Pts',(20.0803533836867,-67.7556749498972,29.2601028563431));
#14895=CARTESIAN_POINT('Ctrl Pts',(19.5493935524781,-67.6067714288199,29.2230584836792));
#14896=CARTESIAN_POINT('Ctrl Pts',(19.0184337212696,-67.4578679077427,29.1860141110154));
#14897=CARTESIAN_POINT('Ctrl Pts',(18.5685814948505,-67.0197510770193,29.1489697383515));
#14898=CARTESIAN_POINT('Ctrl Pts',(18.4056981050357,-66.4929118204442,29.1119253656877));
#14899=CARTESIAN_POINT('Ctrl Pts',(18.3567366569113,-66.3345481410045,29.1007901226617));
#14900=CARTESIAN_POINT('Ctrl Pts',(18.3337044404468,-66.1681678965589,29.0896548796358));
#14901=CARTESIAN_POINT('Ctrl Pts',(18.3350591945307,-66.0014219186036,29.0785196366098));
#14902=CARTESIAN_POINT('Ctrl Pts',(18.3366137500186,-65.9995968836509,29.2714803633902));
#14903=CARTESIAN_POINT('Ctrl Pts',(18.3372694842635,-66.3024575250332,29.2916578824289));
#14904=CARTESIAN_POINT('Ctrl Pts',(18.416275455694,-66.6056368032707,29.3118354014677));
#14905=CARTESIAN_POINT('Ctrl Pts',(18.5715624445679,-66.8627440673682,29.3320129205064));
#14906=CARTESIAN_POINT('Ctrl Pts',(18.8566574096448,-67.3347732245466,29.3690572931703));
#14907=CARTESIAN_POINT('Ctrl Pts',(19.3988662028737,-67.6515114283102,29.4061016658342));
#14908=CARTESIAN_POINT('Ctrl Pts',(19.9500634099081,-67.6680130432697,29.443146038498));
#14909=CARTESIAN_POINT('Ctrl Pts',(20.5012606169424,-67.6845146582292,29.4801904111619));
#14910=CARTESIAN_POINT('Ctrl Pts',(21.0614462377821,-67.4007796843847,29.5172347838257));
#14911=CARTESIAN_POINT('Ctrl Pts',(21.3742683079854,-66.9466508296172,29.5542791564896));
#14912=CARTESIAN_POINT('Ctrl Pts',(21.6870903781887,-66.4925219748497,29.5913235291534));
#14913=CARTESIAN_POINT('Ctrl Pts',(21.7525488977555,-65.8679992391592,29.6283679018173));
#14914=CARTESIAN_POINT('Ctrl Pts',(21.540688759921,-65.3588765168854,29.6654122744811));
#14915=CARTESIAN_POINT('Ctrl Pts',(21.3288286220865,-64.8497537946116,29.702456647145));
#14916=CARTESIAN_POINT('Ctrl Pts',(20.8396498268506,-64.4560310857545,29.7395010198088));
#14917=CARTESIAN_POINT('Ctrl Pts',(20.2970102178582,-64.3578836502745,29.7765453924727));
#14918=CARTESIAN_POINT('Ctrl Pts',(19.7543706088658,-64.2597362147945,29.8135897651365));
#14919=CARTESIAN_POINT('Ctrl Pts',(19.1582701861169,-64.4571640526916,29.8506341378004));
#14920=CARTESIAN_POINT('Ctrl Pts',(18.7814962342033,-64.8598203000021,29.8876785104643));
#14921=CARTESIAN_POINT('Ctrl Pts',(18.4973833084148,-65.1634502190276,29.9156124614396));
#14922=CARTESIAN_POINT('Ctrl Pts',(18.3379832586462,-65.5837766092154,29.9435464124149));
#14923=CARTESIAN_POINT('Ctrl Pts',(18.33418984545,-66.0015225986866,29.9714803633902));
#14924=CARTESIAN_POINT('Origin',(20.,-66.,30.));
#14925=CARTESIAN_POINT('',(18.3314458131932,-65.999469377919,30.6714803633902));
#14926=CARTESIAN_POINT('',(18.3350039368976,-65.9985661152072,30.4785196366098));
#14927=CARTESIAN_POINT('',(18.334,-66.,30.));
#14928=CARTESIAN_POINT('Ctrl Pts',(18.3350039368976,-65.9985661152072,30.4785196366098));
#14929=CARTESIAN_POINT('Ctrl Pts',(18.333651229393,-65.8338748785772,30.4675206849353));
#14930=CARTESIAN_POINT('Ctrl Pts',(18.3561120724071,-65.6695444482994,30.4565217332609));
#14931=CARTESIAN_POINT('Ctrl Pts',(18.4038998375659,-65.5129426455764,30.4455227815864));
#14932=CARTESIAN_POINT('Ctrl Pts',(18.5648486110225,-64.9855091490396,30.4084784089225));
#14933=CARTESIAN_POINT('Ctrl Pts',(19.0130899030193,-64.5457442946841,30.3714340362587));
#14934=CARTESIAN_POINT('Ctrl Pts',(19.5434996770359,-64.3948931343509,30.3343896635948));
#14935=CARTESIAN_POINT('Ctrl Pts',(20.0739094510525,-64.2440419740177,30.297345290931));
#14936=CARTESIAN_POINT('Ctrl Pts',(20.6864877070889,-64.3821045077068,30.2603009182671));
#14937=CARTESIAN_POINT('Ctrl Pts',(21.1009065797602,-64.745900602958,30.2232565456033));
#14938=CARTESIAN_POINT('Ctrl Pts',(21.5153254524316,-65.1096966982092,30.1862121729394));
#14939=CARTESIAN_POINT('Ctrl Pts',(21.7315849417379,-65.6992263550224,30.1491678002755));
#14940=CARTESIAN_POINT('Ctrl Pts',(21.6507204494273,-66.2447092006093,30.1121234276117));
#14941=CARTESIAN_POINT('Ctrl Pts',(21.5698559571167,-66.7901920461962,30.0750790549479));
#14942=CARTESIAN_POINT('Ctrl Pts',(21.1918674831892,-67.2916280805568,30.038034682284));
#14943=CARTESIAN_POINT('Ctrl Pts',(20.6897299920547,-67.5195503062027,30.0009903096202));
#14944=CARTESIAN_POINT('Ctrl Pts',(20.1875925009203,-67.7474725318485,29.9639459369563));
#14945=CARTESIAN_POINT('Ctrl Pts',(19.5613059925788,-67.7018809487796,29.9269015642924));
#14946=CARTESIAN_POINT('Ctrl Pts',(19.0974714984457,-67.403639162642,29.8898571916286));
#14947=CARTESIAN_POINT('Ctrl Pts',(18.6327837488041,-67.104848740191,29.852744673289));
#14948=CARTESIAN_POINT('Ctrl Pts',(18.3311471767583,-66.5524777230817,29.8156321549494));
#14949=CARTESIAN_POINT('Ctrl Pts',(18.3312400767123,-66.0000189535616,29.7785196366098));
#14950=CARTESIAN_POINT('Ctrl Pts',(18.33418984545,-66.0015225986866,29.9714803633902));
#14951=CARTESIAN_POINT('Ctrl Pts',(18.332952655842,-66.1377669175135,29.9805907850787));
#14952=CARTESIAN_POINT('Ctrl Pts',(18.3482670799087,-66.2737367634984,29.9897012067673));
#14953=CARTESIAN_POINT('Ctrl Pts',(18.3812048568464,-66.4052942882035,29.9988116284558));
#14954=CARTESIAN_POINT('Ctrl Pts',(18.5151349124813,-66.9402273723704,30.0358560011197));
#14955=CARTESIAN_POINT('Ctrl Pts',(18.940442504829,-67.4022088839804,30.0729003737835));
#14956=CARTESIAN_POINT('Ctrl Pts',(19.4624985096596,-67.5798269916133,30.1099447464474));
#14957=CARTESIAN_POINT('Ctrl Pts',(19.9845545144902,-67.7574450992461,30.1469891191112));
#14958=CARTESIAN_POINT('Ctrl Pts',(20.6033589318036,-67.6506998029017,30.1840334917751));
#14959=CARTESIAN_POINT('Ctrl Pts',(21.0357346822848,-67.3084398509142,30.2210778644389));
#14960=CARTESIAN_POINT('Ctrl Pts',(21.4681104327661,-66.9661798989267,30.2581222371028));
#14961=CARTESIAN_POINT('Ctrl Pts',(21.7140575164153,-66.3884052912962,30.2951666097666));
#14962=CARTESIAN_POINT('Ctrl Pts',(21.6610257075631,-65.8395170589677,30.3322109824305));
#14963=CARTESIAN_POINT('Ctrl Pts',(21.6079938987109,-65.2906288266393,30.3692553550943));
#14964=CARTESIAN_POINT('Ctrl Pts',(21.2559831973573,-64.770626969613,30.4062997277582));
#14965=CARTESIAN_POINT('Ctrl Pts',(20.7660806279449,-64.517474571201,30.443344100422));
#14966=CARTESIAN_POINT('Ctrl Pts',(20.2761780585324,-64.264322172789,30.4803884730859));
#14967=CARTESIAN_POINT('Ctrl Pts',(19.648383621061,-64.2780192329911,30.5174328457497));
#14968=CARTESIAN_POINT('Ctrl Pts',(19.1699884049918,-64.5522977075035,30.5544772184136));
#14969=CARTESIAN_POINT('Ctrl Pts',(18.6915931889226,-64.8265761820158,30.5915215910775));
#14970=CARTESIAN_POINT('Ctrl Pts',(18.3625971942555,-65.3614360708382,30.6285659637413));
#14971=CARTESIAN_POINT('Ctrl Pts',(18.3335554627283,-65.9121149629056,30.6656103364052));
#14972=CARTESIAN_POINT('Ctrl Pts',(18.3320214848211,-65.941201701539,30.6675670120669));
#14973=CARTESIAN_POINT('Ctrl Pts',(18.3313243580995,-65.9703325740729,30.6695236877285));
#14974=CARTESIAN_POINT('Ctrl Pts',(18.3314458131932,-65.999469377919,30.6714803633902));
#14975=CARTESIAN_POINT('Origin',(20.,-66.,30.));
#14976=CARTESIAN_POINT('',(18.3357539768147,-65.9988133681531,31.3714803633902));
#14977=CARTESIAN_POINT('',(18.3362976949234,-66.000827356963,31.1785196366098));
#14978=CARTESIAN_POINT('',(18.334,-66.,30.));
#14979=CARTESIAN_POINT('Ctrl Pts',(18.3362976949234,-66.000827356963,31.1785196366098));
#14980=CARTESIAN_POINT('Ctrl Pts',(18.3377857059205,-65.6697775954689,31.1564535875851));
#14981=CARTESIAN_POINT('Ctrl Pts',(18.4333703169726,-65.3379360998736,31.1343875385604));
#14982=CARTESIAN_POINT('Ctrl Pts',(18.6172645337012,-65.0657606167262,31.1123214895358));
#14983=CARTESIAN_POINT('Ctrl Pts',(18.9259852243695,-64.6088337778346,31.0752771168719));
#14984=CARTESIAN_POINT('Ctrl Pts',(19.4835935249369,-64.3200668023759,31.0382327442081));
#14985=CARTESIAN_POINT('Ctrl Pts',(20.0349169034394,-64.3316051411987,31.0011883715442));
#14986=CARTESIAN_POINT('Ctrl Pts',(20.5862402819419,-64.3431434800215,30.9641439988803));
#14987=CARTESIAN_POINT('Ctrl Pts',(21.1312787383795,-64.6549871331258,30.9270996262165));
#14988=CARTESIAN_POINT('Ctrl Pts',(21.420611948834,-65.1244303078278,30.8900552535526));
#14989=CARTESIAN_POINT('Ctrl Pts',(21.7099451592885,-65.5938734825299,30.8530108808888));
#14990=CARTESIAN_POINT('Ctrl Pts',(21.7435731237599,-66.2209161788296,30.8159665082249));
#14991=CARTESIAN_POINT('Ctrl Pts',(21.5061070239143,-66.7186113188203,30.7789221355611));
#14992=CARTESIAN_POINT('Ctrl Pts',(21.2686409240686,-67.2163064588109,30.7418777628972));
#14993=CARTESIAN_POINT('Ctrl Pts',(20.7600807599058,-67.5846540424924,30.7048333902334));
#14994=CARTESIAN_POINT('Ctrl Pts',(20.2131536709134,-67.6550909665624,30.6677890175695));
#14995=CARTESIAN_POINT('Ctrl Pts',(19.6662265819209,-67.7255278906324,30.6307446449057));
#14996=CARTESIAN_POINT('Ctrl Pts',(19.0809325680987,-67.4980541550909,30.5937002722418));
#14997=CARTESIAN_POINT('Ctrl Pts',(18.7251136886458,-67.0767662179611,30.556655899578));
#14998=CARTESIAN_POINT('Ctrl Pts',(18.4749420203221,-66.7805640989547,30.5306104785886));
#14999=CARTESIAN_POINT('Ctrl Pts',(18.3382071363911,-66.3885535174836,30.5045650575992));
#15000=CARTESIAN_POINT('Ctrl Pts',(18.3350039368976,-65.9985661152072,30.4785196366098));
#15001=CARTESIAN_POINT('Ctrl Pts',(18.3314458131932,-65.999469377919,30.6714803633902));
#15002=CARTESIAN_POINT('Ctrl Pts',(18.3336237824952,-66.5219593158195,30.7065680603924));
#15003=CARTESIAN_POINT('Ctrl Pts',(18.599030994634,-67.0463565704791,30.7416557573945));
#15004=CARTESIAN_POINT('Ctrl Pts',(19.0223181515937,-67.352368063378,30.7767434543967));
#15005=CARTESIAN_POINT('Ctrl Pts',(19.4692100403736,-67.6754443764704,30.8137878270606));
#15006=CARTESIAN_POINT('Ctrl Pts',(20.0920812863208,-67.755099107343,30.8508321997244));
#15007=CARTESIAN_POINT('Ctrl Pts',(20.6058937493031,-67.5548806835585,30.8878765723883));
#15008=CARTESIAN_POINT('Ctrl Pts',(21.1197062122855,-67.354662259774,30.9249209450521));
#15009=CARTESIAN_POINT('Ctrl Pts',(21.524459892303,-66.8745706813325,30.961965317716));
#15010=CARTESIAN_POINT('Ctrl Pts',(21.6349315399048,-66.334305302639,30.9990096903798));
#15011=CARTESIAN_POINT('Ctrl Pts',(21.7454031875066,-65.7940399239454,31.0360540630437));
#15012=CARTESIAN_POINT('Ctrl Pts',(21.5615928026928,-65.1936007449999,31.0730984357075));
#15013=CARTESIAN_POINT('Ctrl Pts',(21.1676156349072,-64.8077605506157,31.1101428083714));
#15014=CARTESIAN_POINT('Ctrl Pts',(20.7736384671217,-64.4219203562316,31.1471871810353));
#15015=CARTESIAN_POINT('Ctrl Pts',(20.1694945163644,-64.2506791464088,31.1842315536991));
#15016=CARTESIAN_POINT('Ctrl Pts',(19.631651943939,-64.3724002687565,31.221275926363));
#15017=CARTESIAN_POINT('Ctrl Pts',(19.0938093715137,-64.4941213911041,31.2583202990268));
#15018=CARTESIAN_POINT('Ctrl Pts',(18.6222681774202,-64.9088048456222,31.2953646716907));
#15019=CARTESIAN_POINT('Ctrl Pts',(18.432814891916,-65.4266833226324,31.3324090443545));
#15020=CARTESIAN_POINT('Ctrl Pts',(18.366208376288,-65.608755017935,31.3454328173664));
#15021=CARTESIAN_POINT('Ctrl Pts',(18.334468783344,-65.803581931597,31.3584565903783));
#15022=CARTESIAN_POINT('Ctrl Pts',(18.3357539768147,-65.9988133681531,31.3714803633902));
#15023=CARTESIAN_POINT('Origin',(20.,-66.,30.));
#15024=CARTESIAN_POINT('',(18.3357308127244,-66.0011975491724,32.0714803633902));
#15025=CARTESIAN_POINT('',(18.3319843264428,-66.0009873427492,31.8785196366098));
#15026=CARTESIAN_POINT('',(18.334,-66.,30.));
#15027=CARTESIAN_POINT('Ctrl Pts',(18.3319843264428,-66.0009873427492,31.8785196366098));
#15028=CARTESIAN_POINT('Ctrl Pts',(18.3354516848774,-65.5071812495811,31.8453864902349));
#15029=CARTESIAN_POINT('Ctrl Pts',(18.5685743737179,-65.010531129917,31.81225334386));
#15030=CARTESIAN_POINT('Ctrl Pts',(18.952527100275,-64.7009383696829,31.7791201974851));
#15031=CARTESIAN_POINT('Ctrl Pts',(19.381803804846,-64.3547995075786,31.7420758248213));
#15032=CARTESIAN_POINT('Ctrl Pts',(19.9996220148609,-64.2424872537891,31.7050314521574));
#15033=CARTESIAN_POINT('Ctrl Pts',(20.523255958873,-64.4153979059321,31.6679870794935));
#15034=CARTESIAN_POINT('Ctrl Pts',(21.0468899028851,-64.5883085580752,31.6309427068297));
#15035=CARTESIAN_POINT('Ctrl Pts',(21.4763395808944,-65.0464421161508,31.5938983341658));
#15036=CARTESIAN_POINT('Ctrl Pts',(21.6150803687566,-65.5801476480029,31.556853961502));
#15037=CARTESIAN_POINT('Ctrl Pts',(21.7538211566187,-66.1138531798551,31.5198095888381));
#15038=CARTESIAN_POINT('Ctrl Pts',(21.6018530543337,-66.7231306854838,31.4827652161743));
#15039=CARTESIAN_POINT('Ctrl Pts',(21.2287196562103,-67.129162787849,31.4457208435104));
#15040=CARTESIAN_POINT('Ctrl Pts',(20.8555862580868,-67.5351948902141,31.4086764708466));
#15041=CARTESIAN_POINT('Ctrl Pts',(20.2612875641249,-67.7379815893157,31.3716320981827));
#15042=CARTESIAN_POINT('Ctrl Pts',(19.7177863523659,-67.6447237008414,31.3345877255189));
#15043=CARTESIAN_POINT('Ctrl Pts',(19.1742851406069,-67.5514658123671,31.297543352855));
#15044=CARTESIAN_POINT('Ctrl Pts',(18.6815814110507,-67.162163336317,31.2604989801912));
#15045=CARTESIAN_POINT('Ctrl Pts',(18.4651460866572,-66.6549687471297,31.2234546075273));
#15046=CARTESIAN_POINT('Ctrl Pts',(18.3776337844479,-66.4498923979142,31.2084762838881));
#15047=CARTESIAN_POINT('Ctrl Pts',(18.3352876405059,-66.225542278188,31.193497960249));
#15048=CARTESIAN_POINT('Ctrl Pts',(18.3362976949234,-66.000827356963,31.1785196366098));
#15049=CARTESIAN_POINT('Ctrl Pts',(18.3357539768147,-65.9988133681531,31.3714803633902));
#15050=CARTESIAN_POINT('Ctrl Pts',(18.338124343513,-66.3588915246679,31.3955009630422));
#15051=CARTESIAN_POINT('Ctrl Pts',(18.452834619963,-66.7203457405113,31.4195215626941));
#15052=CARTESIAN_POINT('Ctrl Pts',(18.6683273346162,-67.0056883651597,31.4435421623461));
#15053=CARTESIAN_POINT('Ctrl Pts',(19.0006584397354,-67.4457414311745,31.4805865350099));
#15054=CARTESIAN_POINT('Ctrl Pts',(19.5726860268885,-67.7047740637018,31.5176309076738));
#15055=CARTESIAN_POINT('Ctrl Pts',(20.122639014801,-67.6642478323845,31.5546752803376));
#15056=CARTESIAN_POINT('Ctrl Pts',(20.6725920027136,-67.6237216010672,31.5917196530015));
#15057=CARTESIAN_POINT('Ctrl Pts',(21.2004703913856,-67.2836365059054,31.6287640256653));
#15058=CARTESIAN_POINT('Ctrl Pts',(21.4647066416153,-66.7996221792546,31.6658083983292));
#15059=CARTESIAN_POINT('Ctrl Pts',(21.728942891845,-66.3156078526038,31.702852770993));
#15060=CARTESIAN_POINT('Ctrl Pts',(21.7295370036324,-65.6876642944639,31.7398971436569));
#15061=CARTESIAN_POINT('Ctrl Pts',(21.4662170997316,-65.2031508348486,31.7769415163208));
#15062=CARTESIAN_POINT('Ctrl Pts',(21.2028971958308,-64.7186373752333,31.8139858889846));
#15063=CARTESIAN_POINT('Ctrl Pts',(20.6756632762418,-64.3775540141426,31.8510302616484));
#15064=CARTESIAN_POINT('Ctrl Pts',(20.1257879584309,-64.3359872100667,31.8880746343123));
#15065=CARTESIAN_POINT('Ctrl Pts',(19.57591264062,-64.2944204059907,31.9251190069761));
#15066=CARTESIAN_POINT('Ctrl Pts',(19.0033959245872,-64.5523701589297,31.96216337964));
#15067=CARTESIAN_POINT('Ctrl Pts',(18.6702327266084,-64.9917935855369,31.9992077523039));
#15068=CARTESIAN_POINT('Ctrl Pts',(18.4535684714254,-65.2775614915163,32.023298622666));
#15069=CARTESIAN_POINT('Ctrl Pts',(18.3381321348796,-65.6400786444767,32.0473894930281));
#15070=CARTESIAN_POINT('Ctrl Pts',(18.3357308127244,-66.0011975491724,32.0714803633902));
#15071=CARTESIAN_POINT('Origin',(20.,-66.,30.));
#15072=CARTESIAN_POINT('',(18.3314319388862,-66.0005124578368,32.7714803633902));
#15073=CARTESIAN_POINT('',(18.3333053457166,-65.9985455597719,32.5785196366098));
#15074=CARTESIAN_POINT('',(18.334,-66.,30.));
#15075=CARTESIAN_POINT('Ctrl Pts',(18.3333053457166,-65.9985455597719,32.5785196366098));
#15076=CARTESIAN_POINT('Ctrl Pts',(18.3323271587739,-65.8916766923834,32.5713637655485));
#15077=CARTESIAN_POINT('Ctrl Pts',(18.3417256832142,-65.7849791876526,32.5642078944873));
#15078=CARTESIAN_POINT('Ctrl Pts',(18.3621250373911,-65.6804280959176,32.557052023426));
#15079=CARTESIAN_POINT('Ctrl Pts',(18.4677280131519,-65.1391900591385,32.5200076507622));
#15080=CARTESIAN_POINT('Ctrl Pts',(18.8681428272523,-64.6554738617393,32.4829632780983));
#15081=CARTESIAN_POINT('Ctrl Pts',(19.3801317806736,-64.4506375550925,32.4459189054345));
#15082=CARTESIAN_POINT('Ctrl Pts',(19.892120734095,-64.2458012484457,32.4088745327706));
#15083=CARTESIAN_POINT('Ctrl Pts',(20.5156838268372,-64.3198448325512,32.3718301601068));
#15084=CARTESIAN_POINT('Ctrl Pts',(20.9654663160592,-64.6388845061585,32.3347857874429));
#15085=CARTESIAN_POINT('Ctrl Pts',(21.4152488052812,-64.9579241797659,32.297741414779));
#15086=CARTESIAN_POINT('Ctrl Pts',(21.691250690983,-65.5219599428751,32.2606970421152));
#15087=CARTESIAN_POINT('Ctrl Pts',(21.6671680786034,-66.0728779301719,32.2236526694513));
#15088=CARTESIAN_POINT('Ctrl Pts',(21.6430854662238,-66.6237959174687,32.1866082967875));
#15089=CARTESIAN_POINT('Ctrl Pts',(21.3189183557627,-67.1615961289531,32.1495639241236));
#15090=CARTESIAN_POINT('Ctrl Pts',(20.8430119965137,-67.4401706040447,32.1125195514598));
#15091=CARTESIAN_POINT('Ctrl Pts',(20.3671056372647,-67.7187450791363,32.0754751787959));
#15092=CARTESIAN_POINT('Ctrl Pts',(19.7394600292277,-67.7380938178351,32.0384308061321));
#15093=CARTESIAN_POINT('Ctrl Pts',(19.2472981545858,-67.4893624565331,32.0013864334682));
#15094=CARTESIAN_POINT('Ctrl Pts',(18.7551362799438,-67.2406310952312,31.9643420608044));
#15095=CARTESIAN_POINT('Ctrl Pts',(18.3984581386968,-66.7238196339284,31.9272976881405));
#15096=CARTESIAN_POINT('Ctrl Pts',(18.3404866676369,-66.1754311680674,31.8902533154767));
#15097=CARTESIAN_POINT('Ctrl Pts',(18.3343659123018,-66.1175311084903,31.8863420891877));
#15098=CARTESIAN_POINT('Ctrl Pts',(18.3315750196022,-66.0592790410803,31.8824308628988));
#15099=CARTESIAN_POINT('Ctrl Pts',(18.3319843264428,-66.0009873427492,31.8785196366098));
#15100=CARTESIAN_POINT('Ctrl Pts',(18.3357308127244,-66.0011975491724,32.0714803633902));
#15101=CARTESIAN_POINT('Ctrl Pts',(18.3344396376196,-66.195368805456,32.0844338656919));
#15102=CARTESIAN_POINT('Ctrl Pts',(18.3658284909666,-66.3891358083027,32.0973873679937));
#15103=CARTESIAN_POINT('Ctrl Pts',(18.4317328425237,-66.5703501541415,32.1103408702954));
#15104=CARTESIAN_POINT('Ctrl Pts',(18.6202058363429,-67.0885861958634,32.1473852429593));
#15105=CARTESIAN_POINT('Ctrl Pts',(19.0909615039061,-67.5041611790318,32.1844296156231));
#15106=CARTESIAN_POINT('Ctrl Pts',(19.6285727873552,-67.6268998129126,32.221473988287));
#15107=CARTESIAN_POINT('Ctrl Pts',(20.1661840708043,-67.7496384467933,32.2585183609508));
#15108=CARTESIAN_POINT('Ctrl Pts',(20.7706509701393,-67.5795407313865,32.2955627336147));
#15109=CARTESIAN_POINT('Ctrl Pts',(21.1653575364318,-67.1944467287532,32.3326071062785));
#15110=CARTESIAN_POINT('Ctrl Pts',(21.5600641027243,-66.8093527261198,32.3696514789424));
#15111=CARTESIAN_POINT('Ctrl Pts',(21.7450103359744,-66.20926243626,32.4066958516063));
#15112=CARTESIAN_POINT('Ctrl Pts',(21.6355612001404,-65.6687889854742,32.4437402242701));
#15113=CARTESIAN_POINT('Ctrl Pts',(21.5261120643063,-65.1283155346885,32.480784596934));
#15114=CARTESIAN_POINT('Ctrl Pts',(21.1222675593881,-64.6474589229769,32.5178289695978));
#15115=CARTESIAN_POINT('Ctrl Pts',(20.6088348784189,-64.4462685990267,32.5548733422617));
#15116=CARTESIAN_POINT('Ctrl Pts',(20.0954021974497,-64.2450782750765,32.5919177149255));
#15117=CARTESIAN_POINT('Ctrl Pts',(19.4723813404294,-64.3235542388877,32.6289620875894));
#15118=CARTESIAN_POINT('Ctrl Pts',(19.0248789124613,-64.6457843450241,32.6660064602532));
#15119=CARTESIAN_POINT('Ctrl Pts',(18.600164582529,-64.9516055765046,32.7011644279656));
#15120=CARTESIAN_POINT('Ctrl Pts',(18.3335480283789,-65.4769877278693,32.7363223956779));
#15121=CARTESIAN_POINT('Ctrl Pts',(18.3314319388862,-66.0005124578368,32.7714803633902));
#15122=CARTESIAN_POINT('Origin',(20.,-66.,30.));
#15123=CARTESIAN_POINT('',(18.3342213249666,-65.9984780340466,33.4714803633902));
#15124=CARTESIAN_POINT('',(18.3367010446132,-65.9999263102719,33.2785196366098));
#15125=CARTESIAN_POINT('',(18.334,-66.,30.));
#15126=CARTESIAN_POINT('Ctrl Pts',(18.3367010446132,-65.9999263102719,33.2785196366098));
#15127=CARTESIAN_POINT('Ctrl Pts',(18.3365931047954,-65.7263673738448,33.2602966681983));
#15128=CARTESIAN_POINT('Ctrl Pts',(18.4003187588333,-65.4528557910589,33.2420736997868));
#15129=CARTESIAN_POINT('Ctrl Pts',(18.5281536212252,-65.2135975379756,33.2238507313754));
#15130=CARTESIAN_POINT('Ctrl Pts',(18.7880213977008,-64.7272238753543,33.1868063587115));
#15131=CARTESIAN_POINT('Ctrl Pts',(19.3128164406399,-64.3823999407418,33.1497619860477));
#15132=CARTESIAN_POINT('Ctrl Pts',(19.8623822105493,-64.3369239527128,33.1127176133838));
#15133=CARTESIAN_POINT('Ctrl Pts',(20.4119479804586,-64.2914479646837,33.07567324072));
#15134=CARTESIAN_POINT('Ctrl Pts',(20.9862844773381,-64.545319923238,33.0386288680561));
#15135=CARTESIAN_POINT('Ctrl Pts',(21.3225640173729,-64.9823630239762,33.0015844953923));
#15136=CARTESIAN_POINT('Ctrl Pts',(21.6588435574077,-65.4194061247144,32.9645401227284));
#15137=CARTESIAN_POINT('Ctrl Pts',(21.7570661405977,-66.0396203676365,32.9274957500645));
#15138=CARTESIAN_POINT('Ctrl Pts',(21.572283179879,-66.5591835094909,32.8904513774007));
#15139=CARTESIAN_POINT('Ctrl Pts',(21.3875002191603,-67.0787466513452,32.8534070047368));
#15140=CARTESIAN_POINT('Ctrl Pts',(20.9197117145329,-67.4976586921317,32.816362632073));
#15141=CARTESIAN_POINT('Ctrl Pts',(20.3829868916996,-67.6242172378744,32.7793182594091));
#15142=CARTESIAN_POINT('Ctrl Pts',(19.8462620688664,-67.7507757836172,32.7422738867453));
#15143=CARTESIAN_POINT('Ctrl Pts',(19.2406009278272,-67.5849808343162,32.7052295140814));
#15144=CARTESIAN_POINT('Ctrl Pts',(18.8431659260182,-67.2027034215861,32.6681851414176));
#15145=CARTESIAN_POINT('Ctrl Pts',(18.5225035464367,-66.8942706356756,32.638296639815));
#15146=CARTESIAN_POINT('Ctrl Pts',(18.3373910177132,-66.4449133446109,32.6084081382124));
#15147=CARTESIAN_POINT('Ctrl Pts',(18.3333053457166,-65.9985455597719,32.5785196366098));
#15148=CARTESIAN_POINT('Ctrl Pts',(18.3314319388862,-66.0005124578368,32.7714803633902));
#15149=CARTESIAN_POINT('Ctrl Pts',(18.3313183998521,-66.0286022396733,32.7733667683417));
#15150=CARTESIAN_POINT('Ctrl Pts',(18.3319663237535,-66.0566866742318,32.7752531732933));
#15151=CARTESIAN_POINT('Ctrl Pts',(18.3333921462108,-66.0847315598599,32.7771395782448));
#15152=CARTESIAN_POINT('Ctrl Pts',(18.3613918068445,-66.6354644200977,32.8141839509086));
#15153=CARTESIAN_POINT('Ctrl Pts',(18.6893751270277,-67.1709458921119,32.8512283235725));
#15154=CARTESIAN_POINT('Ctrl Pts',(19.1672504847947,-67.4461291161188,32.8882726962364));
#15155=CARTESIAN_POINT('Ctrl Pts',(19.6451258425617,-67.7213123401258,32.9253170689002));
#15156=CARTESIAN_POINT('Ctrl Pts',(20.2728932379124,-67.7361973161255,32.962361441564));
#15157=CARTESIAN_POINT('Ctrl Pts',(20.7632739563948,-67.4839723862013,32.9994058142279));
#15158=CARTESIAN_POINT('Ctrl Pts',(21.2536546748772,-67.231747456277,33.0364501868917));
#15159=CARTESIAN_POINT('Ctrl Pts',(21.6066487164913,-66.7124126204288,33.0734945595556));
#15160=CARTESIAN_POINT('Ctrl Pts',(21.6607190609346,-66.1636257198826,33.1105389322195));
#15161=CARTESIAN_POINT('Ctrl Pts',(21.7147894053779,-65.6148388193364,33.1475833048833));
#15162=CARTESIAN_POINT('Ctrl Pts',(21.4699360526505,-65.0365998540921,33.1846276775472));
#15163=CARTESIAN_POINT('Ctrl Pts',(21.038208715637,-64.6935223544135,33.221672050211));
#15164=CARTESIAN_POINT('Ctrl Pts',(20.6064813786234,-64.3504448547349,33.2587164228749));
#15165=CARTESIAN_POINT('Ctrl Pts',(19.9878800573237,-64.2425288206219,33.2957607955387));
#15166=CARTESIAN_POINT('Ctrl Pts',(19.4654888903011,-64.4191587527804,33.3328051682026));
#15167=CARTESIAN_POINT('Ctrl Pts',(18.9430977232784,-64.5957886849389,33.3698495408664));
#15168=CARTESIAN_POINT('Ctrl Pts',(18.5169167105327,-65.0569645833689,33.4068939135303));
#15169=CARTESIAN_POINT('Ctrl Pts',(18.3819746706949,-65.5916432816362,33.4439382861941));
#15170=CARTESIAN_POINT('Ctrl Pts',(18.3485320377033,-65.7241524944515,33.4531189785928));
#15171=CARTESIAN_POINT('Ctrl Pts',(18.3329771612274,-65.8611762135967,33.4622996709915));
#15172=CARTESIAN_POINT('Ctrl Pts',(18.3342213249666,-65.9984780340466,33.4714803633902));
#15173=CARTESIAN_POINT('Origin',(20.,-66.,30.));
#15174=CARTESIAN_POINT('',(18.3366059788164,-66.0004198226349,34.1714803633902));
#15175=CARTESIAN_POINT('',(18.3335758017906,-66.001492963312,33.9785196366098));
#15176=CARTESIAN_POINT('',(18.334,-66.,30.));
#15177=CARTESIAN_POINT('Ctrl Pts',(18.3335758017906,-66.001492963312,33.9785196366098));
#15178=CARTESIAN_POINT('Ctrl Pts',(18.3376146481614,-65.563879799351,33.9492295708481));
#15179=CARTESIAN_POINT('Ctrl Pts',(18.5146051988431,-65.1233755891636,33.9199395050864));
#15180=CARTESIAN_POINT('Ctrl Pts',(18.8239358304384,-64.8160938964247,33.8906494393248));
#15181=CARTESIAN_POINT('Ctrl Pts',(19.2151592331577,-64.4274618724746,33.8536050666609));
#15182=CARTESIAN_POINT('Ctrl Pts',(19.8180701248551,-64.2519288582829,33.816560693997));
#15183=CARTESIAN_POINT('Ctrl Pts',(20.3567646176707,-64.3698222172911,33.7795163213332));
#15184=CARTESIAN_POINT('Ctrl Pts',(20.8954591104862,-64.4877155762994,33.7424719486693));
#15185=CARTESIAN_POINT('Ctrl Pts',(21.3699372044197,-64.8990353085074,33.7054275760055));
#15186=CARTESIAN_POINT('Ctrl Pts',(21.5630683853716,-65.4155534089152,33.6683832033416));
#15187=CARTESIAN_POINT('Ctrl Pts',(21.7561995663234,-65.9320715093229,33.6313388306778));
#15188=CARTESIAN_POINT('Ctrl Pts',(21.6679838342935,-66.5537879779303,33.5942944580139));
#15189=CARTESIAN_POINT('Ctrl Pts',(21.3387904446675,-66.9961931238673,33.55725008535));
#15190=CARTESIAN_POINT('Ctrl Pts',(21.0095970550415,-67.4385982698042,33.5202057126862));
#15191=CARTESIAN_POINT('Ctrl Pts',(20.4394260078194,-67.7016920930707,33.4831613400223));
#15192=CARTESIAN_POINT('Ctrl Pts',(19.8891987948963,-67.6650776822906,33.4461169673585));
#15193=CARTESIAN_POINT('Ctrl Pts',(19.3389715819732,-67.6284632715105,33.4090725946946));
#15194=CARTESIAN_POINT('Ctrl Pts',(18.8086882033491,-67.2921406266838,33.3720282220308));
#15195=CARTESIAN_POINT('Ctrl Pts',(18.5410167690432,-66.8100176089554,33.3349838493669));
#15196=CARTESIAN_POINT('Ctrl Pts',(18.4050189936833,-66.56506185553,33.3161624451146));
#15197=CARTESIAN_POINT('Ctrl Pts',(18.3368125291365,-66.2824688254694,33.2973410408622));
#15198=CARTESIAN_POINT('Ctrl Pts',(18.3367010446132,-65.9999263102719,33.2785196366098));
#15199=CARTESIAN_POINT('Ctrl Pts',(18.3342213249666,-65.9984780340466,33.4714803633902));
#15200=CARTESIAN_POINT('Ctrl Pts',(18.3379973997026,-66.41519322923,33.4993440436554));
#15201=CARTESIAN_POINT('Ctrl Pts',(18.4965163106871,-66.8344701293732,33.5272077239205));
#15202=CARTESIAN_POINT('Ctrl Pts',(18.779340917363,-67.1378719524441,33.5550714041857));
#15203=CARTESIAN_POINT('Ctrl Pts',(19.155352270799,-67.5412404268801,33.5921157768495));
#15204=CARTESIAN_POINT('Ctrl Pts',(19.7510780446009,-67.7397958776474,33.6291601495134));
#15205=CARTESIAN_POINT('Ctrl Pts',(20.2939024010583,-67.6426754250913,33.6662045221772));
#15206=CARTESIAN_POINT('Ctrl Pts',(20.8367267575157,-67.5455549725352,33.7032488948411));
#15207=CARTESIAN_POINT('Ctrl Pts',(21.3266496966286,-67.1527586166557,33.740293267505));
#15208=CARTESIAN_POINT('Ctrl Pts',(21.5394728395698,-66.6440376957742,33.7773376401688));
#15209=CARTESIAN_POINT('Ctrl Pts',(21.752295982511,-66.1353167748926,33.8143820128327));
#15210=CARTESIAN_POINT('Ctrl Pts',(21.6880193292805,-65.5106712890091,33.8514263854965));
#15211=CARTESIAN_POINT('Ctrl Pts',(21.3760571419463,-65.0559513139131,33.8884707581604));
#15212=CARTESIAN_POINT('Ctrl Pts',(21.0640949546121,-64.6012313388172,33.9255151308242));
#15213=CARTESIAN_POINT('Ctrl Pts',(20.5044472331742,-64.316436874509,33.9625595034881));
#15214=CARTESIAN_POINT('Ctrl Pts',(19.9532197875309,-64.3318954555163,33.9996038761519));
#15215=CARTESIAN_POINT('Ctrl Pts',(19.4019923418877,-64.3473540365236,34.0366482488158));
#15216=CARTESIAN_POINT('Ctrl Pts',(18.859185172039,-64.6630656628465,34.0736926214796));
#15217=CARTESIAN_POINT('Ctrl Pts',(18.5731975236246,-65.1345545151115,34.1107369941435));
#15218=CARTESIAN_POINT('Ctrl Pts',(18.416881803868,-65.3922618661374,34.1309847838924));
#15219=CARTESIAN_POINT('Ctrl Pts',(18.3372914182245,-65.6965079679593,34.1512325736413));
#15220=CARTESIAN_POINT('Ctrl Pts',(18.3366059788164,-66.0004198226349,34.1714803633902));
#15221=CARTESIAN_POINT('Origin',(20.,-66.,30.));
#15222=CARTESIAN_POINT('',(18.332682461926,-66.0013023226252,34.8714803633902));
#15223=CARTESIAN_POINT('',(18.3317911996431,-65.9991411289371,34.6785196366098));
#15224=CARTESIAN_POINT('',(18.334,-66.,30.));
#15225=CARTESIAN_POINT('Ctrl Pts',(18.3317911996431,-65.9991411289371,34.6785196366098));
#15226=CARTESIAN_POINT('Ctrl Pts',(18.331481150105,-65.9497833776327,34.6752068461618));
#15227=CARTESIAN_POINT('Ctrl Pts',(18.3334818713826,-65.9004511145936,34.6718940557137));
#15228=CARTESIAN_POINT('Ctrl Pts',(18.3378752000437,-65.851332857239,34.6685812652657));
#15229=CARTESIAN_POINT('Ctrl Pts',(18.3870023955927,-65.3020813852329,34.6315368926018));
#15230=CARTESIAN_POINT('Ctrl Pts',(18.7353064493333,-64.7795896519118,34.5944925199379));
#15231=CARTESIAN_POINT('Ctrl Pts',(19.2233964026499,-64.5229599453814,34.5574481472741));
#15232=CARTESIAN_POINT('Ctrl Pts',(19.7114863559666,-64.2663302388509,34.5204037746102));
#15233=CARTESIAN_POINT('Ctrl Pts',(20.3393622088594,-64.275562559111,34.4833594019464));
#15234=CARTESIAN_POINT('Ctrl Pts',(20.8196956993778,-64.5464321208658,34.4463150292825));
#15235=CARTESIAN_POINT('Ctrl Pts',(21.3000291898962,-64.8173016826206,34.4092706566187));
#15236=CARTESIAN_POINT('Ctrl Pts',(21.6328203180401,-65.3498084858701,34.3722262839548));
#15237=CARTESIAN_POINT('Ctrl Pts',(21.6657772717621,-65.9002668845694,34.335181911291));
#15238=CARTESIAN_POINT('Ctrl Pts',(21.698734225484,-66.4507252832687,34.2981375386271));
#15239=CARTESIAN_POINT('Ctrl Pts',(21.4318570047839,-67.0191352774177,34.2610931659632));
#15240=CARTESIAN_POINT('Ctrl Pts',(20.9872738992879,-67.3453812942044,34.2240487932994));
#15241=CARTESIAN_POINT('Ctrl Pts',(20.5426907937918,-67.671627310991,34.1870044206355));
#15242=CARTESIAN_POINT('Ctrl Pts',(19.9204018034998,-67.7557093504152,34.1499600479717));
#15243=CARTESIAN_POINT('Ctrl Pts',(19.405178606192,-67.5591498031194,34.1129156753078));
#15244=CARTESIAN_POINT('Ctrl Pts',(18.8899554088842,-67.3625902558236,34.075871302644));
#15245=CARTESIAN_POINT('Ctrl Pts',(18.4817980045605,-66.8853891218078,34.0388269299801));
#15246=CARTESIAN_POINT('Ctrl Pts',(18.3674872592693,-66.3459230379456,34.0017825573163));
#15247=CARTESIAN_POINT('Ctrl Pts',(18.3435591822778,-66.2329993932254,33.9940282504141));
#15248=CARTESIAN_POINT('Ctrl Pts',(18.3325065500332,-66.1173474924684,33.986273943512));
#15249=CARTESIAN_POINT('Ctrl Pts',(18.3335758017906,-66.001492963312,33.9785196366098));
#15250=CARTESIAN_POINT('Ctrl Pts',(18.3366059788164,-66.0004198226349,34.1714803633902));
#15251=CARTESIAN_POINT('Ctrl Pts',(18.336037371576,-66.2525303358908,34.1882769463051));
#15252=CARTESIAN_POINT('Ctrl Pts',(18.3897676428184,-66.5044108351101,34.2050735292201));
#15253=CARTESIAN_POINT('Ctrl Pts',(18.4990410468759,-66.729303380124,34.2218701121351));
#15254=CARTESIAN_POINT('Ctrl Pts',(18.7400403455219,-67.2252973146641,34.2589144847989));
#15255=CARTESIAN_POINT('Ctrl Pts',(19.2512070697942,-67.5900191055372,34.2959588574628));
#15256=CARTESIAN_POINT('Ctrl Pts',(19.7986212764483,-67.6565650186632,34.3330032301266));
#15257=CARTESIAN_POINT('Ctrl Pts',(20.3460354831024,-67.7231109317891,34.3700476027905));
#15258=CARTESIAN_POINT('Ctrl Pts',(20.9296971721382,-67.491480967168,34.4070919754543));
#15259=CARTESIAN_POINT('Ctrl Pts',(21.2825112494692,-67.0676732857095,34.4441363481182));
#15260=CARTESIAN_POINT('Ctrl Pts',(21.6353253268003,-66.643865604251,34.481180720782));
#15261=CARTESIAN_POINT('Ctrl Pts',(21.7572917924265,-66.0278802059553,34.5182250934459));
#15262=CARTESIAN_POINT('Ctrl Pts',(21.5925964289533,-65.5016046685849,34.5552694661097));
#15263=CARTESIAN_POINT('Ctrl Pts',(21.4279010654802,-64.9753291312145,34.5923138387736));
#15264=CARTESIAN_POINT('Ctrl Pts',(20.9765438729076,-64.5387634547694,34.6293582114374));
#15265=CARTESIAN_POINT('Ctrl Pts',(20.4450747103033,-64.3916876135341,34.6664025841013));
#15266=CARTESIAN_POINT('Ctrl Pts',(19.9136055476989,-64.2446117722988,34.7034469567651));
#15267=CARTESIAN_POINT('Ctrl Pts',(19.3020244150628,-64.3870257662733,34.740491329429));
#15268=CARTESIAN_POINT('Ctrl Pts',(18.8902030237858,-64.7537602841853,34.7775357020928));
#15269=CARTESIAN_POINT('Ctrl Pts',(18.5420761843907,-65.0637736329866,34.808850589192));
#15270=CARTESIAN_POINT('Ctrl Pts',(18.3366957496508,-65.5340842872638,34.8401654762911));
#15271=CARTESIAN_POINT('Ctrl Pts',(18.332682461926,-66.0013023226252,34.8714803633902));
#15272=CARTESIAN_POINT('Origin',(20.,-66.,30.));
#15273=CARTESIAN_POINT('',(18.3325226604529,-65.9987867968397,35.5714803633902));
#15274=CARTESIAN_POINT('',(18.3361559831984,-65.999055845664,35.3785196366098));
#15275=CARTESIAN_POINT('',(18.334,-66.,30.));
#15276=CARTESIAN_POINT('',(21.2690708798524,-64.9206413469515,36.));
#15277=CARTESIAN_POINT('Ctrl Pts',(18.3325226604529,-65.9987867968397,35.5714803633902));
#15278=CARTESIAN_POINT('Ctrl Pts',(18.3364573709904,-66.4716253136251,35.6031871242686));
#15279=CARTESIAN_POINT('Ctrl Pts',(18.5476202216759,-66.9474487737269,35.634893885147));
#15280=CARTESIAN_POINT('Ctrl Pts',(18.9034044398461,-67.2577324547277,35.6666006460253));
#15281=CARTESIAN_POINT('Ctrl Pts',(19.3190824467032,-67.6202502267133,35.7036450186892));
#15282=CARTESIAN_POINT('Ctrl Pts',(19.9321722943361,-67.7568019946271,35.740689391353));
#15283=CARTESIAN_POINT('Ctrl Pts',(20.4620469760753,-67.6038093106228,35.7777337640169));
#15284=CARTESIAN_POINT('Ctrl Pts',(20.9919216578146,-67.4508166266185,35.8147781366807));
#15285=CARTESIAN_POINT('Ctrl Pts',(21.4385811736603,-67.0082794906961,35.8518225093446));
#15286=CARTESIAN_POINT('Ctrl Pts',(21.5975927337787,-66.4812302053523,35.8888668820085));
#15287=CARTESIAN_POINT('Ctrl Pts',(21.756604293897,-65.9541809200085,35.9259112546723));
#15288=CARTESIAN_POINT('Ctrl Pts',(21.627967898288,-65.3426194852432,35.9629556273362));
#15289=CARTESIAN_POINT('Ctrl Pts',(21.2690708798524,-64.9206413469514,36.));
#15290=CARTESIAN_POINT('',(18.7285279290194,-64.9187949404949,36.));
#15291=CARTESIAN_POINT('Origin',(20.,-66.,36.));
#15292=CARTESIAN_POINT('Ctrl Pts',(18.7285264739144,-64.9187938215856,36.));
#15293=CARTESIAN_POINT('Ctrl Pts',(19.0793427655227,-64.5073237570503,35.9636818543909));
#15294=CARTESIAN_POINT('Ctrl Pts',(19.6492096702252,-64.2812825989047,35.9273637087819));
#15295=CARTESIAN_POINT('Ctrl Pts',(20.1865491454986,-64.341804902964,35.8910455631728));
#15296=CARTESIAN_POINT('Ctrl Pts',(20.7346334002206,-64.4035374267052,35.8540011905089));
#15297=CARTESIAN_POINT('Ctrl Pts',(21.2488763655857,-64.7634083897207,35.8169568178451));
#15298=CARTESIAN_POINT('Ctrl Pts',(21.4942849262207,-65.2571540480588,35.7799124451812));
#15299=CARTESIAN_POINT('Ctrl Pts',(21.7396934868558,-65.7508997063968,35.7428680725174));
#15300=CARTESIAN_POINT('Ctrl Pts',(21.7162676427607,-66.3785200600576,35.7058236998535));
#15301=CARTESIAN_POINT('Ctrl Pts',(21.434559910799,-66.8525937901543,35.6687793271897));
#15302=CARTESIAN_POINT('Ctrl Pts',(21.1528521788373,-67.326667520251,35.6317349545258));
#15303=CARTESIAN_POINT('Ctrl Pts',(20.6128625590089,-67.6471946267836,35.594690581862));
#15304=CARTESIAN_POINT('Ctrl Pts',(20.0617849892622,-67.6676008155073,35.5576462091981));
#15305=CARTESIAN_POINT('Ctrl Pts',(19.5107074195156,-67.6880070042309,35.5206018365343));
#15306=CARTESIAN_POINT('Ctrl Pts',(18.9485418998507,-67.4082922751456,35.4835574638704));
#15307=CARTESIAN_POINT('Ctrl Pts',(18.6325042689313,-66.956406817939,35.4465130912066));
#15308=CARTESIAN_POINT('Ctrl Pts',(18.4391461530328,-66.679934296761,35.423848606341));
#15309=CARTESIAN_POINT('Ctrl Pts',(18.3379195160153,-66.3390142077648,35.4011841214754));
#15310=CARTESIAN_POINT('Ctrl Pts',(18.3361559831984,-65.999055845664,35.3785196366098));
#15311=CARTESIAN_POINT('Origin',(20.,-66.,37.5459252805377));
#15312=CARTESIAN_POINT('',(17.9445921681644,-65.9981769380503,25.3540747194623));
#15313=CARTESIAN_POINT('',(17.9470733560714,-66.0015060535927,25.2959252805377));
#15314=CARTESIAN_POINT('',(17.94525,-65.9999999999999,37.5459252805377));
#15315=CARTESIAN_POINT('',(21.8174278887595,-65.0413794120408,25.));
#15316=CARTESIAN_POINT('Ctrl Pts',(17.9470733560714,-66.0015060535927,25.2959252805377));
#15317=CARTESIAN_POINT('Ctrl Pts',(17.9500635199578,-65.5475809519615,25.2713722656862));
#15318=CARTESIAN_POINT('Ctrl Pts',(18.3216912761193,-64.4040176334961,25.2097748781708));
#15319=CARTESIAN_POINT('Ctrl Pts',(20.2159939907177,-63.5820409220313,25.1111331179916));
#15320=CARTESIAN_POINT('Ctrl Pts',(21.4986774253636,-64.4370673526013,25.0370443726639));
#15321=CARTESIAN_POINT('Ctrl Pts',(21.8174278887595,-65.0413794120408,25.));
#15322=CARTESIAN_POINT('',(22.0570978924847,-66.0754551987761,25.));
#15323=CARTESIAN_POINT('Origin',(20.,-66.,25.));
#15324=CARTESIAN_POINT('Ctrl Pts',(17.9445921681644,-65.9981769380503,25.3540747194623));
#15325=CARTESIAN_POINT('Ctrl Pts',(17.943297586139,-65.8578134130738,25.3464567039117));
#15326=CARTESIAN_POINT('Ctrl Pts',(18.0204259142703,-65.0363089952078,25.3017943156971));
#15327=CARTESIAN_POINT('Ctrl Pts',(19.1263754391461,-63.7340406632385,25.2200875548188));
#15328=CARTESIAN_POINT('Ctrl Pts',(21.4138493882471,-64.0348872703216,25.109680663882));
#15329=CARTESIAN_POINT('Ctrl Pts',(22.0806819706411,-65.4089772617309,25.0363181456091));
#15330=CARTESIAN_POINT('Ctrl Pts',(22.0571001480269,-66.0754553928761,25.));
#15331=CARTESIAN_POINT('Origin',(20.,-66.,37.5459252805377));
#15332=CARTESIAN_POINT('',(17.9485832974788,-66.0000495918166,26.0540747194623));
#15333=CARTESIAN_POINT('',(17.9419861288051,-66.0004830914585,25.9959252805377));
#15334=CARTESIAN_POINT('',(17.94525,-65.9999999999999,37.5459252805377));
#15335=CARTESIAN_POINT('Ctrl Pts',(17.9419861288051,-66.0004830914585,25.9959252805377));
#15336=CARTESIAN_POINT('Ctrl Pts',(17.9440551582811,-65.3463924174249,25.9603051683359));
#15337=CARTESIAN_POINT('Ctrl Pts',(18.6350687960196,-64.0082840246707,25.8876406834704));
#15338=CARTESIAN_POINT('Ctrl Pts',(20.9141747077605,-63.7500129462385,25.7779318259409));
#15339=CARTESIAN_POINT('Ctrl Pts',(22.3860296230922,-65.5475930706263,25.6667987079494));
#15340=CARTESIAN_POINT('Ctrl Pts',(21.6743955907743,-67.7593785514666,25.5556655899578));
#15341=CARTESIAN_POINT('Ctrl Pts',(19.429692000846,-68.3606229571339,25.4445324719662));
#15342=CARTESIAN_POINT('Ctrl Pts',(18.0884943176257,-67.1462799502129,25.3579523688262));
#15343=CARTESIAN_POINT('Ctrl Pts',(17.9455521087929,-66.2324406617768,25.30841663835));
#15344=CARTESIAN_POINT('Ctrl Pts',(17.9470733560714,-66.0015060535927,25.2959252805377));
#15345=CARTESIAN_POINT('Ctrl Pts',(17.9485832974788,-66.0000495918166,26.0540747194623));
#15346=CARTESIAN_POINT('Ctrl Pts',(17.9486573139036,-65.6541000235851,26.0353896065614));
#15347=CARTESIAN_POINT('Ctrl Pts',(18.1957460549727,-64.6221845951523,25.9796601209967));
#15348=CARTESIAN_POINT('Ctrl Pts',(19.829859942873,-63.5773515961876,25.8868862627681));
#15349=CARTESIAN_POINT('Ctrl Pts',(21.9430509240163,-64.5430603155101,25.7757531447765));
#15350=CARTESIAN_POINT('Ctrl Pts',(22.2779267364902,-66.8422110789462,25.664620026785));
#15351=CARTESIAN_POINT('Ctrl Pts',(20.5278715823273,-68.3705500709468,25.5534869087934));
#15352=CARTESIAN_POINT('Ctrl Pts',(18.4479228041263,-67.7732032161842,25.4499718063526));
#15353=CARTESIAN_POINT('Ctrl Pts',(17.949592792374,-66.5403637036397,25.3835010765755));
#15354=CARTESIAN_POINT('Ctrl Pts',(17.9445921681644,-65.9981769380503,25.3540747194623));
#15355=CARTESIAN_POINT('Origin',(20.,-66.,37.5459252805377));
#15356=CARTESIAN_POINT('',(17.9444688958667,-66.0018063311818,26.7540747194623));
#15357=CARTESIAN_POINT('',(17.9457762375739,-65.9981345160027,26.6959252805377));
#15358=CARTESIAN_POINT('',(17.94525,-65.9999999999999,37.5459252805377));
#15359=CARTESIAN_POINT('Ctrl Pts',(17.9457762375739,-65.9981345160027,26.6959252805377));
#15360=CARTESIAN_POINT('Ctrl Pts',(17.9441911203672,-65.8202139891171,26.6862824436496));
#15361=CARTESIAN_POINT('Ctrl Pts',(18.0468091802697,-64.9605854820692,26.6395952340976));
#15362=CARTESIAN_POINT('Ctrl Pts',(19.2507941167209,-63.6898347424764,26.5558636518818));
#15363=CARTESIAN_POINT('Ctrl Pts',(21.5344924336398,-64.1175798748589,26.4447305338903));
#15364=CARTESIAN_POINT('Ctrl Pts',(22.4137604897707,-66.2681888420218,26.3335974158987));
#15365=CARTESIAN_POINT('Ctrl Pts',(21.0838647034058,-68.1733431282881,26.2224642979072));
#15366=CARTESIAN_POINT('Ctrl Pts',(18.7619637841276,-68.0893636493551,26.1113311799156));
#15367=CARTESIAN_POINT('Ctrl Pts',(17.9542069036107,-66.7329548013126,26.0358181741258));
#15368=CARTESIAN_POINT('Ctrl Pts',(17.9419033992264,-66.0266367284935,25.9973495409998));
#15369=CARTESIAN_POINT('Ctrl Pts',(17.9419861288051,-66.0004830914585,25.9959252805377));
#15370=CARTESIAN_POINT('Ctrl Pts',(17.9444688958667,-66.0018063311818,26.7540747194623));
#15371=CARTESIAN_POINT('Ctrl Pts',(17.9494993134766,-65.4537400361145,26.7243225092112));
#15372=CARTESIAN_POINT('Ctrl Pts',(18.4568950033307,-64.2150556037813,26.6575259262963));
#15373=CARTESIAN_POINT('Ctrl Pts',(20.5486976238089,-63.6341805685774,26.5536849707175));
#15374=CARTESIAN_POINT('Ctrl Pts',(22.2852057058799,-65.1778050816215,26.4425518527259));
#15375=CARTESIAN_POINT('Ctrl Pts',(21.9302042425984,-67.4739346416768,26.3314187347344));
#15376=CARTESIAN_POINT('Ctrl Pts',(19.8086025657231,-68.4210614106236,26.2202856167428));
#15377=CARTESIAN_POINT('Ctrl Pts',(18.1894356332652,-67.3656511409621,26.1278376116521));
#15378=CARTESIAN_POINT('Ctrl Pts',(17.9485105718401,-66.3399660815773,26.0724339792253));
#15379=CARTESIAN_POINT('Ctrl Pts',(17.9485832974788,-66.0000495918166,26.0540747194623));
#15380=CARTESIAN_POINT('Origin',(20.,-66.,37.5459252805377));
#15381=CARTESIAN_POINT('',(17.9427073981771,-65.9988171298974,27.4540747194623));
#15382=CARTESIAN_POINT('',(17.948391336186,-66.000651392518,27.3959252805377));
#15383=CARTESIAN_POINT('',(17.94525,-65.9999999999999,37.5459252805377));
#15384=CARTESIAN_POINT('Ctrl Pts',(17.948391336186,-66.000651392518,27.3959252805377));
#15385=CARTESIAN_POINT('Ctrl Pts',(17.9494813643374,-65.6173024424008,27.3752153462994));
#15386=CARTESIAN_POINT('Ctrl Pts',(18.2366610904736,-64.5467312444963,27.3174610393972));
#15387=CARTESIAN_POINT('Ctrl Pts',(19.9621345918737,-63.5716800154371,27.2226623598312));
#15388=CARTESIAN_POINT('Ctrl Pts',(22.0195745014619,-64.6511150583807,27.1115292418397));
#15389=CARTESIAN_POINT('Ctrl Pts',(22.2286202996251,-66.9651026731069,27.000396123848));
#15390=CARTESIAN_POINT('Ctrl Pts',(20.3979451577182,-68.3957903719854,26.8892630058565));
#15391=CARTESIAN_POINT('Ctrl Pts',(18.3935018010201,-67.6998767838394,26.787772724753));
#15392=CARTESIAN_POINT('Ctrl Pts',(17.9502805806786,-66.5037217969321,26.7233268163134));
#15393=CARTESIAN_POINT('Ctrl Pts',(17.9457762375739,-65.9981345160027,26.6959252805377));
#15394=CARTESIAN_POINT('Ctrl Pts',(17.9427073981771,-65.9988171298974,27.4540747194623));
#15395=CARTESIAN_POINT('Ctrl Pts',(17.9422312044669,-65.9294336928593,27.4502997845249));
#15396=CARTESIAN_POINT('Ctrl Pts',(17.9768968646083,-65.1796548342728,27.4094804769236));
#15397=CARTESIAN_POINT('Ctrl Pts',(18.8966146957805,-63.836504826525,27.3316167966584));
#15398=CARTESIAN_POINT('Ctrl Pts',(21.219169386089,-63.8995723038675,27.2204836786668));
#15399=CARTESIAN_POINT('Ctrl Pts',(22.4258922629222,-65.8850338815669,27.1093505606752));
#15400=CARTESIAN_POINT('Ctrl Pts',(21.41234306908,-67.9757169742283,26.9982174426837));
#15401=CARTESIAN_POINT('Ctrl Pts',(19.1061618881228,-68.2581461319033,26.8870843246921));
#15402=CARTESIAN_POINT('Ctrl Pts',(18.0164474647602,-66.9515223045583,26.8057034169517));
#15403=CARTESIAN_POINT('Ctrl Pts',(17.9432359581487,-66.1361354584251,26.7613668818751));
#15404=CARTESIAN_POINT('Ctrl Pts',(17.9444688958667,-66.0018063311818,26.7540747194623));
#15405=CARTESIAN_POINT('Origin',(20.,-66.,37.5459252805377));
#15406=CARTESIAN_POINT('',(17.9480454330843,-65.9989448752678,28.1540747194623));
#15407=CARTESIAN_POINT('',(17.9433900806158,-66.0015207493092,28.0959252805377));
#15408=CARTESIAN_POINT('',(17.94525,-65.9999999999999,37.5459252805377));
#15409=CARTESIAN_POINT('Ctrl Pts',(17.9433900806158,-66.0015207493092,28.0959252805377));
#15410=CARTESIAN_POINT('Ctrl Pts',(17.9482332143848,-65.416949847134,28.0641482489491));
#15411=CARTESIAN_POINT('Ctrl Pts',(18.5151173764583,-64.1426999291749,27.9953268446968));
#15412=CARTESIAN_POINT('Ctrl Pts',(20.676812844959,-63.6675986416085,27.8894610677805));
#15413=CARTESIAN_POINT('Ctrl Pts',(22.3266174994283,-65.3035642630666,27.778327949789));
#15414=CARTESIAN_POINT('Ctrl Pts',(21.8470102430435,-67.576935282117,27.6671948317974));
#15415=CARTESIAN_POINT('Ctrl Pts',(19.6769465158166,-68.4070330639894,27.5560617138059));
#15416=CARTESIAN_POINT('Ctrl Pts',(18.1518517698952,-67.2899653282545,27.4656385300526));
#15417=CARTESIAN_POINT('Ctrl Pts',(17.9475316039668,-66.3030082107063,27.4122597189632));
#15418=CARTESIAN_POINT('Ctrl Pts',(17.948391336186,-66.000651392518,27.3959252805377));
#15419=CARTESIAN_POINT('Ctrl Pts',(17.9480454330843,-65.9989448752678,28.1540747194623));
#15420=CARTESIAN_POINT('Ctrl Pts',(17.946767622487,-65.7243289514539,28.1392326871746));
#15421=CARTESIAN_POINT('Ctrl Pts',(18.1259279022936,-64.7658953828094,28.0873462822231));
#15422=CARTESIAN_POINT('Ctrl Pts',(19.580500984485,-63.6078898290281,27.9984155046077));
#15423=CARTESIAN_POINT('Ctrl Pts',(21.7821628698452,-64.3501315205369,27.8872823866162));
#15424=CARTESIAN_POINT('Ctrl Pts',(22.3527191513918,-66.6023977826542,27.7761492686246));
#15425=CARTESIAN_POINT('Ctrl Pts',(20.7699742636292,-68.3033258839143,27.6650161506331));
#15426=CARTESIAN_POINT('Ctrl Pts',(18.560218200161,-67.9099899791605,27.5576579675789));
#15427=CARTESIAN_POINT('Ctrl Pts',(17.9469042114332,-66.6103105664805,27.4873441571887));
#15428=CARTESIAN_POINT('Ctrl Pts',(17.9427073981771,-65.9988171298974,27.4540747194623));
#15429=CARTESIAN_POINT('Origin',(20.,-66.,37.5459252805377));
#15430=CARTESIAN_POINT('',(17.9465563505173,-66.0017537138358,28.8540747194623));
#15431=CARTESIAN_POINT('',(17.9436613428911,-65.998383858391,28.7959252805377));
#15432=CARTESIAN_POINT('',(17.94525,-65.9999999999999,37.5459252805377));
#15433=CARTESIAN_POINT('Ctrl Pts',(17.9436613428911,-65.998383858391,28.7959252805377));
#15434=CARTESIAN_POINT('Ctrl Pts',(17.9427401993079,-65.8916548076745,28.7901255242628));
#15435=CARTESIAN_POINT('Ctrl Pts',(17.99882477166,-65.1041931740386,28.747281395324));
#15436=CARTESIAN_POINT('Ctrl Pts',(19.0161588486977,-63.7795882560541,28.6673928937214));
#15437=CARTESIAN_POINT('Ctrl Pts',(21.3318252735703,-63.9691348729347,28.5562597757299));
#15438=CARTESIAN_POINT('Ctrl Pts',(22.4285527879442,-66.0174091881803,28.4451266577383));
#15439=CARTESIAN_POINT('Ctrl Pts',(21.3025732038757,-68.0497499291796,28.3339935397468));
#15440=CARTESIAN_POINT('Ctrl Pts',(18.9844273548577,-68.2060788576321,28.2228604217552));
#15441=CARTESIAN_POINT('Ctrl Pts',(17.9928405779599,-66.8759493052599,28.1435043353522));
#15442=CARTESIAN_POINT('Ctrl Pts',(17.9425872857618,-66.0984188600057,28.101192621613));
#15443=CARTESIAN_POINT('Ctrl Pts',(17.9433900806158,-66.0015207493092,28.0959252805377));
#15444=CARTESIAN_POINT('Ctrl Pts',(17.9465563505173,-66.0017537138358,28.8540747194623));
#15445=CARTESIAN_POINT('Ctrl Pts',(17.9504440938478,-65.5232420995012,28.8281655898244));
#15446=CARTESIAN_POINT('Ctrl Pts',(18.355544098096,-64.3546301779743,28.7652120875227));
#15447=CARTESIAN_POINT('Ctrl Pts',(20.3013690653653,-63.5901561916745,28.6652142125571));
#15448=CARTESIAN_POINT('Ctrl Pts',(22.188046145667,-64.9461382640413,28.5540810945655));
#15449=CARTESIAN_POINT('Ctrl Pts',(22.0721372727958,-67.2666560767515,28.442947976574));
#15450=CARTESIAN_POINT('Ctrl Pts',(20.0597268093363,-68.4278803929209,28.3318148585824));
#15451=CARTESIAN_POINT('Ctrl Pts',(18.2687136588368,-67.5086938026241,28.2355237728786));
#15452=CARTESIAN_POINT('Ctrl Pts',(17.9499569223782,-66.4097455051991,28.1762770598385));
#15453=CARTESIAN_POINT('Ctrl Pts',(17.9480454330843,-65.9989448752678,28.1540747194623));
#15454=CARTESIAN_POINT('Origin',(20.,-66.,37.5459252805377));
#15455=CARTESIAN_POINT('',(17.9418459383603,-66.0000233771323,29.5540747194623));
#15456=CARTESIAN_POINT('',(17.9484736511709,-65.9995028191367,29.4959252805377));
#15457=CARTESIAN_POINT('',(17.94525,-65.9999999999999,37.5459252805377));
#15458=CARTESIAN_POINT('Ctrl Pts',(17.9484736511709,-65.9995028191366,29.4959252805377));
#15459=CARTESIAN_POINT('Ctrl Pts',(17.9477976021827,-65.6872595106289,29.4790584269126));
#15460=CARTESIAN_POINT('Ctrl Pts',(18.1614619143335,-64.6901194629804,29.4251472006236));
#15461=CARTESIAN_POINT('Ctrl Pts',(19.7114877884649,-63.5885829005652,29.3341916016708));
#15462=CARTESIAN_POINT('Ctrl Pts',(21.869427923728,-64.4497061692577,29.2230584836792));
#15463=CARTESIAN_POINT('Ctrl Pts',(22.3163940432292,-66.7297193708161,29.1119253656877));
#15464=CARTESIAN_POINT('Ctrl Pts',(20.6433051619858,-68.3418646827291,29.0007922476961));
#15465=CARTESIAN_POINT('Ctrl Pts',(18.4994791972086,-67.8383663641301,28.8954588859795));
#15466=CARTESIAN_POINT('Ctrl Pts',(17.9486237545051,-66.5733577174882,28.8271698969266));
#15467=CARTESIAN_POINT('Ctrl Pts',(17.9436613428911,-65.998383858391,28.7959252805377));
#15468=CARTESIAN_POINT('Ctrl Pts',(17.9418460670015,-66.0000233762489,29.5540747194623));
#15469=CARTESIAN_POINT('Ctrl Pts',(17.9419602237683,-65.3211542896944,29.5170984924742));
#15470=CARTESIAN_POINT('Ctrl Pts',(18.6804457109671,-63.9619521942107,29.4430778928223));
#15471=CARTESIAN_POINT('Ctrl Pts',(20.9956693404756,-63.7848672593903,29.3320129205065));
#15472=CARTESIAN_POINT('Ctrl Pts',(22.4010377426051,-65.6350503422798,29.2208798025149));
#15473=CARTESIAN_POINT('Ctrl Pts',(21.6088818987778,-67.8192497161933,29.1097466845234));
#15474=CARTESIAN_POINT('Ctrl Pts',(19.3442140162146,-68.3384001448757,28.9986135665318));
#15475=CARTESIAN_POINT('Ctrl Pts',(18.0677943807432,-67.0952787540644,28.9133895781781));
#15476=CARTESIAN_POINT('Ctrl Pts',(17.9448854735943,-66.2074087547744,28.8652099624883));
#15477=CARTESIAN_POINT('Ctrl Pts',(17.9465563505173,-66.0017537138358,28.8540747194623));
#15478=CARTESIAN_POINT('Origin',(20.,-66.,37.5459252805377));
#15479=CARTESIAN_POINT('',(17.9464881988838,-65.9982315277441,30.2540747194623));
#15480=CARTESIAN_POINT('',(17.9454841446209,-66.0018778869456,30.1959252805377));
#15481=CARTESIAN_POINT('',(17.94525,-65.9999999999999,37.5459252805377));
#15482=CARTESIAN_POINT('Ctrl Pts',(17.9454841446209,-66.0018778869456,30.1959252805377));
#15483=CARTESIAN_POINT('Ctrl Pts',(17.9501627255122,-65.4866536541329,30.1679913295624));
#15484=CARTESIAN_POINT('Ctrl Pts',(18.4074704960921,-64.280766173597,30.1030130059232));
#15485=CARTESIAN_POINT('Ctrl Pts',(20.432251111771,-63.6101609468367,30.0009903096202));
#15486=CARTESIAN_POINT('Ctrl Pts',(22.24222733538,-65.0669467860159,29.8898571916286));
#15487=CARTESIAN_POINT('Ctrl Pts',(22.0000288484413,-67.3776996512498,29.7787240736371));
#15488=CARTESIAN_POINT('Ctrl Pts',(19.9273252390408,-68.4275275699302,29.6675909556455));
#15489=CARTESIAN_POINT('Ctrl Pts',(18.2256189616023,-67.4334540757706,29.573324691279));
#15490=CARTESIAN_POINT('Ctrl Pts',(17.9492823966329,-66.3730339733265,29.5161027995764));
#15491=CARTESIAN_POINT('Ctrl Pts',(17.9484736511709,-65.9995028191366,29.4959252805377));
#15492=CARTESIAN_POINT('Ctrl Pts',(17.9464881988838,-65.9982315277441,30.2540747194623));
#15493=CARTESIAN_POINT('Ctrl Pts',(17.9448198460957,-65.7951106883291,30.2430757677879));
#15494=CARTESIAN_POINT('Ctrl Pts',(18.0658216378279,-64.9098243930965,30.1950324434495));
#15495=CARTESIAN_POINT('Ctrl Pts',(19.3356364183429,-63.6640223619538,30.1099447464474));
#15496=CARTESIAN_POINT('Ctrl Pts',(21.6021943503792,-64.1748578801372,29.9988116284558));
#15497=CARTESIAN_POINT('Ctrl Pts',(22.4023609511933,-66.3561353033128,29.8876785104642));
#15498=CARTESIAN_POINT('Ctrl Pts',(21.0037922534698,-68.2114636795477,29.7765453924727));
#15499=CARTESIAN_POINT('Ctrl Pts',(18.6865133764925,-68.0427734538981,29.6654122744811));
#15500=CARTESIAN_POINT('Ctrl Pts',(17.9424134466727,-66.6826456501542,29.5912553834777));
#15501=CARTESIAN_POINT('Ctrl Pts',(17.9418458566153,-66.0012745042416,29.5541428651381));
#15502=CARTESIAN_POINT('Ctrl Pts',(17.9418460670015,-66.0000233762489,29.5540747194623));
#15503=CARTESIAN_POINT('Origin',(20.,-66.,37.5459252805377));
#15504=CARTESIAN_POINT('',(17.9480838467249,-66.0010204151978,30.9540747194623));
#15505=CARTESIAN_POINT('',(17.9420998107195,-65.9993455607918,30.8959252805377));
#15506=CARTESIAN_POINT('',(17.94525,-65.9999999999999,37.5459252805377));
#15507=CARTESIAN_POINT('Ctrl Pts',(17.9420998107195,-65.9993455607918,30.8959252805377));
#15508=CARTESIAN_POINT('Ctrl Pts',(17.9419500148889,-65.963409877897,30.893968604876));
#15509=CARTESIAN_POINT('Ctrl Pts',(17.9590877394987,-65.2472748400191,30.8549675565505));
#15510=CARTESIAN_POINT('Ctrl Pts',(18.7920501950665,-63.8930996719321,30.7789221355611));
#15511=CARTESIAN_POINT('Ctrl Pts',(21.1149084550803,-63.8424201381079,30.6677890175695));
#15512=CARTESIAN_POINT('Ctrl Pts',(22.4173586146354,-65.7664426154033,30.556655899578));
#15513=CARTESIAN_POINT('Ctrl Pts',(21.5073470237683,-67.9042260038106,30.4455227815864));
#15514=CARTESIAN_POINT('Ctrl Pts',(19.2177521081477,-68.2991868039253,30.3343896635948));
#15515=CARTESIAN_POINT('Ctrl Pts',(18.0396474822591,-67.0194951979082,30.2511904965786));
#15516=CARTESIAN_POINT('Ctrl Pts',(17.9439582650609,-66.1699139098205,30.2050357022262));
#15517=CARTESIAN_POINT('Ctrl Pts',(17.9454841446209,-66.0018778869456,30.1959252805377));
#15518=CARTESIAN_POINT('Ctrl Pts',(17.948083846725,-66.0010204151978,30.9540747194623));
#15519=CARTESIAN_POINT('Ctrl Pts',(17.9499190751742,-65.5927223975328,30.9320086704377));
#15520=CARTESIAN_POINT('Ctrl Pts',(18.2657185825361,-64.4963599216305,30.8728982487491));
#15521=CARTESIAN_POINT('Ctrl Pts',(20.0508159969719,-63.5719167583182,30.7767434543967));
#15522=CARTESIAN_POINT('Ctrl Pts',(22.0674746434876,-64.7257476338574,30.6656103364051));
#15523=CARTESIAN_POINT('Ctrl Pts',(22.1918991212745,-67.0458244289748,30.5544772184136));
#15524=CARTESIAN_POINT('Ctrl Pts',(20.3102112509622,-68.4087215434459,30.443344100422));
#15525=CARTESIAN_POINT('Ctrl Pts',(18.3589378869015,-67.6503617606642,30.343209934105));
#15526=CARTESIAN_POINT('Ctrl Pts',(17.9504388436372,-66.4792198919863,30.2801201404517));
#15527=CARTESIAN_POINT('Ctrl Pts',(17.9464881988838,-65.9982315277441,30.2540747194623));
#15528=CARTESIAN_POINT('Origin',(20.,-66.,37.5459252805377));
#15529=CARTESIAN_POINT('',(17.942763982448,-66.0012177326012,31.6540747194623));
#15530=CARTESIAN_POINT('',(17.9474132556182,-65.9985364755177,31.5959252805377));
#15531=CARTESIAN_POINT('',(17.94525,-65.9999999999999,37.5459252805377));
#15532=CARTESIAN_POINT('Ctrl Pts',(17.9474132556182,-65.9985364755177,31.5959252805377));
#15533=CARTESIAN_POINT('Ctrl Pts',(17.945828170814,-65.7577490840029,31.5829015075258));
#15534=CARTESIAN_POINT('Ctrl Pts',(18.0963189994412,-64.8339923197765,31.53283336185));
#15535=CARTESIAN_POINT('Ctrl Pts',(19.4639280160152,-63.6312875751501,31.4457208435104));
#15536=CARTESIAN_POINT('Ctrl Pts',(21.6992787653883,-64.2648851907865,31.3345877255189));
#15537=CARTESIAN_POINT('Ctrl Pts',(22.3793827057175,-66.4865281732684,31.2234546075273));
#15538=CARTESIAN_POINT('Ctrl Pts',(20.8817819421834,-68.2628814220129,31.1123214895357));
#15539=CARTESIAN_POINT('Ctrl Pts',(18.6177165393643,-67.9733456286802,31.0031450472059));
#15540=CARTESIAN_POINT('Ctrl Pts',(17.9447859946471,-66.643755044526,30.9310129775399));
#15541=CARTESIAN_POINT('Ctrl Pts',(17.9420998107195,-65.9993455607918,30.8959252805377));
#15542=CARTESIAN_POINT('Ctrl Pts',(17.942763982448,-66.0012177326012,31.6540747194623));
#15543=CARTESIAN_POINT('Ctrl Pts',(17.9470404258716,-65.392185277657,31.6209415730874));
#15544=CARTESIAN_POINT('Ctrl Pts',(18.5560216000726,-64.0947973033485,31.5507640540487));
#15545=CARTESIAN_POINT('Ctrl Pts',(20.7615157875532,-63.6938637942672,31.4435421623461));
#15546=CARTESIAN_POINT('Ctrl Pts',(22.3504924848334,-65.3889717086535,31.3324090443545));
#15547=CARTESIAN_POINT('Ctrl Pts',(21.7882059455114,-67.6433167651191,31.221275926363));
#15548=CARTESIAN_POINT('Ctrl Pts',(19.5892829417572,-68.3936336378304,31.1101428083714));
#15549=CARTESIAN_POINT('Ctrl Pts',(18.128234020465,-67.2392077048223,31.0210757394045));
#15550=CARTESIAN_POINT('Ctrl Pts',(17.9468381028388,-66.2781710660904,30.9690530431015));
#15551=CARTESIAN_POINT('Ctrl Pts',(17.948083846725,-66.0010204151978,30.9540747194623));
#15552=CARTESIAN_POINT('Origin',(20.,-66.,37.5459252805377));
#15553=CARTESIAN_POINT('',(17.9443932527679,-65.998206175835,32.3540747194623));
#15554=CARTESIAN_POINT('',(17.9473846863418,-66.0014769892929,32.2959252805377));
#15555=CARTESIAN_POINT('',(17.94525,-65.9999999999999,37.5459252805377));
#15556=CARTESIAN_POINT('Ctrl Pts',(17.9473846863418,-66.001476989293,32.2959252805377));
#15557=CARTESIAN_POINT('Ctrl Pts',(17.9503463410227,-65.5560933942008,32.2718344101756));
#15558=CARTESIAN_POINT('Ctrl Pts',(18.3116444429935,-64.4214700752732,32.2106991671496));
#15559=CARTESIAN_POINT('Ctrl Pts',(20.1830643580926,-63.5782941622798,32.1125195514598));
#15560=CARTESIAN_POINT('Ctrl Pts',(22.1338456839189,-64.8403128349112,32.0013864334682));
#15561=CARTESIAN_POINT('Ctrl Pts',(22.131647452475,-67.1637228458735,31.8902533154766));
#15562=CARTESIAN_POINT('Ctrl Pts',(20.1784815716998,-68.4220479046079,31.7791201974851));
#15563=CARTESIAN_POINT('Ctrl Pts',(18.309998800391,-67.5759383428421,31.6810108525054));
#15564=CARTESIAN_POINT('Ctrl Pts',(17.9503367315926,-66.442636470775,31.6199458801896));
#15565=CARTESIAN_POINT('Ctrl Pts',(17.9474132556182,-65.9985364755177,31.5959252805377));
#15566=CARTESIAN_POINT('Ctrl Pts',(17.9443932527679,-65.998206175835,32.3540747194623));
#15567=CARTESIAN_POINT('Ctrl Pts',(17.9431868124194,-65.8664001702729,32.3469188484011));
#15568=CARTESIAN_POINT('Ctrl Pts',(18.0147856257919,-65.0535688820171,32.302718604676));
#15569=CARTESIAN_POINT('Ctrl Pts',(19.0978804403178,-63.7451494962803,32.221473988287));
#15570=CARTESIAN_POINT('Ctrl Pts',(21.4050825978426,-64.0191129796669,32.1103408702954));
#15571=CARTESIAN_POINT('Ctrl Pts',(22.4262978583092,-66.1060622310153,31.9992077523039));
#15572=CARTESIAN_POINT('Ctrl Pts',(21.2268698206984,-68.0959391539699,31.8880746343123));
#15573=CARTESIAN_POINT('Ctrl Pts',(18.9045622340586,-68.16753006785,31.7769415163208));
#15574=CARTESIAN_POINT('Ctrl Pts',(17.9783027092024,-66.8254193993548,31.6989415447041));
#15575=CARTESIAN_POINT('Ctrl Pts',(17.9422591665831,-66.0731114103599,31.6579859457513));
#15576=CARTESIAN_POINT('Ctrl Pts',(17.942763982448,-66.0012177326012,31.6540747194623));
#15577=CARTESIAN_POINT('Origin',(20.,-66.,37.5459252805377));
#15578=CARTESIAN_POINT('',(17.9485813153775,-65.9999091152646,33.0540747194623));
#15579=CARTESIAN_POINT('',(17.9420826989354,-66.0006320364587,32.9959252805377));
#15580=CARTESIAN_POINT('',(17.94525,-65.9999999999999,37.5459252805377));
#15581=CARTESIAN_POINT('Ctrl Pts',(17.9420826989354,-66.0006320364586,32.9959252805377));
#15582=CARTESIAN_POINT('Ctrl Pts',(17.9446925638124,-65.3549462988232,32.9607673128254));
#15583=CARTESIAN_POINT('Ctrl Pts',(18.6199954646792,-64.0242258864647,32.8885649724491));
#15584=CARTESIAN_POINT('Ctrl Pts',(20.8860622876183,-63.7387911759138,32.7793182594092));
#15585=CARTESIAN_POINT('Ctrl Pts',(22.3802990759988,-65.5179750707177,32.6681851414176));
#15586=CARTESIAN_POINT('Ctrl Pts',(21.6959924623663,-67.7383271531118,32.5570520234261));
#15587=CARTESIAN_POINT('Ctrl Pts',(19.4594467935634,-68.3676938050906,32.4459189054344));
#15588=CARTESIAN_POINT('Ctrl Pts',(18.09521740236,-67.1633756303953,32.358876657805));
#15589=CARTESIAN_POINT('Ctrl Pts',(17.945792224129,-66.2409568145323,32.3088787828394));
#15590=CARTESIAN_POINT('Ctrl Pts',(17.9473846863418,-66.001476989293,32.2959252805377));
#15591=CARTESIAN_POINT('Ctrl Pts',(17.9485813153775,-65.9999091152646,33.0540747194623));
#15592=CARTESIAN_POINT('Ctrl Pts',(17.9484481885224,-65.6625170236538,33.0358517510509));
#15593=CARTESIAN_POINT('Ctrl Pts',(18.1868160730737,-64.6394380396369,32.9805844099755));
#15594=CARTESIAN_POINT('Ctrl Pts',(19.7997192052125,-63.5796574421335,32.8882726962363));
#15595=CARTESIAN_POINT('Ctrl Pts',(21.9247814806566,-64.5189913079908,32.7771395782448));
#15596=CARTESIAN_POINT('Ctrl Pts',(22.2882079863162,-66.8138026206755,32.6660064602532));
#15597=CARTESIAN_POINT('Ctrl Pts',(20.5573764799239,-68.3637897439758,32.5548733422617));
#15598=CARTESIAN_POINT('Ctrl Pts',(18.4607079720781,-67.7898433151808,32.4508960953314));
#15599=CARTESIAN_POINT('Ctrl Pts',(17.9494322891033,-66.5487309092672,32.3839632210649));
#15600=CARTESIAN_POINT('Ctrl Pts',(17.9443932527679,-65.998206175835,32.3540747194623));
#15601=CARTESIAN_POINT('Origin',(20.,-66.,37.5459252805377));
#15602=CARTESIAN_POINT('',(17.9447268179648,-66.0018413363536,33.7540747194623));
#15603=CARTESIAN_POINT('',(17.9455229696729,-65.9981228934317,33.6959252805377));
#15604=CARTESIAN_POINT('',(17.94525,-65.9999999999999,37.5459252805377));
#15605=CARTESIAN_POINT('Ctrl Pts',(17.9455229696729,-65.9981228934317,33.6959252805377));
#15606=CARTESIAN_POINT('Ctrl Pts',(17.9439884886147,-65.8287826079759,33.686744588139));
#15607=CARTESIAN_POINT('Ctrl Pts',(18.0405830452216,-64.9778761146953,33.6405195230764));
#15608=CARTESIAN_POINT('Ctrl Pts',(19.2221041313598,-63.699337108691,33.55725008535));
#15609=CARTESIAN_POINT('Ctrl Pts',(21.5109475856345,-64.0986296736855,33.4461169673585));
#15610=CARTESIAN_POINT('Ctrl Pts',(22.4169123392658,-66.2381311992,33.3349838493669));
#15611=CARTESIAN_POINT('Ctrl Pts',(21.110823791235,-68.1596856781178,33.2238507313754));
#15612=CARTESIAN_POINT('Ctrl Pts',(18.7880655878792,-68.1046108201909,33.1127176133838));
#15613=CARTESIAN_POINT('Ctrl Pts',(17.9584343935882,-66.7501147046579,33.0367424631046));
#15614=CARTESIAN_POINT('Ctrl Pts',(17.9419426663241,-66.035276381734,32.9978116854892));
#15615=CARTESIAN_POINT('Ctrl Pts',(17.9420826989354,-66.0006320364586,32.9959252805377));
#15616=CARTESIAN_POINT('Ctrl Pts',(17.9447268179648,-66.0018413363536,33.7540747194623));
#15617=CARTESIAN_POINT('Ctrl Pts',(17.9497081022268,-65.4621140562523,33.7247846537006));
#15618=CARTESIAN_POINT('Ctrl Pts',(18.4440788696627,-64.23169580166,33.6584502152751));
#15619=CARTESIAN_POINT('Ctrl Pts',(20.5192141319096,-63.6275356306401,33.5550714041857));
#15620=CARTESIAN_POINT('Ctrl Pts',(22.2747973195027,-65.14943098434,33.4439382861942));
#15621=CARTESIAN_POINT('Ctrl Pts',(21.9483964634611,-67.4498005771448,33.3328051682026));
#15622=CARTESIAN_POINT('Ctrl Pts',(19.838746476763,-68.4232556192041,33.221672050211));
#15623=CARTESIAN_POINT('Ctrl Pts',(18.1984100797459,-67.382901918355,33.1287619006309));
#15624=CARTESIAN_POINT('Ctrl Pts',(17.9487188140715,-66.3483810438974,33.0728961237147));
#15625=CARTESIAN_POINT('Ctrl Pts',(17.9485813153775,-65.9999091152646,33.0540747194623));
#15626=CARTESIAN_POINT('Origin',(20.,-66.,37.5459252805377));
#15627=CARTESIAN_POINT('',(17.9425257907963,-65.9989407170969,34.4540747194623));
#15628=CARTESIAN_POINT('',(17.9484640666104,-66.0005177854496,34.3959252805377));
#15629=CARTESIAN_POINT('',(17.94525,-65.9999999999999,37.5459252805377));
#15630=CARTESIAN_POINT('Ctrl Pts',(17.9484640666104,-66.0005177854496,34.3959252805377));
#15631=CARTESIAN_POINT('Ctrl Pts',(17.9493094487375,-65.6256901243484,34.3756774907888));
#15632=CARTESIAN_POINT('Ctrl Pts',(18.2270646452969,-64.5639295218498,34.318385328376));
#15633=CARTESIAN_POINT('Ctrl Pts',(19.9319188455824,-63.5723392811283,34.2240487932994));
#15634=CARTESIAN_POINT('Ctrl Pts',(22.0026322110525,-64.6260873463218,34.1129156753078));
#15635=CARTESIAN_POINT('Ctrl Pts',(22.2404577570769,-66.9372943909543,34.0017825573163));
#15636=CARTESIAN_POINT('Ctrl Pts',(20.4277281787894,-68.3906526963146,33.8906494393247));
#15637=CARTESIAN_POINT('Ctrl Pts',(18.4056138794515,-67.7166818294076,33.7886970137319));
#15638=CARTESIAN_POINT('Ctrl Pts',(17.9501801662898,-66.5120758029774,33.7237889608029));
#15639=CARTESIAN_POINT('Ctrl Pts',(17.9455229696729,-65.9981228934317,33.6959252805377));
#15640=CARTESIAN_POINT('Ctrl Pts',(17.9425257907963,-65.9989407170969,34.4540747194623));
#15641=CARTESIAN_POINT('Ctrl Pts',(17.9421433932643,-65.9380656633799,34.4507619290143));
#15642=CARTESIAN_POINT('Ctrl Pts',(17.9722039657874,-65.1968549373091,34.4104047659024));
#15643=CARTESIAN_POINT('Ctrl Pts',(18.8697771195624,-63.8504033302666,34.3330032301266));
#15644=CARTESIAN_POINT('Ctrl Pts',(21.1929366190789,-63.8845631923098,34.2218701121351));
#15645=CARTESIAN_POINT('Ctrl Pts',(22.4242737809404,-65.8548543459294,34.1107369941435));
#15646=CARTESIAN_POINT('Ctrl Pts',(21.4368200548297,-67.9579883834045,33.9996038761519));
#15647=CARTESIAN_POINT('Ctrl Pts',(19.134332114609,-68.2690944527448,33.8884707581604));
#15648=CARTESIAN_POINT('Ctrl Pts',(18.0221619398455,-66.9687900530357,33.8066277059305));
#15649=CARTESIAN_POINT('Ctrl Pts',(17.9434080634338,-66.1447297479887,33.7618290263645));
#15650=CARTESIAN_POINT('Ctrl Pts',(17.9447268179648,-66.0018413363536,33.7540747194623));
#15651=CARTESIAN_POINT('Origin',(20.,-66.,37.5459252805377));
#15652=CARTESIAN_POINT('',(17.9479090675131,-65.9988355335402,35.1540747194623));
#15653=CARTESIAN_POINT('',(17.9436250231948,-66.0016062109329,35.0959252805377));
#15654=CARTESIAN_POINT('',(17.94525,-65.9999999999999,37.5459252805377));
#15655=CARTESIAN_POINT('Ctrl Pts',(17.9436250231948,-66.0016062109329,35.0959252805377));
#15656=CARTESIAN_POINT('Ctrl Pts',(17.9485747848709,-65.4253659599372,35.0646103934386));
#15657=CARTESIAN_POINT('Ctrl Pts',(18.5015294951086,-64.1591280542333,34.9962511336756));
#15658=CARTESIAN_POINT('Ctrl Pts',(20.6477354930483,-63.6593582743169,34.8908475012487));
#15659=CARTESIAN_POINT('Ctrl Pts',(22.317770651701,-65.2746643793748,34.7797143832572));
#15660=CARTESIAN_POINT('Ctrl Pts',(21.8664910684258,-67.5538288400258,34.6685812652657));
#15661=CARTESIAN_POINT('Ctrl Pts',(19.7069253021358,-68.4108666608038,34.5574481472741));
#15662=CARTESIAN_POINT('Ctrl Pts',(18.160182505541,-67.3072525638627,34.4665628190314));
#15663=CARTESIAN_POINT('Ctrl Pts',(17.947762778659,-66.3114566072458,34.4127218634526));
#15664=CARTESIAN_POINT('Ctrl Pts',(17.9484640666104,-66.0005177854496,34.3959252805377));
#15665=CARTESIAN_POINT('Ctrl Pts',(17.9479090675131,-65.9988355335402,35.1540747194623));
#15666=CARTESIAN_POINT('Ctrl Pts',(17.9465290735626,-65.732812424341,35.1396948316641));
#15667=CARTESIAN_POINT('Ctrl Pts',(18.1181888186522,-64.7831883521569,35.088270571202));
#15668=CARTESIAN_POINT('Ctrl Pts',(19.5507727141961,-63.6133045893429,34.9998019380759));
#15669=CARTESIAN_POINT('Ctrl Pts',(21.761489776565,-64.3280769471683,34.8886688200845));
#15670=CARTESIAN_POINT('Ctrl Pts',(22.3600352216356,-66.5730755571057,34.7775357020928));
#15671=CARTESIAN_POINT('Ctrl Pts',(20.7985769413999,-68.2935646002867,34.6664025841013));
#15672=CARTESIAN_POINT('Ctrl Pts',(18.5745658878196,-67.9261849676859,34.5585822565578));
#15673=CARTESIAN_POINT('Ctrl Pts',(17.9464194490253,-66.6187842935463,34.4878063016781));
#15674=CARTESIAN_POINT('Ctrl Pts',(17.9425257907963,-65.9989407170969,34.4540747194623));
#15675=CARTESIAN_POINT('Origin',(20.,-66.,37.5459252805377));
#15676=CARTESIAN_POINT('',(17.9473272127329,-66.0023217579764,35.8540747194623));
#15677=CARTESIAN_POINT('',(17.9434279331127,-65.9985037039655,35.7959252805377));
#15678=CARTESIAN_POINT('',(17.94525,-65.9999999999999,37.5459252805377));
#15679=CARTESIAN_POINT('',(19.4698297828114,-67.9851743256717,36.));
#15680=CARTESIAN_POINT('Ctrl Pts',(19.4698297828114,-67.9851743256717,36.));
#15681=CARTESIAN_POINT('Ctrl Pts',(18.8097404375819,-67.8088876857537,35.9629556273362));
#15682=CARTESIAN_POINT('Ctrl Pts',(18.0750703124531,-67.1127915443424,35.9143138671569));
#15683=CARTESIAN_POINT('Ctrl Pts',(17.9457101070604,-66.2165907677818,35.8656721069777));
#15684=CARTESIAN_POINT('Ctrl Pts',(17.9473272127329,-66.0023217579764,35.8540747194623));
#15685=CARTESIAN_POINT('',(20.5313109889995,-67.9887317423832,36.));
#15686=CARTESIAN_POINT('Origin',(20.,-66.,36.));
#15687=CARTESIAN_POINT('Ctrl Pts',(20.5313116823135,-67.9887339044341,36.));
#15688=CARTESIAN_POINT('Ctrl Pts',(19.886791211028,-68.1600296186371,35.9636818543909));
#15689=CARTESIAN_POINT('Ctrl Pts',(18.5070308443187,-67.8407344661192,35.8956569479035));
#15690=CARTESIAN_POINT('Ctrl Pts',(17.9482807821384,-66.581675938278,35.8276320414161));
#15691=CARTESIAN_POINT('Ctrl Pts',(17.9434279331127,-65.9985037039655,35.7959252805377));
#15692=CARTESIAN_POINT('Origin',(-20.,66.,30.));
#15693=CARTESIAN_POINT('',(-21.6686462681531,65.9996083069911,25.7714803633902));
#15694=CARTESIAN_POINT('',(-21.6665334416367,66.0014781716809,25.5785196366098));
#15695=CARTESIAN_POINT('',(-21.666,66.,30.));
#15696=CARTESIAN_POINT('',(-20.7699020406705,64.5225674811446,25.));
#15697=CARTESIAN_POINT('Ctrl Pts',(-21.6665334416367,66.0014781716809,25.5785196366098));
#15698=CARTESIAN_POINT('Ctrl Pts',(-21.6675830928675,66.1152855193122,25.5709016210591));
#15699=CARTESIAN_POINT('Ctrl Pts',(-21.6569163987491,66.2288979483422,25.5632836055085));
#15700=CARTESIAN_POINT('Ctrl Pts',(-21.6338086023805,66.3399235421032,25.5556655899578));
#15701=CARTESIAN_POINT('Ctrl Pts',(-21.5214415673665,66.8798113177522,25.518621217294));
#15702=CARTESIAN_POINT('Ctrl Pts',(-21.1148901326579,67.3585303508392,25.4815768446301));
#15703=CARTESIAN_POINT('Ctrl Pts',(-20.6004654535252,67.5569679067401,25.4445324719662));
#15704=CARTESIAN_POINT('Ctrl Pts',(-20.0860407743925,67.7554054626409,25.4074880993024));
#15705=CARTESIAN_POINT('Ctrl Pts',(-19.4637428508357,67.6735615413556,25.3704437266385));
#15706=CARTESIAN_POINT('Ctrl Pts',(-19.0178170908,67.3489733082452,25.3333993539747));
#15707=CARTESIAN_POINT('Ctrl Pts',(-18.5718913307643,67.0243850751348,25.2963549813108));
#15708=CARTESIAN_POINT('Ctrl Pts',(-18.3023377342496,66.4570525301995,25.259310608647));
#15709=CARTESIAN_POINT('Ctrl Pts',(-18.3335864217295,65.9064187381511,25.2222662359831));
#15710=CARTESIAN_POINT('Ctrl Pts',(-18.3648351092095,65.3557849461027,25.1852218633193));
#15711=CARTESIAN_POINT('Ctrl Pts',(-18.696886080684,64.8218499069412,25.1481774906554));
#15712=CARTESIAN_POINT('Ctrl Pts',(-19.1753377222773,64.5495456028442,25.1111331179916));
#15713=CARTESIAN_POINT('Ctrl Pts',(-19.6537893638706,64.2772412987472,25.0740887453277));
#15714=CARTESIAN_POINT('Ctrl Pts',(-20.2786416755828,64.2665677297147,25.0370443726639));
#15715=CARTESIAN_POINT('Ctrl Pts',(-20.7699020406704,64.5225674811445,25.));
#15716=CARTESIAN_POINT('',(-21.3370260870439,66.9990029413793,25.));
#15717=CARTESIAN_POINT('Origin',(-20.,66.,25.));
#15718=CARTESIAN_POINT('',(-21.6645215499604,65.9987788526261,25.0714803633902));
#15719=CARTESIAN_POINT('Ctrl Pts',(-21.3370275036536,66.9990041127265,25.));
#15720=CARTESIAN_POINT('Ctrl Pts',(-21.5489928091346,66.714549930132,25.0238267877968));
#15721=CARTESIAN_POINT('Ctrl Pts',(-21.6621689158337,66.3559372077737,25.0476535755935));
#15722=CARTESIAN_POINT('Ctrl Pts',(-21.6645215499604,65.9987788526261,25.0714803633902));
#15723=CARTESIAN_POINT('',(-21.666,66.,24.));
#15724=CARTESIAN_POINT('',(-21.666,66.,30.));
#15725=CARTESIAN_POINT('Origin',(-20.,66.,24.));
#15726=CARTESIAN_POINT('Ctrl Pts',(-21.6645215499604,65.9987788526261,25.0714803633902));
#15727=CARTESIAN_POINT('Ctrl Pts',(-21.6657549346251,65.8115361219705,25.0839717212025));
#15728=CARTESIAN_POINT('Ctrl Pts',(-21.6365290094972,65.624693117297,25.0964630790149));
#15729=CARTESIAN_POINT('Ctrl Pts',(-21.5751097615993,65.4491448676051,25.1089544368272));
#15730=CARTESIAN_POINT('Ctrl Pts',(-21.3929648305163,64.9285389511166,25.145998809491));
#15731=CARTESIAN_POINT('Ctrl Pts',(-20.927686570446,64.5072679681757,25.1830431821549));
#15732=CARTESIAN_POINT('Ctrl Pts',(-20.3917115430329,64.3778810633712,25.2200875548188));
#15733=CARTESIAN_POINT('Ctrl Pts',(-19.8557365156198,64.2484941585667,25.2571319274826));
#15734=CARTESIAN_POINT('Ctrl Pts',(-19.2490647208639,64.4109913318987,25.2941763001465));
#15735=CARTESIAN_POINT('Ctrl Pts',(-18.8495628769352,64.7911274066971,25.3312206728103));
#15736=CARTESIAN_POINT('Ctrl Pts',(-18.4500610330064,65.1712634814956,25.3682650454742));
#15737=CARTESIAN_POINT('Ctrl Pts',(-18.2577291399049,65.7690384577606,25.405309418138));
#15738=CARTESIAN_POINT('Ctrl Pts',(-18.3604608656205,66.3108401952129,25.4423537908019));
#15739=CARTESIAN_POINT('Ctrl Pts',(-18.4631925913361,66.8526419326652,25.4793981634657));
#15740=CARTESIAN_POINT('Ctrl Pts',(-18.8609879358689,67.3384704313048,25.5164425361296));
#15741=CARTESIAN_POINT('Ctrl Pts',(-19.3718687026598,67.5460303751797,25.5534869087934));
#15742=CARTESIAN_POINT('Ctrl Pts',(-19.8827494694507,67.7535903190547,25.5905312814573));
#15743=CARTESIAN_POINT('Ctrl Pts',(-20.5067156584998,67.682881708165,25.6275756541211));
#15744=CARTESIAN_POINT('Ctrl Pts',(-20.9581975756331,67.3662474649163,25.664620026785));
#15745=CARTESIAN_POINT('Ctrl Pts',(-21.3923211790011,67.0617869906151,25.7002401389867));
#15746=CARTESIAN_POINT('Ctrl Pts',(-21.6669686931593,66.5299477666492,25.7358602511885));
#15747=CARTESIAN_POINT('Ctrl Pts',(-21.6686462681531,65.9996083069911,25.7714803633902));
#15748=CARTESIAN_POINT('Origin',(-20.,66.,30.));
#15749=CARTESIAN_POINT('',(-21.6655732346566,66.0015125422222,26.4714803633902));
#15750=CARTESIAN_POINT('',(-21.6632974484405,65.9999597910396,26.2785196366098));
#15751=CARTESIAN_POINT('',(-21.666,66.,30.));
#15752=CARTESIAN_POINT('Ctrl Pts',(-21.6632974484405,65.9999597910396,26.2785196366098));
#15753=CARTESIAN_POINT('Ctrl Pts',(-21.66323743521,66.2804571829106,26.2598345237089));
#15754=CARTESIAN_POINT('Ctrl Pts',(-21.5960667645061,66.5609817057811,26.241149410808));
#15755=CARTESIAN_POINT('Ctrl Pts',(-21.4619468807006,66.8046575880589,26.2224642979072));
#15756=CARTESIAN_POINT('Ctrl Pts',(-21.196046054536,67.2877598438589,26.1854199252433));
#15757=CARTESIAN_POINT('Ctrl Pts',(-20.666998173837,67.6260267717087,26.1483755525794));
#15758=CARTESIAN_POINT('Ctrl Pts',(-20.116910180859,67.6646601094217,26.1113311799156));
#15759=CARTESIAN_POINT('Ctrl Pts',(-19.566822187881,67.7032934471347,26.0742868072517));
#15760=CARTESIAN_POINT('Ctrl Pts',(-18.995694082624,67.4422931947108,26.0372424345879));
#15761=CARTESIAN_POINT('Ctrl Pts',(-18.6648769112216,67.0010995179133,26.000198061924));
#15762=CARTESIAN_POINT('Ctrl Pts',(-18.3340597398192,66.5599058411157,25.9631536892602));
#15763=CARTESIAN_POINT('Ctrl Pts',(-18.2435535022714,65.9385187399443,25.9261093165963));
#15764=CARTESIAN_POINT('Ctrl Pts',(-18.4347924103425,65.4212945612671,25.8890649439325));
#15765=CARTESIAN_POINT('Ctrl Pts',(-18.6260313184137,64.9040703825899,25.8520205712686));
#15766=CARTESIAN_POINT('Ctrl Pts',(-19.0990153721038,64.4910091264068,25.8149761986048));
#15767=CARTESIAN_POINT('Ctrl Pts',(-19.6372643126555,64.3711409749501,25.7779318259409));
#15768=CARTESIAN_POINT('Ctrl Pts',(-20.1755132532071,64.2512728234933,25.7408874532771));
#15769=CARTESIAN_POINT('Ctrl Pts',(-20.7790270806202,64.424597776763,25.7038430806132));
#15770=CARTESIAN_POINT('Ctrl Pts',(-21.1716926766671,64.8117885125033,25.6667987079494));
#15771=CARTESIAN_POINT('Ctrl Pts',(-21.4836082855555,65.1193551425066,25.6373723508362));
#15772=CARTESIAN_POINT('Ctrl Pts',(-21.6624789195953,65.5618708183968,25.607945993723));
#15773=CARTESIAN_POINT('Ctrl Pts',(-21.6665334416367,66.0014781716809,25.5785196366098));
#15774=CARTESIAN_POINT('Ctrl Pts',(-21.6686462681531,65.9996083069911,25.7714803633902));
#15775=CARTESIAN_POINT('Ctrl Pts',(-21.6687133455312,65.978402828479,25.7729046238523));
#15776=CARTESIAN_POINT('Ctrl Pts',(-21.6683440044686,65.9571997477577,25.7743288843144));
#15777=CARTESIAN_POINT('Ctrl Pts',(-21.667530989676,65.9360136962792,25.7757531447766));
#15778=CARTESIAN_POINT('Ctrl Pts',(-21.6463848413682,65.3849740464984,25.8127975174404));
#15779=CARTESIAN_POINT('Ctrl Pts',(-21.3250948995353,64.8454546225443,25.8498418901043));
#15780=CARTESIAN_POINT('Ctrl Pts',(-20.8506820945636,64.5643464247502,25.8868862627681));
#15781=CARTESIAN_POINT('Ctrl Pts',(-20.3762692895919,64.283238226956,25.923930635432));
#15782=CARTESIAN_POINT('Ctrl Pts',(-19.7487336214815,64.2605412553218,25.9609750080958));
#15783=CARTESIAN_POINT('Ctrl Pts',(-19.2552516088359,64.5066439494556,25.9980193807597));
#15784=CARTESIAN_POINT('Ctrl Pts',(-18.7617695961903,64.7527466435894,26.0350637534235));
#15785=CARTESIAN_POINT('Ctrl Pts',(-18.4023412390094,65.2676490034913,26.0721081260874));
#15786=CARTESIAN_POINT('Ctrl Pts',(-18.3414460973868,65.8157206437916,26.1091524987512));
#15787=CARTESIAN_POINT('Ctrl Pts',(-18.2805509557642,66.3637922840919,26.1461968714151));
#15788=CARTESIAN_POINT('Ctrl Pts',(-18.5181890296997,66.9450332047907,26.1832412440789));
#15789=CARTESIAN_POINT('Ctrl Pts',(-18.9456134277585,67.2934565894908,26.2202856167428));
#15790=CARTESIAN_POINT('Ctrl Pts',(-19.3730378258172,67.6418799741908,26.2573299894066));
#15791=CARTESIAN_POINT('Ctrl Pts',(-19.9902485479992,67.7574858228921,26.2943743620705));
#15792=CARTESIAN_POINT('Ctrl Pts',(-20.5147973357793,67.5873703895759,26.3314187347344));
#15793=CARTESIAN_POINT('Ctrl Pts',(-21.0393461235593,67.4172549562597,26.3684631073982));
#15794=CARTESIAN_POINT('Ctrl Pts',(-21.4712329769374,66.9614182409261,26.4055074800621));
#15795=CARTESIAN_POINT('Ctrl Pts',(-21.6128182158583,66.4284602129379,26.4425518527259));
#15796=CARTESIAN_POINT('Ctrl Pts',(-21.6496735670628,66.2897285524311,26.452194689614));
#15797=CARTESIAN_POINT('Ctrl Pts',(-21.6668584543246,66.14577125099,26.4618375265021));
#15798=CARTESIAN_POINT('Ctrl Pts',(-21.6655732346566,66.0015125422222,26.4714803633902));
#15799=CARTESIAN_POINT('Origin',(-20.,66.,30.));
#15800=CARTESIAN_POINT('',(-21.6634529018243,65.9994718482165,27.1714803633902));
#15801=CARTESIAN_POINT('',(-21.6666334235039,65.9985354189402,26.9785196366098));
#15802=CARTESIAN_POINT('',(-21.666,66.,30.));
#15803=CARTESIAN_POINT('Ctrl Pts',(-21.6666334235039,65.9985354189402,26.9785196366098));
#15804=CARTESIAN_POINT('Ctrl Pts',(-21.6625547393445,66.4429099184687,26.9487674263587));
#15805=CARTESIAN_POINT('Ctrl Pts',(-21.4793115692531,66.8902540064005,26.9190152161076));
#15806=CARTESIAN_POINT('Ctrl Pts',(-21.1612403286263,67.1984497694804,26.8892630058565));
#15807=CARTESIAN_POINT('Ctrl Pts',(-20.7652109421709,67.5821832334683,26.8522186331926));
#15808=CARTESIAN_POINT('Ctrl Pts',(-20.1601622793762,67.7501998808548,26.8151742605288));
#15809=CARTESIAN_POINT('Ctrl Pts',(-19.6229765827774,67.6256119767683,26.7781298878649));
#15810=CARTESIAN_POINT('Ctrl Pts',(-19.0857908861786,67.5010240726819,26.7410855152011));
#15811=CARTESIAN_POINT('Ctrl Pts',(-18.6164681557757,67.0838316171223,26.7040411425373));
#15812=CARTESIAN_POINT('Ctrl Pts',(-18.4297795752062,66.56495010894,26.6669967698734));
#15813=CARTESIAN_POINT('Ctrl Pts',(-18.2430909946367,66.0460686007576,26.6299523972095));
#15814=CARTESIAN_POINT('Ctrl Pts',(-18.3390365639006,65.4254980399525,26.5929080245457));
#15815=CARTESIAN_POINT('Ctrl Pts',(-18.6737099694251,64.9872236861523,26.5558636518818));
#15816=CARTESIAN_POINT('Ctrl Pts',(-19.0083833749495,64.5489493323522,26.518819279218));
#15817=CARTESIAN_POINT('Ctrl Pts',(-19.5817846167346,64.2929711855571,26.4817749065541));
#15818=CARTESIAN_POINT('Ctrl Pts',(-20.1315134695615,64.3364299664923,26.4447305338903));
#15819=CARTESIAN_POINT('Ctrl Pts',(-20.6812423223883,64.3798887474276,26.4076861612264));
#15820=CARTESIAN_POINT('Ctrl Pts',(-21.2072987862569,64.7227844560932,26.3706417885626));
#15821=CARTESIAN_POINT('Ctrl Pts',(-21.4689501323761,65.208201102301,26.3335974158987));
#15822=CARTESIAN_POINT('Ctrl Pts',(-21.5986250245473,65.4487744919996,26.3152381561357));
#15823=CARTESIAN_POINT('Ctrl Pts',(-21.6633564150892,65.7243540450368,26.2968788963728));
#15824=CARTESIAN_POINT('Ctrl Pts',(-21.6632974484405,65.9999597910396,26.2785196366098));
#15825=CARTESIAN_POINT('Ctrl Pts',(-21.6655732346566,66.0015125422222,26.4714803633902));
#15826=CARTESIAN_POINT('Ctrl Pts',(-21.6619210944078,65.591580256201,26.4988818991659));
#15827=CARTESIAN_POINT('Ctrl Pts',(-21.5091236523064,65.1792141192603,26.5262834349417));
#15828=CARTESIAN_POINT('Ctrl Pts',(-21.2347245072689,64.8774064445228,26.5536849707175));
#15829=CARTESIAN_POINT('Ctrl Pts',(-20.8637619352948,64.4693900447385,26.5907293433813));
#15830=CARTESIAN_POINT('Ctrl Pts',(-20.270553166883,64.2634365858125,26.6277737160452));
#15831=CARTESIAN_POINT('Ctrl Pts',(-19.7265622699546,64.353794453272,26.664818088709));
#15832=CARTESIAN_POINT('Ctrl Pts',(-19.1825713730262,64.4441523207316,26.7018624613729));
#15833=CARTESIAN_POINT('Ctrl Pts',(-18.6877983475811,64.8308215145768,26.7389068340367));
#15834=CARTESIAN_POINT('Ctrl Pts',(-18.4686610363739,65.3368545872826,26.7759512067006));
#15835=CARTESIAN_POINT('Ctrl Pts',(-18.2495237251666,65.8428876599883,26.8129955793645));
#15836=CARTESIAN_POINT('Ctrl Pts',(-18.3060221281972,66.4682846115547,26.8500399520283));
#15837=CARTESIAN_POINT('Ctrl Pts',(-18.6123014797734,66.9268514966992,26.8870843246922));
#15838=CARTESIAN_POINT('Ctrl Pts',(-18.9185808313496,67.3854183818437,26.924128697356));
#15839=CARTESIAN_POINT('Ctrl Pts',(-19.4746411314715,67.6771552005663,26.9611730700198));
#15840=CARTESIAN_POINT('Ctrl Pts',(-20.0260182359126,67.6685574395601,26.9982174426837));
#15841=CARTESIAN_POINT('Ctrl Pts',(-20.5773953403537,67.6599596785538,27.0352618153475));
#15842=CARTESIAN_POINT('Ctrl Pts',(-21.1240892491141,67.3510273378186,27.0723061880114));
#15843=CARTESIAN_POINT('Ctrl Pts',(-21.4159220745912,66.8831339380774,27.1093505606753));
#15844=CARTESIAN_POINT('Ctrl Pts',(-21.5790734033788,66.6215546254215,27.1300604949136));
#15845=CARTESIAN_POINT('Ctrl Pts',(-21.6625691024306,66.3102927833835,27.1507704291519));
#15846=CARTESIAN_POINT('Ctrl Pts',(-21.6634529018243,65.9994718482165,27.1714803633902));
#15847=CARTESIAN_POINT('Origin',(-20.,66.,30.));
#15848=CARTESIAN_POINT('',(-21.667507940799,65.9987669700874,27.8714803633902));
#15849=CARTESIAN_POINT('',(-21.6680616533731,66.0009590761454,27.6785196366098));
#15850=CARTESIAN_POINT('',(-21.666,66.,30.));
#15851=CARTESIAN_POINT('Ctrl Pts',(-21.6680616533731,66.0009590761454,27.6785196366098));
#15852=CARTESIAN_POINT('Ctrl Pts',(-21.668447753273,66.0572154640797,27.6747447016723));
#15853=CARTESIAN_POINT('Ctrl Pts',(-21.6658484356799,66.1134357515378,27.6709697667349));
#15854=CARTESIAN_POINT('Ctrl Pts',(-21.6601460955106,66.1693395220565,27.6671948317974));
#15855=CARTESIAN_POINT('Ctrl Pts',(-21.6041876173419,66.7179370853841,27.6301504591336));
#15856=CARTESIAN_POINT('Ctrl Pts',(-21.2494085740158,67.2360541193704,27.5931060864697));
#15857=CARTESIAN_POINT('Ctrl Pts',(-20.7581628372053,67.4865900729032,27.5560617138058));
#15858=CARTESIAN_POINT('Ctrl Pts',(-20.2669171003947,67.737126026436,27.519017341142));
#15859=CARTESIAN_POINT('Ctrl Pts',(-19.6392046700997,67.7200808995153,27.4819729684782));
#15860=CARTESIAN_POINT('Ctrl Pts',(-19.1622791087534,67.4432548774978,27.4449285958143));
#15861=CARTESIAN_POINT('Ctrl Pts',(-18.6853535474071,67.1664288554803,27.4078842231505));
#15862=CARTESIAN_POINT('Ctrl Pts',(-18.3592148550096,66.629821938366,27.3708398504866));
#15863=CARTESIAN_POINT('Ctrl Pts',(-18.3331105134156,66.0789960120806,27.3337954778227));
#15864=CARTESIAN_POINT('Ctrl Pts',(-18.3070061718216,65.5281700857952,27.2967511051589));
#15865=CARTESIAN_POINT('Ctrl Pts',(-18.5809361810313,64.9631251503388,27.259706732495));
#15866=CARTESIAN_POINT('Ctrl Pts',(-19.0295447821931,64.6424368874882,27.2226623598312));
#15867=CARTESIAN_POINT('Ctrl Pts',(-19.4781533833549,64.3217486246376,27.1856179871673));
#15868=CARTESIAN_POINT('Ctrl Pts',(-20.1014405764689,64.2454170343927,27.1485736145035));
#15869=CARTESIAN_POINT('Ctrl Pts',(-20.6141778673144,64.4483729559646,27.1115292418396));
#15870=CARTESIAN_POINT('Ctrl Pts',(-21.12691515816,64.6513288775365,27.0744848691758));
#15871=CARTESIAN_POINT('Ctrl Pts',(-21.529102546737,65.1335723109252,27.0374404965119));
#15872=CARTESIAN_POINT('Ctrl Pts',(-21.6366911859674,65.6744191679142,27.0003961238481));
#15873=CARTESIAN_POINT('Ctrl Pts',(-21.6578699446997,65.7808845454597,26.9931039614353));
#15874=CARTESIAN_POINT('Ctrl Pts',(-21.6676330946903,65.8896207872102,26.9858117990226));
#15875=CARTESIAN_POINT('Ctrl Pts',(-21.6666334235039,65.9985354189402,26.9785196366098));
#15876=CARTESIAN_POINT('Ctrl Pts',(-21.6634529018243,65.9994718482165,27.1714803633902));
#15877=CARTESIAN_POINT('Ctrl Pts',(-21.6641499763108,65.7543196730124,27.1878148018157));
#15878=CARTESIAN_POINT('Ctrl Pts',(-21.6134552796394,65.5094417801467,27.2041492402413));
#15879=CARTESIAN_POINT('Ctrl Pts',(-21.5099183024031,65.2894314975948,27.2204836786668));
#15880=CARTESIAN_POINT('Ctrl Pts',(-21.275109962544,64.7904769156004,27.2575280513307));
#15881=CARTESIAN_POINT('Ctrl Pts',(-20.7685215406322,64.4194222103586,27.2945724239945));
#15882=CARTESIAN_POINT('Ctrl Pts',(-20.2219778690728,64.3460693177449,27.3316167966584));
#15883=CARTESIAN_POINT('Ctrl Pts',(-19.6754341975135,64.2727164251311,27.3686611693223));
#15884=CARTESIAN_POINT('Ctrl Pts',(-19.0889352763067,64.4970653451454,27.4057055419861));
#15885=CARTESIAN_POINT('Ctrl Pts',(-18.7308745534937,64.916449596609,27.4427499146499));
#15886=CARTESIAN_POINT('Ctrl Pts',(-18.3728138306807,65.3358338480726,27.4797942873138));
#15887=CARTESIAN_POINT('Ctrl Pts',(-18.2431913062614,65.9502534309856,27.5168386599777));
#15888=CARTESIAN_POINT('Ctrl Pts',(-18.401324798602,66.478537852666,27.5538830326415));
#15889=CARTESIAN_POINT('Ctrl Pts',(-18.5594582909426,67.0068222743464,27.5909274053054));
#15890=CARTESIAN_POINT('Ctrl Pts',(-19.005347800043,67.4489715347942,27.6279717779692));
#15891=CARTESIAN_POINT('Ctrl Pts',(-19.5349455113959,67.6026494309563,27.6650161506331));
#15892=CARTESIAN_POINT('Ctrl Pts',(-20.0645432227487,67.7563273271185,27.7020605232969));
#15893=CARTESIAN_POINT('Ctrl Pts',(-20.6778491363538,67.621533858995,27.7391048959608));
#15894=CARTESIAN_POINT('Ctrl Pts',(-21.0942023964646,67.2599531703386,27.7761492686246));
#15895=CARTESIAN_POINT('Ctrl Pts',(-21.4513543671184,66.9497856566518,27.8079263002132));
#15896=CARTESIAN_POINT('Ctrl Pts',(-21.6635811076441,66.472739507198,27.8397033318017));
#15897=CARTESIAN_POINT('Ctrl Pts',(-21.667507940799,65.9987669700874,27.8714803633902));
#15898=CARTESIAN_POINT('Origin',(-20.,66.,30.));
#15899=CARTESIAN_POINT('',(-21.6672880002095,66.001310374389,28.5714803633902));
#15900=CARTESIAN_POINT('',(-21.6637335518062,66.000855499652,28.3785196366098));
#15901=CARTESIAN_POINT('',(-21.666,66.,30.));
#15902=CARTESIAN_POINT('Ctrl Pts',(-21.6637335518062,66.000855499652,28.3785196366098));
#15903=CARTESIAN_POINT('Ctrl Pts',(-21.6647696061116,66.2235152669179,28.3636776043221));
#15904=CARTESIAN_POINT('Ctrl Pts',(-21.6232170679033,66.4458042001806,28.3488355720345));
#15905=CARTESIAN_POINT('Ctrl Pts',(-21.5372474291621,66.6493314053291,28.3339935397468));
#15906=CARTESIAN_POINT('Ctrl Pts',(-21.3226749721306,67.157316935115,28.2969491670829));
#15907=CARTESIAN_POINT('Ctrl Pts',(-20.8314032853562,67.5484250538238,28.2599047944191));
#15908=CARTESIAN_POINT('Ctrl Pts',(-20.2882479608308,67.6436769894029,28.2228604217552));
#15909=CARTESIAN_POINT('Ctrl Pts',(-19.7450926363055,67.738928924982,28.1858160490914));
#15910=CARTESIAN_POINT('Ctrl Pts',(-19.1500536740293,67.5383246774313,28.1487716764275));
#15911=CARTESIAN_POINT('Ctrl Pts',(-18.7754326134094,67.1336646982806,28.1117273037637));
#15912=CARTESIAN_POINT('Ctrl Pts',(-18.4008115527896,66.7290047191299,28.0746829310998));
#15913=CARTESIAN_POINT('Ctrl Pts',(-18.2466083938262,66.1202890083791,28.0376385584359));
#15914=CARTESIAN_POINT('Ctrl Pts',(-18.3833895367155,65.5860778546815,28.0005941857721));
#15915=CARTESIAN_POINT('Ctrl Pts',(-18.5201706796048,65.051866700984,27.9635498131083));
#15916=CARTESIAN_POINT('Ctrl Pts',(-18.9479361243467,64.5921601043397,27.9265054404444));
#15917=CARTESIAN_POINT('Ctrl Pts',(-19.4709319851533,64.4173288503001,27.8894610677805));
#15918=CARTESIAN_POINT('Ctrl Pts',(-19.9939278459598,64.2424975962605,27.8524166951167));
#15919=CARTESIAN_POINT('Ctrl Pts',(-20.6121541228309,64.3525416848257,27.8153723224528));
#15920=CARTESIAN_POINT('Ctrl Pts',(-21.0426983047608,64.6971027754428,27.778327949789));
#15921=CARTESIAN_POINT('Ctrl Pts',(-21.4293687170027,65.0065520365018,27.7450585120626));
#15922=CARTESIAN_POINT('Ctrl Pts',(-21.6646588592093,65.5051575786095,27.7117890743362));
#15923=CARTESIAN_POINT('Ctrl Pts',(-21.6680616533731,66.0009590761454,27.6785196366098));
#15924=CARTESIAN_POINT('Ctrl Pts',(-21.667507940799,65.9987669700874,27.8714803633902));
#15925=CARTESIAN_POINT('Ctrl Pts',(-21.6681588502308,65.9202015758861,27.8767477044655));
#15926=CARTESIAN_POINT('Ctrl Pts',(-21.6630864755223,65.8417206327871,27.8820150455409));
#15927=CARTESIAN_POINT('Ctrl Pts',(-21.6520021809334,65.7640981769684,27.8872823866162));
#15928=CARTESIAN_POINT('Ctrl Pts',(-21.5740480986749,65.2181917814439,27.92432675928));
#15929=CARTESIAN_POINT('Ctrl Pts',(-21.1987393275416,64.7147468995842,27.9613711319439));
#15930=CARTESIAN_POINT('Ctrl Pts',(-20.6978245472241,64.4841498170345,27.9984155046077));
#15931=CARTESIAN_POINT('Ctrl Pts',(-20.1969097669067,64.2535527344848,28.0354598772716));
#15932=CARTESIAN_POINT('Ctrl Pts',(-19.5703889774051,64.2958034512451,28.0725042499354));
#15933=CARTESIAN_POINT('Ctrl Pts',(-19.1049704217966,64.5915672078361,28.1095486225993));
#15934=CARTESIAN_POINT('Ctrl Pts',(-18.6395518661881,64.8873309644271,28.1465929952632));
#15935=CARTESIAN_POINT('Ctrl Pts',(-18.3352355444726,65.4366077608489,28.183637367927));
#15936=CARTESIAN_POINT('Ctrl Pts',(-18.3312825943579,65.9880377253988,28.2206817405909));
#15937=CARTESIAN_POINT('Ctrl Pts',(-18.3273296442431,66.5394676899486,28.2577261132547));
#15938=CARTESIAN_POINT('Ctrl Pts',(-18.6237400657292,67.0930508226264,28.2947704859186));
#15939=CARTESIAN_POINT('Ctrl Pts',(-19.0848706166418,67.395456587508,28.3318148585824));
#15940=CARTESIAN_POINT('Ctrl Pts',(-19.5460011675545,67.6978623523895,28.3688592312463));
#15941=CARTESIAN_POINT('Ctrl Pts',(-20.1718518478936,67.7490907494749,28.4059036039101));
#15942=CARTESIAN_POINT('Ctrl Pts',(-20.6760210697158,67.5256986560933,28.442947976574));
#15943=CARTESIAN_POINT('Ctrl Pts',(-21.1801902915379,67.3023065627116,28.4799923492378));
#15944=CARTESIAN_POINT('Ctrl Pts',(-21.562678054843,66.804293978863,28.5170367219017));
#15945=CARTESIAN_POINT('Ctrl Pts',(-21.6484504318563,66.2595612637084,28.5540810945655));
#15946=CARTESIAN_POINT('Ctrl Pts',(-21.6618791619446,66.1742765968166,28.5598808508404));
#15947=CARTESIAN_POINT('Ctrl Pts',(-21.6680348672868,66.0878467359549,28.5656806071153));
#15948=CARTESIAN_POINT('Ctrl Pts',(-21.6672880002095,66.001310374389,28.5714803633902));
#15949=CARTESIAN_POINT('Origin',(-20.,66.,30.));
#15950=CARTESIAN_POINT('',(-21.6633861604904,66.0004031163274,29.2714803633902));
#15951=CARTESIAN_POINT('',(-21.6649409063295,65.9985780813102,29.0785196366098));
#15952=CARTESIAN_POINT('',(-21.666,66.,30.));
#15953=CARTESIAN_POINT('Ctrl Pts',(-21.6649409063295,65.9985780813102,29.0785196366098));
#15954=CARTESIAN_POINT('Ctrl Pts',(-21.6617887073852,66.3865573477782,29.0526105069719));
#15955=CARTESIAN_POINT('Ctrl Pts',(-21.5266090909747,66.7765166408617,29.026701377334));
#15956=CARTESIAN_POINT('Ctrl Pts',(-21.2788295744943,67.0720801517677,29.0007922476961));
#15957=CARTESIAN_POINT('Ctrl Pts',(-20.9245592120679,67.4946711456321,28.9637478750323));
#15958=CARTESIAN_POINT('Ctrl Pts',(-20.3401039415215,67.7242914136439,28.9267035023684));
#15959=CARTESIAN_POINT('Ctrl Pts',(-19.7929219966247,67.6558622022781,28.8896591297046));
#15960=CARTESIAN_POINT('Ctrl Pts',(-19.2457400517279,67.5874329909124,28.8526147570407));
#15961=CARTESIAN_POINT('Ctrl Pts',(-18.7358314324807,67.2209543001691,28.8155703843769));
#15962=CARTESIAN_POINT('Ctrl Pts',(-18.4965403579548,66.7241339911626,28.778526011713));
#15963=CARTESIAN_POINT('Ctrl Pts',(-18.2572492834288,66.2273136821561,28.7414816390492));
#15964=CARTESIAN_POINT('Ctrl Pts',(-18.2885757536241,65.6001517548864,28.7044372663853));
#15965=CARTESIAN_POINT('Ctrl Pts',(-18.5761841592798,65.1296498496988,28.6673928937215));
#15966=CARTESIAN_POINT('Ctrl Pts',(-18.8637925649355,64.6591479445111,28.6303485210576));
#15967=CARTESIAN_POINT('Ctrl Pts',(-19.4076829060515,64.3453060614055,28.5933041483937));
#15968=CARTESIAN_POINT('Ctrl Pts',(-19.9589602588768,64.3317444224388,28.5562597757299));
#15969=CARTESIAN_POINT('Ctrl Pts',(-20.510237611702,64.3181827834722,28.519215403066));
#15970=CARTESIAN_POINT('Ctrl Pts',(-21.0689019762364,64.6049013886446,28.4821710304022));
#15971=CARTESIAN_POINT('Ctrl Pts',(-21.3792975448593,65.0606921616624,28.4451266577383));
#15972=CARTESIAN_POINT('Ctrl Pts',(-21.56533141641,65.3338678467978,28.4229243173622));
#15973=CARTESIAN_POINT('Ctrl Pts',(-21.6621837080993,65.6677765893587,28.400721976986));
#15974=CARTESIAN_POINT('Ctrl Pts',(-21.6637335518062,66.000855499652,28.3785196366098));
#15975=CARTESIAN_POINT('Ctrl Pts',(-21.6672880002095,66.001310374389,28.5714803633902));
#15976=CARTESIAN_POINT('Ctrl Pts',(-21.663264456078,65.5351191600222,28.6027249797792));
#15977=CARTESIAN_POINT('Ctrl Pts',(-21.4589128088386,65.065837056818,28.6339695961681));
#15978=CARTESIAN_POINT('Ctrl Pts',(-21.112153076385,64.7558631865457,28.6652142125571));
#15979=CARTESIAN_POINT('Ctrl Pts',(-20.7010263531788,64.3883506709982,28.7022585852209));
#15980=CARTESIAN_POINT('Ctrl Pts',(-20.0897159160448,64.2447784863638,28.7393029578848));
#15981=CARTESIAN_POINT('Ctrl Pts',(-19.5579694514877,64.3908480898042,28.7763473305487));
#15982=CARTESIAN_POINT('Ctrl Pts',(-19.0262229869306,64.5369176932446,28.8133917032125));
#15983=CARTESIAN_POINT('Ctrl Pts',(-18.5740404949502,64.9726290847598,28.8504360758764));
#15984=CARTESIAN_POINT('Ctrl Pts',(-18.4083495827417,65.4985921568759,28.8874804485402));
#15985=CARTESIAN_POINT('Ctrl Pts',(-18.2426586705331,66.0245552289919,28.9245248212041));
#15986=CARTESIAN_POINT('Ctrl Pts',(-18.3634593380964,66.6407699817089,28.9615691938679));
#15987=CARTESIAN_POINT('Ctrl Pts',(-18.7154708226205,67.0652444171952,28.9986135665318));
#15988=CARTESIAN_POINT('Ctrl Pts',(-19.0674823071445,67.4897188526815,29.0356579391956));
#15989=CARTESIAN_POINT('Ctrl Pts',(-19.6507046086295,67.7224529709372,29.0727023118595));
#15990=CARTESIAN_POINT('Ctrl Pts',(-20.1982437242128,67.6569430592857,29.1097466845233));
#15991=CARTESIAN_POINT('Ctrl Pts',(-20.745782839796,67.5914331476342,29.1467910571872));
#15992=CARTESIAN_POINT('Ctrl Pts',(-21.2576387694775,67.2276792060755,29.183835429851));
#15993=CARTESIAN_POINT('Ctrl Pts',(-21.4995761666085,66.7321421968747,29.2208798025149));
#15994=CARTESIAN_POINT('Ctrl Pts',(-21.6097338604876,66.5065168292688,29.23774665614));
#15995=CARTESIAN_POINT('Ctrl Pts',(-21.663934303843,66.2535712993117,29.2546135097651));
#15996=CARTESIAN_POINT('Ctrl Pts',(-21.6633861604904,66.0004031163274,29.2714803633902));
#15997=CARTESIAN_POINT('Origin',(-20.,66.,30.));
#15998=CARTESIAN_POINT('',(-21.6658100649286,65.9984774013953,29.9714803633902));
#15999=CARTESIAN_POINT('',(-21.6687601286834,65.999981045721,29.7785196366098));
#16000=CARTESIAN_POINT('',(-21.666,66.,30.));
#16001=CARTESIAN_POINT('Ctrl Pts',(-21.6687600243793,65.9999810464372,29.7785196366098));
#16002=CARTESIAN_POINT('Ctrl Pts',(-21.6686674655839,66.550411009554,29.7415434096217));
#16003=CARTESIAN_POINT('Ctrl Pts',(-21.3695594894198,67.1009271605486,29.7045671826336));
#16004=CARTESIAN_POINT('Ctrl Pts',(-20.9076738855946,67.4003174817966,29.6675909556455));
#16005=CARTESIAN_POINT('Ctrl Pts',(-20.444937045471,67.7002595671756,29.6305465829816));
#16006=CARTESIAN_POINT('Ctrl Pts',(-19.8188220397766,67.7481493405696,29.5935022103178));
#16007=CARTESIAN_POINT('Ctrl Pts',(-19.3158514169405,67.5220714992119,29.5564578376539));
#16008=CARTESIAN_POINT('Ctrl Pts',(-18.8128807941043,67.2959936578542,29.5194134649901));
#16009=CARTESIAN_POINT('Ctrl Pts',(-18.4330545541264,66.7959482017448,29.4823690923262));
#16010=CARTESIAN_POINT('Ctrl Pts',(-18.3501886593282,66.250765772398,29.4453247196624));
#16011=CARTESIAN_POINT('Ctrl Pts',(-18.26732276453,65.7055833430513,29.4082803469985));
#16012=CARTESIAN_POINT('Ctrl Pts',(-18.4814172149115,65.1152639404671,29.3712359743347));
#16013=CARTESIAN_POINT('Ctrl Pts',(-18.8944981766404,64.7499493406408,29.3341916016708));
#16014=CARTESIAN_POINT('Ctrl Pts',(-19.3075791383693,64.3846347408145,29.297147229007));
#16015=CARTESIAN_POINT('Ctrl Pts',(-19.9196466114455,64.244324943746,29.2601028563431));
#16016=CARTESIAN_POINT('Ctrl Pts',(-20.450606474819,64.3932284738437,29.2230584836793));
#16017=CARTESIAN_POINT('Ctrl Pts',(-20.9815663381925,64.5421320039414,29.1860141110154));
#16018=CARTESIAN_POINT('Ctrl Pts',(-21.4314185918632,64.9802488612052,29.1489697383515));
#16019=CARTESIAN_POINT('Ctrl Pts',(-21.5943019915453,65.5070881496957,29.1119253656877));
#16020=CARTESIAN_POINT('Ctrl Pts',(-21.6432634426356,65.6654518387288,29.1007901226617));
#16021=CARTESIAN_POINT('Ctrl Pts',(-21.6662956604954,65.8318320932536,29.0896548796358));
#16022=CARTESIAN_POINT('Ctrl Pts',(-21.6649409063295,65.9985780813102,29.0785196366098));
#16023=CARTESIAN_POINT('Ctrl Pts',(-21.6633861604904,66.0004031163274,29.2714803633902));
#16024=CARTESIAN_POINT('Ctrl Pts',(-21.6627304262808,65.6975424912392,29.291657882429));
#16025=CARTESIAN_POINT('Ctrl Pts',(-21.5837244591008,65.3943632293128,29.3118354014677));
#16026=CARTESIAN_POINT('Ctrl Pts',(-21.4284374785815,65.1372559790479,29.3320129205065));
#16027=CARTESIAN_POINT('Ctrl Pts',(-21.1433425288428,64.6652268472649,29.3690572931703));
#16028=CARTESIAN_POINT('Ctrl Pts',(-20.601133764785,64.3484886605419,29.4061016658341));
#16029=CARTESIAN_POINT('Ctrl Pts',(-20.0499365874053,64.3319870464702,29.443146038498));
#16030=CARTESIAN_POINT('Ctrl Pts',(-19.4987394100257,64.3154854323984,29.4801904111618));
#16031=CARTESIAN_POINT('Ctrl Pts',(-18.9385538193242,64.599220390978,29.5172347838257));
#16032=CARTESIAN_POINT('Ctrl Pts',(-18.6257317659509,65.0533492213131,29.5542791564896));
#16033=CARTESIAN_POINT('Ctrl Pts',(-18.3129097125776,65.5074780516483,29.5913235291534));
#16034=CARTESIAN_POINT('Ctrl Pts',(-18.2474511965325,66.1320007537391,29.6283679018173));
#16035=CARTESIAN_POINT('Ctrl Pts',(-18.4593113229688,66.6411234486219,29.6654122744811));
#16036=CARTESIAN_POINT('Ctrl Pts',(-18.6711714494052,67.1502461435046,29.702456647145));
#16037=CARTESIAN_POINT('Ctrl Pts',(-19.160350218323,67.5439688311792,29.7395010198088));
#16038=CARTESIAN_POINT('Ctrl Pts',(-19.7029897981211,67.6421162613788,29.7765453924727));
#16039=CARTESIAN_POINT('Ctrl Pts',(-20.2456293779192,67.7402636915784,29.8135897651365));
#16040=CARTESIAN_POINT('Ctrl Pts',(-20.8417297685976,67.542835864303,29.8506341378004));
#16041=CARTESIAN_POINT('Ctrl Pts',(-21.2185037002406,67.1401796386557,29.8876785104642));
#16042=CARTESIAN_POINT('Ctrl Pts',(-21.5026166107437,66.8365497359656,29.9156124614396));
#16043=CARTESIAN_POINT('Ctrl Pts',(-21.6620166519365,66.4162233683915,29.9435464124149));
#16044=CARTESIAN_POINT('Ctrl Pts',(-21.6658100649286,65.9984774013953,29.9714803633902));
#16045=CARTESIAN_POINT('Origin',(-20.,66.,30.));
#16046=CARTESIAN_POINT('',(-21.6685540970378,66.0005306220524,30.6714803633902));
#16047=CARTESIAN_POINT('',(-21.6649961639659,66.0014338848797,30.4785196366098));
#16048=CARTESIAN_POINT('',(-21.666,66.,30.));
#16049=CARTESIAN_POINT('Ctrl Pts',(-21.6649961639659,66.0014338848797,30.4785196366098));
#16050=CARTESIAN_POINT('Ctrl Pts',(-21.6663488715524,66.1661251314864,30.4675206849354));
#16051=CARTESIAN_POINT('Ctrl Pts',(-21.6438880271777,66.3304555717191,30.4565217332609));
#16052=CARTESIAN_POINT('Ctrl Pts',(-21.596100259124,66.4870573839289,30.4455227815864));
#16053=CARTESIAN_POINT('Ctrl Pts',(-21.4351514759174,67.0144909124171,30.4084784089226));
#16054=CARTESIAN_POINT('Ctrl Pts',(-20.9869101567667,67.4542557934131,30.3714340362587));
#16055=CARTESIAN_POINT('Ctrl Pts',(-20.4565003506185,67.6051069628847,30.3343896635948));
#16056=CARTESIAN_POINT('Ctrl Pts',(-19.9260905444702,67.7559581323562,30.297345290931));
#16057=CARTESIAN_POINT('Ctrl Pts',(-19.3135122513245,67.6178955903034,30.2603009182671));
#16058=CARTESIAN_POINT('Ctrl Pts',(-18.8990933535481,67.2540994730139,30.2232565456033));
#16059=CARTESIAN_POINT('Ctrl Pts',(-18.4846744557717,66.8903033557244,30.1862121729394));
#16060=CARTESIAN_POINT('Ctrl Pts',(-18.2684149533647,66.3007736631982,30.1491678002756));
#16061=CARTESIAN_POINT('Ctrl Pts',(-18.3492794505739,65.7552907845666,30.1121234276117));
#16062=CARTESIAN_POINT('Ctrl Pts',(-18.4301439477832,65.209807905935,30.0750790549479));
#16063=CARTESIAN_POINT('Ctrl Pts',(-18.8081324446088,64.7083718411979,30.038034682284));
#16064=CARTESIAN_POINT('Ctrl Pts',(-19.3102699661622,64.4804496017448,30.0009903096202));
#16065=CARTESIAN_POINT('Ctrl Pts',(-19.8124074877155,64.2525273622916,29.9639459369563));
#16066=CARTESIAN_POINT('Ctrl Pts',(-20.4386940339967,64.2981189481223,29.9269015642924));
#16067=CARTESIAN_POINT('Ctrl Pts',(-20.9025285562284,64.5963607523271,29.8898571916286));
#16068=CARTESIAN_POINT('Ctrl Pts',(-21.3672163340203,64.8951511928785,29.852744673289));
#16069=CARTESIAN_POINT('Ctrl Pts',(-21.6688529243389,65.4475222434498,29.8156321549494));
#16070=CARTESIAN_POINT('Ctrl Pts',(-21.6687600243793,65.9999810464372,29.7785196366098));
#16071=CARTESIAN_POINT('Ctrl Pts',(-21.6658100649286,65.9984774013953,29.9714803633902));
#16072=CARTESIAN_POINT('Ctrl Pts',(-21.66704725447,65.8622330898984,29.9805907850787));
#16073=CARTESIAN_POINT('Ctrl Pts',(-21.6517328312273,65.7262632512288,29.9897012067673));
#16074=CARTESIAN_POINT('Ctrl Pts',(-21.6187950560616,65.5947057336016,29.9988116284558));
#16075=CARTESIAN_POINT('Ctrl Pts',(-21.4848650076323,65.0597726782143,30.0358560011197));
#16076=CARTESIAN_POINT('Ctrl Pts',(-21.0595574381662,64.5977911914591,30.0729003737835));
#16077=CARTESIAN_POINT('Ctrl Pts',(-20.5375014614225,64.4201730933822,30.1099447464474));
#16078=CARTESIAN_POINT('Ctrl Pts',(-20.0154454846788,64.2425549953053,30.1469891191112));
#16079=CARTESIAN_POINT('Ctrl Pts',(-19.3966411006575,64.3493002859068,30.1840334917751));
#16080=CARTESIAN_POINT('Ctrl Pts',(-18.9642653734382,64.6915602194806,30.2210778644389));
#16081=CARTESIAN_POINT('Ctrl Pts',(-18.531889646219,65.0338201530543,30.2581222371028));
#16082=CARTESIAN_POINT('Ctrl Pts',(-18.2859425758018,65.6115947296003,30.2951666097666));
#16083=CARTESIAN_POINT('Ctrl Pts',(-18.3389743818009,66.1604829323982,30.3322109824305));
#16084=CARTESIAN_POINT('Ctrl Pts',(-18.3920061877999,66.7093711351962,30.3692553550943));
#16085=CARTESIAN_POINT('Ctrl Pts',(-18.7440168702152,67.229372964246,30.4062997277582));
#16086=CARTESIAN_POINT('Ctrl Pts',(-19.2339194132707,67.4825253490384,30.443344100422));
#16087=CARTESIAN_POINT('Ctrl Pts',(-19.7238219563261,67.7356777338307,30.4803884730859));
#16088=CARTESIAN_POINT('Ctrl Pts',(-20.3516163600219,67.7219806743655,30.5174328457498));
#16089=CARTESIAN_POINT('Ctrl Pts',(-20.8300115503532,67.4477022146095,30.5544772184136));
#16090=CARTESIAN_POINT('Ctrl Pts',(-21.3084067406845,67.1734237548535,30.5915215910775));
#16091=CARTESIAN_POINT('Ctrl Pts',(-21.6374027176515,66.6385638948067,30.6285659637413));
#16092=CARTESIAN_POINT('Ctrl Pts',(-21.6664444476162,66.087885032366,30.6656103364051));
#16093=CARTESIAN_POINT('Ctrl Pts',(-21.6679784254409,66.0587982952976,30.6675670120668));
#16094=CARTESIAN_POINT('Ctrl Pts',(-21.6686755521249,66.0296674243309,30.6695236877285));
#16095=CARTESIAN_POINT('Ctrl Pts',(-21.6685540970378,66.0005306220524,30.6714803633902));
#16096=CARTESIAN_POINT('Origin',(-20.,66.,30.));
#16097=CARTESIAN_POINT('',(-21.6642459336481,66.0011866317831,31.3714803633902));
#16098=CARTESIAN_POINT('',(-21.6637024058618,65.9991726429868,31.1785196366098));
#16099=CARTESIAN_POINT('',(-21.666,66.,30.));
#16100=CARTESIAN_POINT('Ctrl Pts',(-21.6637024058618,65.9991726429868,31.1785196366098));
#16101=CARTESIAN_POINT('Ctrl Pts',(-21.6622143947745,66.3302224245355,31.1564535875851));
#16102=CARTESIAN_POINT('Ctrl Pts',(-21.566629777932,66.6620639402334,31.1343875385604));
#16103=CARTESIAN_POINT('Ctrl Pts',(-21.3827355500634,66.9342394398688,31.1123214895358));
#16104=CARTESIAN_POINT('Ctrl Pts',(-21.0740148406931,67.3911663064406,31.0752771168719));
#16105=CARTESIAN_POINT('Ctrl Pts',(-20.5164065063464,67.6799332993925,31.038232744208));
#16106=CARTESIAN_POINT('Ctrl Pts',(-19.9650830944454,67.6683949598707,31.0011883715442));
#16107=CARTESIAN_POINT('Ctrl Pts',(-19.4137596825443,67.6568566203489,30.9641439988803));
#16108=CARTESIAN_POINT('Ctrl Pts',(-18.868721193089,67.3450129483535,30.9270996262165));
#16109=CARTESIAN_POINT('Ctrl Pts',(-18.579387965107,66.8755697452132,30.8900552535526));
#16110=CARTESIAN_POINT('Ctrl Pts',(-18.290054737125,66.4061265420728,30.8530108808888));
#16111=CARTESIAN_POINT('Ctrl Pts',(-18.2564267706164,65.7790838077876,30.8159665082249));
#16112=CARTESIAN_POINT('Ctrl Pts',(-18.4938928848475,65.2813886376472,30.7789221355611));
#16113=CARTESIAN_POINT('Ctrl Pts',(-18.7313589990786,64.7836934675067,30.7418777628972));
#16114=CARTESIAN_POINT('Ctrl Pts',(-19.2399191940493,64.4153458615111,30.7048333902334));
#16115=CARTESIAN_POINT('Ctrl Pts',(-19.786846316174,64.3449089331741,30.6677890175695));
#16116=CARTESIAN_POINT('Ctrl Pts',(-20.3337734382987,64.2744720048371,30.6307446449057));
#16117=CARTESIAN_POINT('Ctrl Pts',(-20.9190674875773,64.5019457541587,30.5937002722418));
#16118=CARTESIAN_POINT('Ctrl Pts',(-21.2748863885853,64.9232337168097,30.556655899578));
#16119=CARTESIAN_POINT('Ctrl Pts',(-21.5250580720641,65.2194358537596,30.5306104785886));
#16120=CARTESIAN_POINT('Ctrl Pts',(-21.6617929642784,65.6114464589783,30.5045650575992));
#16121=CARTESIAN_POINT('Ctrl Pts',(-21.6649961639659,66.0014338848797,30.4785196366098));
#16122=CARTESIAN_POINT('Ctrl Pts',(-21.6685540970378,66.0005306220524,30.6714803633902));
#16123=CARTESIAN_POINT('Ctrl Pts',(-21.6663761278529,65.4780407122621,30.7065680603924));
#16124=CARTESIAN_POINT('Ctrl Pts',(-21.4009689299932,64.9536434858154,30.7416557573946));
#16125=CARTESIAN_POINT('Ctrl Pts',(-20.9776817958066,64.6476320093801,30.7767434543967));
#16126=CARTESIAN_POINT('Ctrl Pts',(-20.5307899310697,64.3245557136693,30.8137878270606));
#16127=CARTESIAN_POINT('Ctrl Pts',(-19.9079187186333,64.2449009870822,30.8508321997244));
#16128=CARTESIAN_POINT('Ctrl Pts',(-19.3941062832943,64.4451194000948,30.8878765723883));
#16129=CARTESIAN_POINT('Ctrl Pts',(-18.8802938479553,64.6453378131074,30.9249209450521));
#16130=CARTESIAN_POINT('Ctrl Pts',(-18.4755401897137,65.1254293657198,30.961965317716));
#16131=CARTESIAN_POINT('Ctrl Pts',(-18.3650685480553,65.6656947153468,30.9990096903798));
#16132=CARTESIAN_POINT('Ctrl Pts',(-18.2545969063969,66.2059600649738,31.0360540630437));
#16133=CARTESIAN_POINT('Ctrl Pts',(-18.4384072813217,66.8063992116154,31.0730984357075));
#16134=CARTESIAN_POINT('Ctrl Pts',(-18.8323844279111,67.1922393852412,31.1101428083714));
#16135=CARTESIAN_POINT('Ctrl Pts',(-19.2263615745004,67.5780795588669,31.1471871810352));
#16136=CARTESIAN_POINT('Ctrl Pts',(-19.8305054927545,67.7493207594768,31.1842315536991));
#16137=CARTESIAN_POINT('Ctrl Pts',(-20.3683480362437,67.6275996436778,31.2212759263629));
#16138=CARTESIAN_POINT('Ctrl Pts',(-20.9061905797328,67.5058785278788,31.2583202990268));
#16139=CARTESIAN_POINT('Ctrl Pts',(-21.3777317484572,67.091195095671,31.2953646716907));
#16140=CARTESIAN_POINT('Ctrl Pts',(-21.5671850237686,66.5733166465229,31.3324090443545));
#16141=CARTESIAN_POINT('Ctrl Pts',(-21.6337915358132,66.3912449610159,31.3454328173664));
#16142=CARTESIAN_POINT('Ctrl Pts',(-21.6655311270496,66.1964180578357,31.3584565903783));
#16143=CARTESIAN_POINT('Ctrl Pts',(-21.6642459336481,66.0011866317831,31.3714803633902));
#16144=CARTESIAN_POINT('Origin',(-20.,66.,30.));
#16145=CARTESIAN_POINT('',(-21.6642690977371,65.998802450892,32.0714803633902));
#16146=CARTESIAN_POINT('',(-21.6680157746037,65.999012657191,31.8785196366098));
#16147=CARTESIAN_POINT('',(-21.666,66.,30.));
#16148=CARTESIAN_POINT('Ctrl Pts',(-21.6680157746037,65.999012657191,31.8785196366098));
#16149=CARTESIAN_POINT('Ctrl Pts',(-21.664548415959,66.4928187802733,31.8453864902349));
#16150=CARTESIAN_POINT('Ctrl Pts',(-21.4314257129962,66.9894689300238,31.81225334386));
#16151=CARTESIAN_POINT('Ctrl Pts',(-21.0474729631797,67.2990617090127,31.7791201974851));
#16152=CARTESIAN_POINT('Ctrl Pts',(-20.6181962326036,67.6452005920857,31.7420758248213));
#16153=CARTESIAN_POINT('Ctrl Pts',(-20.000377985162,67.757512852679,31.7050314521574));
#16154=CARTESIAN_POINT('Ctrl Pts',(-19.4767440094288,67.5846021900613,31.6679870794935));
#16155=CARTESIAN_POINT('Ctrl Pts',(-18.9531100336955,67.4116915274435,31.6309427068297));
#16156=CARTESIAN_POINT('Ctrl Pts',(-18.5236603296707,66.9535579416147,31.5938983341658));
#16157=CARTESIAN_POINT('Ctrl Pts',(-18.3849195334037,66.4198523774313,31.556853961502));
#16158=CARTESIAN_POINT('Ctrl Pts',(-18.2461787371368,65.8861468132478,31.5198095888381));
#16159=CARTESIAN_POINT('Ctrl Pts',(-18.3981468486279,65.2768692707098,31.4827652161743));
#16160=CARTESIAN_POINT('Ctrl Pts',(-18.7712802693553,64.8708371437477,31.4457208435104));
#16161=CARTESIAN_POINT('Ctrl Pts',(-19.1444136900827,64.4648050167856,31.4086764708466));
#16162=CARTESIAN_POINT('Ctrl Pts',(-19.7387124200466,64.2620183053994,31.3716320981827));
#16163=CARTESIAN_POINT('Ctrl Pts',(-20.2822136647303,64.3552761995232,31.3345877255189));
#16164=CARTESIAN_POINT('Ctrl Pts',(-20.825714909414,64.4485340936469,31.297543352855));
#16165=CARTESIAN_POINT('Ctrl Pts',(-21.3184186688175,64.8378365932804,31.2604989801912));
#16166=CARTESIAN_POINT('Ctrl Pts',(-21.5348540063224,65.345031213193,31.2234546075273));
#16167=CARTESIAN_POINT('Ctrl Pts',(-21.6223663138332,65.5501075748318,31.2084762838881));
#16168=CARTESIAN_POINT('Ctrl Pts',(-21.6647124603405,65.7744577081488,31.193497960249));
#16169=CARTESIAN_POINT('Ctrl Pts',(-21.6637024058618,65.9991726429868,31.1785196366098));
#16170=CARTESIAN_POINT('Ctrl Pts',(-21.6642459336481,66.0011866317831,31.3714803633902));
#16171=CARTESIAN_POINT('Ctrl Pts',(-21.6618755670773,65.6411084946407,31.3955009630422));
#16172=CARTESIAN_POINT('Ctrl Pts',(-21.5471652967987,65.2796542982436,31.4195215626941));
#16173=CARTESIAN_POINT('Ctrl Pts',(-21.3316725937391,64.9943116889468,31.4435421623461));
#16174=CARTESIAN_POINT('Ctrl Pts',(-20.9993415064995,64.5542586466071,31.4805865350099));
#16175=CARTESIAN_POINT('Ctrl Pts',(-20.4273139501218,64.2952260280159,31.5176309076738));
#16176=CARTESIAN_POINT('Ctrl Pts',(-19.877360991797,64.3357522571528,31.5546752803376));
#16177=CARTESIAN_POINT('Ctrl Pts',(-19.3274080334722,64.3762784862898,31.5917196530015));
#16178=CARTESIAN_POINT('Ctrl Pts',(-18.7995296732003,64.7163635631548,31.6287640256653));
#16179=CARTESIAN_POINT('Ctrl Pts',(-18.5352934371866,65.2003778637654,31.6658083983292));
#16180=CARTESIAN_POINT('Ctrl Pts',(-18.2710572011729,65.6843921643761,31.7028527709931));
#16181=CARTESIAN_POINT('Ctrl Pts',(-18.2704630894175,66.3123356887323,31.7398971436569));
#16182=CARTESIAN_POINT('Ctrl Pts',(-18.5337829791516,66.7968491222805,31.7769415163208));
#16183=CARTESIAN_POINT('Ctrl Pts',(-18.7971028688856,67.2813625558288,31.8139858889846));
#16184=CARTESIAN_POINT('Ctrl Pts',(-19.3243367601092,67.622445898569,31.8510302616485));
#16185=CARTESIAN_POINT('Ctrl Pts',(-19.8742120483366,67.6640127004086,31.8880746343123));
#16186=CARTESIAN_POINT('Ctrl Pts',(-20.4240873365639,67.7055795022482,31.9251190069762));
#16187=CARTESIAN_POINT('Ctrl Pts',(-20.996604021795,67.4476297631871,31.96216337964));
#16188=CARTESIAN_POINT('Ctrl Pts',(-21.3297672018495,67.0082063602211,31.9992077523039));
#16189=CARTESIAN_POINT('Ctrl Pts',(-21.5464314453758,66.7224384696162,32.023298622666));
#16190=CARTESIAN_POINT('Ctrl Pts',(-21.6618677757111,66.3599213361594,32.0473894930281));
#16191=CARTESIAN_POINT('Ctrl Pts',(-21.6642690977371,65.998802450892,32.0714803633902));
#16192=CARTESIAN_POINT('Origin',(-20.,66.,30.));
#16193=CARTESIAN_POINT('',(-21.668567971344,65.9994875421907,32.7714803633902));
#16194=CARTESIAN_POINT('',(-21.6666947552498,66.0014544403163,32.5785196366098));
#16195=CARTESIAN_POINT('',(-21.666,66.,30.));
#16196=CARTESIAN_POINT('Ctrl Pts',(-21.6666947552498,66.0014544403163,32.5785196366098));
#16197=CARTESIAN_POINT('Ctrl Pts',(-21.6676729422518,66.1083233141787,32.5713637655485));
#16198=CARTESIAN_POINT('Ctrl Pts',(-21.6582744172421,66.2150208253731,32.5642078944873));
#16199=CARTESIAN_POINT('Ctrl Pts',(-21.6378750618295,66.3195719234416,32.557052023426));
#16200=CARTESIAN_POINT('Ctrl Pts',(-21.5322720796714,66.8608099930084,32.5200076507622));
#16201=CARTESIAN_POINT('Ctrl Pts',(-21.1318572413143,67.3445262197104,32.4829632780983));
#16202=CARTESIAN_POINT('Ctrl Pts',(-20.6198682568773,67.549362538766,32.4459189054344));
#16203=CARTESIAN_POINT('Ctrl Pts',(-20.1078792724403,67.7541988578216,32.4088745327706));
#16204=CARTESIAN_POINT('Ctrl Pts',(-19.4843161419233,67.6801552692307,32.3718301601068));
#16205=CARTESIAN_POINT('Ctrl Pts',(-19.034533625454,67.3611155762963,32.3347857874429));
#16206=CARTESIAN_POINT('Ctrl Pts',(-18.5847511089847,67.0420758833619,32.2977414147791));
#16207=CARTESIAN_POINT('Ctrl Pts',(-18.308749206563,66.4780400860841,32.2606970421152));
#16208=CARTESIAN_POINT('Ctrl Pts',(-18.3328318204015,65.9271220654133,32.2236526694513));
#16209=CARTESIAN_POINT('Ctrl Pts',(-18.35691443424,65.3762040447425,32.1866082967875));
#16210=CARTESIAN_POINT('Ctrl Pts',(-18.6810815643387,64.8384038006788,32.1495639241236));
#16211=CARTESIAN_POINT('Ctrl Pts',(-19.1569879524176,64.5598293087115,32.1125195514598));
#16212=CARTESIAN_POINT('Ctrl Pts',(-19.6328943404965,64.2812548167441,32.0754751787959));
#16213=CARTESIAN_POINT('Ctrl Pts',(-20.2605399865555,64.2619060768732,32.0384308061321));
#16214=CARTESIAN_POINT('Ctrl Pts',(-20.752701891012,64.510637453243,32.0013864334682));
#16215=CARTESIAN_POINT('Ctrl Pts',(-21.2448637954686,64.7593688296128,31.9643420608044));
#16216=CARTESIAN_POINT('Ctrl Pts',(-21.6015419583227,65.2761803222235,31.9272976881405));
#16217=CARTESIAN_POINT('Ctrl Pts',(-21.6595134328945,65.8245688213051,31.8902533154767));
#16218=CARTESIAN_POINT('Ctrl Pts',(-21.6656341886004,65.8824688843898,31.8863420891877));
#16219=CARTESIAN_POINT('Ctrl Pts',(-21.6684250814691,65.9407209553286,31.8824308628987));
#16220=CARTESIAN_POINT('Ctrl Pts',(-21.6680157746037,65.999012657191,31.8785196366098));
#16221=CARTESIAN_POINT('Ctrl Pts',(-21.6642690977371,65.998802450892,32.0714803633902));
#16222=CARTESIAN_POINT('Ctrl Pts',(-21.6655602727724,65.8046312050549,32.0844338656919));
#16223=CARTESIAN_POINT('Ctrl Pts',(-21.6341714211142,65.610864212633,32.0973873679937));
#16224=CARTESIAN_POINT('Ctrl Pts',(-21.5682670731027,65.4296498765436,32.1103408702954));
#16225=CARTESIAN_POINT('Ctrl Pts',(-21.3797940894235,64.911413862703,32.1473852429593));
#16226=CARTESIAN_POINT('Ctrl Pts',(-20.9090384471872,64.4958389018927,32.1844296156231));
#16227=CARTESIAN_POINT('Ctrl Pts',(-20.3714271926618,64.3731002746154,32.221473988287));
#16228=CARTESIAN_POINT('Ctrl Pts',(-19.8338159381365,64.250361647338,32.2585183609508));
#16229=CARTESIAN_POINT('Ctrl Pts',(-19.2293490713221,64.4204593535935,32.2955627336147));
#16230=CARTESIAN_POINT('Ctrl Pts',(-18.834642526265,64.8055533355086,32.3326071062785));
#16231=CARTESIAN_POINT('Ctrl Pts',(-18.4399359812079,65.1906473174238,32.3696514789424));
#16232=CARTESIAN_POINT('Ctrl Pts',(-18.254989757908,65.7907375749985,32.4066958516063));
#16233=CARTESIAN_POINT('Ctrl Pts',(-18.3644388878536,66.3312109967065,32.4437402242701));
#16234=CARTESIAN_POINT('Ctrl Pts',(-18.4738880177993,66.8716844184144,32.480784596934));
#16235=CARTESIAN_POINT('Ctrl Pts',(-18.8777325009904,67.3525410042557,32.5178289695978));
#16236=CARTESIAN_POINT('Ctrl Pts',(-19.3911651543367,67.5537313173818,32.5548733422616));
#16237=CARTESIAN_POINT('Ctrl Pts',(-19.904597807683,67.7549216305078,32.5919177149255));
#16238=CARTESIAN_POINT('Ctrl Pts',(-20.5276186311845,67.6764456709187,32.6289620875894));
#16239=CARTESIAN_POINT('Ctrl Pts',(-20.9751210350767,67.3542155821184,32.6660064602532));
#16240=CARTESIAN_POINT('Ctrl Pts',(-21.3998353421592,67.0483943670912,32.7011644279656));
#16241=CARTESIAN_POINT('Ctrl Pts',(-21.6664518819652,66.5230122439924,32.7363223956779));
#16242=CARTESIAN_POINT('Ctrl Pts',(-21.668567971344,65.9994875421907,32.7714803633902));
#16243=CARTESIAN_POINT('Origin',(-20.,66.,30.));
#16244=CARTESIAN_POINT('',(-21.6657785854137,66.0015219658715,33.4714803633902));
#16245=CARTESIAN_POINT('',(-21.6632990561475,66.0000736897326,33.2785196366098));
#16246=CARTESIAN_POINT('',(-21.666,66.,30.));
#16247=CARTESIAN_POINT('Ctrl Pts',(-21.6632990561475,66.0000736897326,33.2785196366098));
#16248=CARTESIAN_POINT('Ctrl Pts',(-21.6634069959719,66.2736326427316,33.2602966681983));
#16249=CARTESIAN_POINT('Ctrl Pts',(-21.5996813380736,66.5471442420865,33.2420736997869));
#16250=CARTESIAN_POINT('Ctrl Pts',(-21.4718464679376,66.7864025096638,33.2238507313754));
#16251=CARTESIAN_POINT('Ctrl Pts',(-21.2119786757195,67.2727762017491,33.1868063587115));
#16252=CARTESIAN_POINT('Ctrl Pts',(-20.6871836009889,67.6176001572505,33.1497619860477));
#16253=CARTESIAN_POINT('Ctrl Pts',(-20.1376177977875,67.6630761480344,33.1127176133838));
#16254=CARTESIAN_POINT('Ctrl Pts',(-19.5880519945861,67.7085521388184,33.07567324072));
#16255=CARTESIAN_POINT('Ctrl Pts',(-19.0137154629139,67.4546801648849,33.0386288680561));
#16256=CARTESIAN_POINT('Ctrl Pts',(-18.6774359025077,67.0176370376711,33.0015844953923));
#16257=CARTESIAN_POINT('Ctrl Pts',(-18.3411563421015,66.5805939104574,32.9645401227284));
#16258=CARTESIAN_POINT('Ctrl Pts',(-18.2429337529613,65.9603796299633,32.9274957500645));
#16259=CARTESIAN_POINT('Ctrl Pts',(-18.4277167248739,65.4408164566345,32.8904513774007));
#16260=CARTESIAN_POINT('Ctrl Pts',(-18.6124996967865,64.9212532833056,32.8534070047368));
#16261=CARTESIAN_POINT('Ctrl Pts',(-19.080288229752,64.5023412171419,32.816362632073));
#16262=CARTESIAN_POINT('Ctrl Pts',(-19.6170130850995,64.3757826637324,32.7793182594092));
#16263=CARTESIAN_POINT('Ctrl Pts',(-20.1537379404469,64.2492241103229,32.7422738867453));
#16264=CARTESIAN_POINT('Ctrl Pts',(-20.7593991181762,64.4150190696675,32.7052295140814));
#16265=CARTESIAN_POINT('Ctrl Pts',(-21.1568341440614,64.7972965055555,32.6681851414176));
#16266=CARTESIAN_POINT('Ctrl Pts',(-21.4774965430683,65.1057293101505,32.638296639815));
#16267=CARTESIAN_POINT('Ctrl Pts',(-21.6626090830058,65.5550866284368,32.6084081382124));
#16268=CARTESIAN_POINT('Ctrl Pts',(-21.6666947552498,66.0014544403163,32.5785196366098));
#16269=CARTESIAN_POINT('Ctrl Pts',(-21.668567971344,65.9994875421907,32.7714803633902));
#16270=CARTESIAN_POINT('Ctrl Pts',(-21.668681510372,65.9713977618654,32.7733667683417));
#16271=CARTESIAN_POINT('Ctrl Pts',(-21.6680335865054,65.9433133288179,32.7752531732932));
#16272=CARTESIAN_POINT('Ctrl Pts',(-21.6666077641248,65.9152684446987,32.7771395782448));
#16273=CARTESIAN_POINT('Ctrl Pts',(-21.6386081049976,65.3645356140905,32.8141839509086));
#16274=CARTESIAN_POINT('Ctrl Pts',(-21.31062480246,64.8290541708855,32.8512283235725));
#16275=CARTESIAN_POINT('Ctrl Pts',(-20.8327494704029,64.5538709616836,32.8882726962364));
#16276=CARTESIAN_POINT('Ctrl Pts',(-20.3548741383459,64.2786877524817,32.9253170689002));
#16277=CARTESIAN_POINT('Ctrl Pts',(-19.7271067767693,64.2638027772828,32.962361441564));
#16278=CARTESIAN_POINT('Ctrl Pts',(-19.2367260846697,64.5160276936372,32.9994058142279));
#16279=CARTESIAN_POINT('Ctrl Pts',(-18.74634539257,64.7682526099916,33.0364501868917));
#16280=CARTESIAN_POINT('Ctrl Pts',(-18.3933513699472,65.2875874178992,33.0734945595556));
#16281=CARTESIAN_POINT('Ctrl Pts',(-18.3392810284129,65.8363742889205,33.1105389322195));
#16282=CARTESIAN_POINT('Ctrl Pts',(-18.2852106868786,66.3851611599418,33.1475833048833));
#16283=CARTESIAN_POINT('Ctrl Pts',(-18.5300640264328,66.9634000940767,33.1846276775472));
#16284=CARTESIAN_POINT('Ctrl Pts',(-18.9617913402192,67.3064775752974,33.221672050211));
#16285=CARTESIAN_POINT('Ctrl Pts',(-19.3935186540056,67.6495550565182,33.2587164228749));
#16286=CARTESIAN_POINT('Ctrl Pts',(-20.0121199420242,67.7574710848249,33.2957607955387));
#16287=CARTESIAN_POINT('Ctrl Pts',(-20.534511080942,67.5808411621693,33.3328051682026));
#16288=CARTESIAN_POINT('Ctrl Pts',(-21.0569022198598,67.4042112395138,33.3698495408664));
#16289=CARTESIAN_POINT('Ctrl Pts',(-21.4830832096766,66.9430353658961,33.4068939135303));
#16290=CARTESIAN_POINT('Ctrl Pts',(-21.6180252422545,66.4083566963944,33.4439382861941));
#16291=CARTESIAN_POINT('Ctrl Pts',(-21.6514678734469,66.2758474907081,33.4531189785928));
#16292=CARTESIAN_POINT('Ctrl Pts',(-21.6670227490859,66.1388237789346,33.4622996709915));
#16293=CARTESIAN_POINT('Ctrl Pts',(-21.6657785854137,66.0015219658715,33.4714803633902));
#16294=CARTESIAN_POINT('Origin',(-20.,66.,30.));
#16295=CARTESIAN_POINT('',(-21.6633939316965,65.999580177356,34.1714803633902));
#16296=CARTESIAN_POINT('',(-21.6664242991574,65.998507036594,33.9785196366098));
#16297=CARTESIAN_POINT('',(-21.666,66.,30.));
#16298=CARTESIAN_POINT('Ctrl Pts',(-21.6664242991574,65.998507036594,33.9785196366098));
#16299=CARTESIAN_POINT('Ctrl Pts',(-21.6623854525421,66.4361202270654,33.9492295708481));
#16300=CARTESIAN_POINT('Ctrl Pts',(-21.4853948911407,66.8766244639417,33.9199395050864));
#16301=CARTESIAN_POINT('Ctrl Pts',(-21.1760642408071,67.1839061752964,33.8906494393247));
#16302=CARTESIAN_POINT('Ctrl Pts',(-20.7848408143887,67.5725382227907,33.8536050666609));
#16303=CARTESIAN_POINT('Ctrl Pts',(-20.1819298861659,67.7480712476131,33.816560693997));
#16304=CARTESIAN_POINT('Ctrl Pts',(-19.6432353607165,67.6301778814624,33.7795163213332));
#16305=CARTESIAN_POINT('Ctrl Pts',(-19.1045408352671,67.5122845153116,33.7424719486693));
#16306=CARTESIAN_POINT('Ctrl Pts',(-18.6300627125911,67.1009647581878,33.7054275760055));
#16307=CARTESIAN_POINT('Ctrl Pts',(-18.4369315199398,66.5844466264903,33.6683832033416));
#16308=CARTESIAN_POINT('Ctrl Pts',(-18.2438003272885,66.0679284947929,33.6313388306778));
#16309=CARTESIAN_POINT('Ctrl Pts',(-18.3320160646619,65.4462119885219,33.5942944580139));
#16310=CARTESIAN_POINT('Ctrl Pts',(-18.66120947423,65.0038068157843,33.5572500853501));
#16311=CARTESIAN_POINT('Ctrl Pts',(-18.990402883798,64.5614016430468,33.5202057126862));
#16312=CARTESIAN_POINT('Ctrl Pts',(-19.5605739655607,64.2983078038427,33.4831613400223));
#16313=CARTESIAN_POINT('Ctrl Pts',(-20.110801211816,64.3349222168409,33.4461169673585));
#16314=CARTESIAN_POINT('Ctrl Pts',(-20.6610284580713,64.3715366298392,33.4090725946946));
#16315=CARTESIAN_POINT('Ctrl Pts',(-21.1913118688192,64.7078592950398,33.3720282220308));
#16316=CARTESIAN_POINT('Ctrl Pts',(-21.4589833193403,65.1899823419746,33.3349838493669));
#16317=CARTESIAN_POINT('Ctrl Pts',(-21.5949811029387,65.4349381102391,33.3161624451146));
#16318=CARTESIAN_POINT('Ctrl Pts',(-21.6631875716174,65.7175311574189,33.2973410408622));
#16319=CARTESIAN_POINT('Ctrl Pts',(-21.6632990561475,66.0000736897326,33.2785196366098));
#16320=CARTESIAN_POINT('Ctrl Pts',(-21.6657785854137,66.0015219658715,33.4714803633902));
#16321=CARTESIAN_POINT('Ctrl Pts',(-21.662002510881,65.584806793107,33.4993440436554));
#16322=CARTESIAN_POINT('Ctrl Pts',(-21.5034836084249,65.1655299155204,33.5272077239205));
#16323=CARTESIAN_POINT('Ctrl Pts',(-21.220659016965,64.8621281087732,33.5550714041857));
#16324=CARTESIAN_POINT('Ctrl Pts',(-20.8446476837586,64.4587596560393,33.5921157768495));
#16325=CARTESIAN_POINT('Ctrl Pts',(-20.2489219420067,64.2602042159574,33.6291601495134));
#16326=CARTESIAN_POINT('Ctrl Pts',(-19.7060976147537,64.357324663287,33.6662045221773));
#16327=CARTESIAN_POINT('Ctrl Pts',(-19.1632732875006,64.4544451106166,33.7032488948411));
#16328=CARTESIAN_POINT('Ctrl Pts',(-18.6733503747463,64.8472414453578,33.7402932675049));
#16329=CARTESIAN_POINT('Ctrl Pts',(-18.4605272432548,65.3559623388724,33.7773376401688));
#16330=CARTESIAN_POINT('Ctrl Pts',(-18.2477041117633,65.8646832323871,33.8143820128327));
#16331=CARTESIAN_POINT('Ctrl Pts',(-18.3119807615347,66.4893286846752,33.8514263854965));
#16332=CARTESIAN_POINT('Ctrl Pts',(-18.6239429320858,66.9440486353022,33.8884707581604));
#16333=CARTESIAN_POINT('Ctrl Pts',(-18.9359051026368,67.3987685859291,33.9255151308242));
#16334=CARTESIAN_POINT('Ctrl Pts',(-19.4955527939675,67.6835630348949,33.9625595034881));
#16335=CARTESIAN_POINT('Ctrl Pts',(-20.0467802099533,67.6681044547283,33.9996038761519));
#16336=CARTESIAN_POINT('Ctrl Pts',(-20.5980076259392,67.6526458745618,34.0366482488158));
#16337=CARTESIAN_POINT('Ctrl Pts',(-21.1408147665801,67.3369342652628,34.0736926214796));
#16338=CARTESIAN_POINT('Ctrl Pts',(-21.4268023996106,66.865445438347,34.1107369941435));
#16339=CARTESIAN_POINT('Ctrl Pts',(-21.5831181109586,66.6077381011766,34.1309847838924));
#16340=CARTESIAN_POINT('Ctrl Pts',(-21.6627084923234,66.3034920156973,34.1512325736413));
#16341=CARTESIAN_POINT('Ctrl Pts',(-21.6633939316965,65.999580177356,34.1714803633902));
#16342=CARTESIAN_POINT('Origin',(-20.,66.,30.));
#16343=CARTESIAN_POINT('',(-21.6673174487995,65.9986976755605,34.8714803633902));
#16344=CARTESIAN_POINT('',(-21.6682089013646,66.0008588710179,34.6785196366098));
#16345=CARTESIAN_POINT('',(-21.666,66.,30.));
#16346=CARTESIAN_POINT('Ctrl Pts',(-21.6682089013646,66.0008588710179,34.6785196366098));
#16347=CARTESIAN_POINT('Ctrl Pts',(-21.6685189509142,66.0502166252967,34.6752068461617));
#16348=CARTESIAN_POINT('Ctrl Pts',(-21.6665182295093,66.0995488913109,34.6718940557137));
#16349=CARTESIAN_POINT('Ctrl Pts',(-21.6621249005774,66.1486671516306,34.6685812652656));
#16350=CARTESIAN_POINT('Ctrl Pts',(-21.6129977019998,66.697918656794,34.6315368926018));
#16351=CARTESIAN_POINT('Ctrl Pts',(-21.2646936272885,67.2204104220295,34.5944925199379));
#16352=CARTESIAN_POINT('Ctrl Pts',(-20.7766036444332,67.4770401441681,34.5574481472741));
#16353=CARTESIAN_POINT('Ctrl Pts',(-20.2885136615778,67.7336698663066,34.5204037746102));
#16354=CARTESIAN_POINT('Ctrl Pts',(-19.6606377705784,67.7244375453482,34.4833594019464));
#16355=CARTESIAN_POINT('Ctrl Pts',(-19.1803042509458,67.4535679671517,34.4463150292825));
#16356=CARTESIAN_POINT('Ctrl Pts',(-18.6999707313132,67.1826983889551,34.4092706566187));
#16357=CARTESIAN_POINT('Ctrl Pts',(-18.3671795830475,66.6501915535204,34.3722262839548));
#16358=CARTESIAN_POINT('Ctrl Pts',(-18.3342226273379,66.0997331214924,34.335181911291));
#16359=CARTESIAN_POINT('Ctrl Pts',(-18.3012656716283,65.5492746894643,34.2981375386271));
#16360=CARTESIAN_POINT('Ctrl Pts',(-18.5681429084748,64.9808646608429,34.2610931659633));
#16361=CARTESIAN_POINT('Ctrl Pts',(-19.0127260408984,64.6546186242835,34.2240487932994));
#16362=CARTESIAN_POINT('Ctrl Pts',(-19.4573091733219,64.3283725877241,34.1870044206356));
#16363=CARTESIAN_POINT('Ctrl Pts',(-20.0795982013227,64.2442905432266,34.1499600479717));
#16364=CARTESIAN_POINT('Ctrl Pts',(-20.5948214298447,64.4408501024346,34.1129156753078));
#16365=CARTESIAN_POINT('Ctrl Pts',(-21.1100446583667,64.6374096616425,34.075871302644));
#16366=CARTESIAN_POINT('Ctrl Pts',(-21.5182020874101,65.114610824556,34.0388269299802));
#16367=CARTESIAN_POINT('Ctrl Pts',(-21.6325128396248,65.6540769410959,34.0017825573163));
#16368=CARTESIAN_POINT('Ctrl Pts',(-21.6564409180656,65.7670005926563,33.9940282504141));
#16369=CARTESIAN_POINT('Ctrl Pts',(-21.6674935509796,65.8826525004193,33.986273943512));
#16370=CARTESIAN_POINT('Ctrl Pts',(-21.6664242991574,65.998507036594,33.9785196366098));
#16371=CARTESIAN_POINT('Ctrl Pts',(-21.6633939316965,65.999580177356,34.1714803633902));
#16372=CARTESIAN_POINT('Ctrl Pts',(-21.6639625389079,65.7474696776501,34.1882769463052));
#16373=CARTESIAN_POINT('Ctrl Pts',(-21.6102322705569,65.495589191975,34.2050735292201));
#16374=CARTESIAN_POINT('Ctrl Pts',(-21.5009588723762,65.270696659075,34.2218701121351));
#16375=CARTESIAN_POINT('Ctrl Pts',(-21.2599595866913,64.7747027512516,34.2589144847989));
#16376=CARTESIAN_POINT('Ctrl Pts',(-20.7487928899015,64.4099809801376,34.2959588574628));
#16377=CARTESIAN_POINT('Ctrl Pts',(-20.2013787127083,64.3434350705321,34.3330032301266));
#16378=CARTESIAN_POINT('Ctrl Pts',(-19.6539645355152,64.2768891609266,34.3700476027905));
#16379=CARTESIAN_POINT('Ctrl Pts',(-19.0703028779187,64.5085191128297,34.4070919754543));
#16380=CARTESIAN_POINT('Ctrl Pts',(-18.7174888195492,64.932326771598,34.4441363481182));
#16381=CARTESIAN_POINT('Ctrl Pts',(-18.3646747611796,65.3561344303663,34.481180720782));
#16382=CARTESIAN_POINT('Ctrl Pts',(-18.242708302037,65.9721197959998,34.5182250934459));
#16383=CARTESIAN_POINT('Ctrl Pts',(-18.4074036566907,66.4983953048516,34.5552694661097));
#16384=CARTESIAN_POINT('Ctrl Pts',(-18.5720990113444,67.0246708137035,34.5923138387736));
#16385=CARTESIAN_POINT('Ctrl Pts',(-19.0234561797943,67.4612364657736,34.6293582114375));
#16386=CARTESIAN_POINT('Ctrl Pts',(-19.554925313721,67.6083122994716,34.6664025841013));
#16387=CARTESIAN_POINT('Ctrl Pts',(-20.0863944476476,67.7553881331697,34.7034469567652));
#16388=CARTESIAN_POINT('Ctrl Pts',(-20.697975547051,67.6129741484956,34.740491329429));
#16389=CARTESIAN_POINT('Ctrl Pts',(-21.1097969163446,67.2462396496305,34.7775357020928));
#16390=CARTESIAN_POINT('Ctrl Pts',(-21.4579237371563,66.9362263169302,34.808850589192));
#16391=CARTESIAN_POINT('Ctrl Pts',(-21.6633041613515,66.4659156857186,34.8401654762911));
#16392=CARTESIAN_POINT('Ctrl Pts',(-21.6673174487995,65.9986976755605,34.8714803633902));
#16393=CARTESIAN_POINT('Origin',(-20.,66.,30.));
#16394=CARTESIAN_POINT('',(-21.6674772588494,66.0012131718681,35.5714803633902));
#16395=CARTESIAN_POINT('',(-21.6638441182547,66.0009441583361,35.3785196366098));
#16396=CARTESIAN_POINT('',(-21.666,66.,30.));
#16397=CARTESIAN_POINT('',(-18.7309291201476,67.0793586530486,36.));
#16398=CARTESIAN_POINT('Ctrl Pts',(-21.6674772588494,66.0012131718681,35.5714803633902));
#16399=CARTESIAN_POINT('Ctrl Pts',(-21.6635425119738,65.5283747294322,35.6031871242686));
#16400=CARTESIAN_POINT('Ctrl Pts',(-21.4523796053324,65.0525513983493,35.6348938851469));
#16401=CARTESIAN_POINT('Ctrl Pts',(-21.0965954523948,64.7422676947146,35.6666006460253));
#16402=CARTESIAN_POINT('Ctrl Pts',(-20.6809175217517,64.379749896285,35.7036450186892));
#16403=CARTESIAN_POINT('Ctrl Pts',(-20.0678279157583,64.2431978949171,35.740689391353));
#16404=CARTESIAN_POINT('Ctrl Pts',(-19.5379531300011,64.3961906766735,35.7777337640169));
#16405=CARTESIAN_POINT('Ctrl Pts',(-19.0080783442439,64.5491834584299,35.8147781366807));
#16406=CARTESIAN_POINT('Ctrl Pts',(-18.5614183787227,64.9917210233105,35.8518225093446));
#16407=CARTESIAN_POINT('Ctrl Pts',(-18.4024068180897,65.5187702873923,35.8888668820084));
#16408=CARTESIAN_POINT('Ctrl Pts',(-18.2433952574568,66.045819551474,35.9259112546723));
#16409=CARTESIAN_POINT('Ctrl Pts',(-18.372032101712,66.6573805147568,35.9629556273362));
#16410=CARTESIAN_POINT('Ctrl Pts',(-18.7309291201477,67.0793586530486,36.));
#16411=CARTESIAN_POINT('',(-21.2714721605028,67.0812049688959,36.));
#16412=CARTESIAN_POINT('Origin',(-20.,66.,36.));
#16413=CARTESIAN_POINT('Ctrl Pts',(-21.271473618129,67.0812060896471,36.));
#16414=CARTESIAN_POINT('Ctrl Pts',(-20.9206573555038,67.4926760200616,35.9636818543909));
#16415=CARTESIAN_POINT('Ctrl Pts',(-20.350790378308,67.7187175367081,35.9273637087819));
#16416=CARTESIAN_POINT('Ctrl Pts',(-19.8134508504095,67.6581953046217,35.8910455631728));
#16417=CARTESIAN_POINT('Ctrl Pts',(-19.2653665420103,67.5964628542926,35.854001190509));
#16418=CARTESIAN_POINT('Ctrl Pts',(-18.7511235436386,67.2365916665876,35.8169568178451));
#16419=CARTESIAN_POINT('Ctrl Pts',(-18.5057149733845,66.7428459347189,35.7799124451812));
#16420=CARTESIAN_POINT('Ctrl Pts',(-18.2603064031304,66.2491002028503,35.7428680725174));
#16421=CARTESIAN_POINT('Ctrl Pts',(-18.2837322609937,65.6214799268181,35.7058236998535));
#16422=CARTESIAN_POINT('Ctrl Pts',(-18.5654400102027,65.147406193219,35.6687793271897));
#16423=CARTESIAN_POINT('Ctrl Pts',(-18.8471477594117,64.6733324596199,35.6317349545258));
#16424=CARTESIAN_POINT('Ctrl Pts',(-19.3871373999664,64.352805268454,35.594690581862));
#16425=CARTESIAN_POINT('Ctrl Pts',(-19.9382150015654,64.3323990640615,35.5576462091981));
#16426=CARTESIAN_POINT('Ctrl Pts',(-20.4892926031645,64.3119928596691,35.5206018365343));
#16427=CARTESIAN_POINT('Ctrl Pts',(-21.051458165808,64.5917076420502,35.4835574638704));
#16428=CARTESIAN_POINT('Ctrl Pts',(-21.3674958173659,65.0435931347764,35.4465130912065));
#16429=CARTESIAN_POINT('Ctrl Pts',(-21.5608539458915,65.3200656776861,35.423848606341));
#16430=CARTESIAN_POINT('Ctrl Pts',(-21.6620805871735,65.6609857817599,35.4011841214754));
#16431=CARTESIAN_POINT('Ctrl Pts',(-21.6638441182547,66.0009441583361,35.3785196366098));
#16432=CARTESIAN_POINT('Origin',(-20.,66.,37.5459252805377));
#16433=CARTESIAN_POINT('',(-22.0554079166885,66.0018230931942,25.3540747194623));
#16434=CARTESIAN_POINT('',(-22.0529265634941,65.9984939060226,25.2959252805377));
#16435=CARTESIAN_POINT('',(-22.05475,66.0000000000002,37.5459252805377));
#16436=CARTESIAN_POINT('',(-18.1825721112405,66.9586205879593,25.));
#16437=CARTESIAN_POINT('Ctrl Pts',(-22.0529265634941,65.9984939060226,25.2959252805377));
#16438=CARTESIAN_POINT('Ctrl Pts',(-22.0499365185657,66.4524189410876,25.2713722656861));
#16439=CARTESIAN_POINT('Ctrl Pts',(-21.6783090895603,67.5959821141663,25.2097748781708));
#16440=CARTESIAN_POINT('Ctrl Pts',(-19.7840045183826,68.4179596733709,25.1111331179915));
#16441=CARTESIAN_POINT('Ctrl Pts',(-18.5013225746364,67.5629326473987,25.0370443726639));
#16442=CARTESIAN_POINT('Ctrl Pts',(-18.1825721112405,66.9586205879592,25.));
#16443=CARTESIAN_POINT('',(-17.9429021015473,65.924544644241,25.));
#16444=CARTESIAN_POINT('Origin',(-20.,66.,25.));
#16445=CARTESIAN_POINT('Ctrl Pts',(-22.0554079166885,66.0018230931942,25.3540747194623));
#16446=CARTESIAN_POINT('Ctrl Pts',(-22.0567024970405,66.1421866271351,25.3464567039117));
#16447=CARTESIAN_POINT('Ctrl Pts',(-21.9795741683388,66.9636910851773,25.3017943156971));
#16448=CARTESIAN_POINT('Ctrl Pts',(-20.8736248136923,68.2659592866881,25.2200875548188));
#16449=CARTESIAN_POINT('Ctrl Pts',(-18.5861502173631,67.9651132068328,25.109680663882));
#16450=CARTESIAN_POINT('Ctrl Pts',(-17.9193181049043,66.5910224347197,25.0363181456091));
#16451=CARTESIAN_POINT('Ctrl Pts',(-17.9428998421776,65.9245444497166,25.));
#16452=CARTESIAN_POINT('Origin',(-20.,66.,37.5459252805377));
#16453=CARTESIAN_POINT('',(-22.0514168260403,65.9999504085468,26.0540747194623));
#16454=CARTESIAN_POINT('',(-22.0580137571954,65.9995169080372,25.9959252805377));
#16455=CARTESIAN_POINT('',(-22.05475,66.0000000000002,37.5459252805377));
#16456=CARTESIAN_POINT('Ctrl Pts',(-22.0580137571954,65.9995169080372,25.9959252805377));
#16457=CARTESIAN_POINT('Ctrl Pts',(-22.055944731254,66.6536075471323,25.9603051683359));
#16458=CARTESIAN_POINT('Ctrl Pts',(-21.3649311540752,67.9917158703155,25.8876406834703));
#16459=CARTESIAN_POINT('Ctrl Pts',(-19.0858252973621,68.2499869305541,25.777931825941));
#16460=CARTESIAN_POINT('Ctrl Pts',(-17.6139705839552,66.4524069049006,25.6667987079493));
#16461=CARTESIAN_POINT('Ctrl Pts',(-18.3256043606965,64.2406215522943,25.5556655899578));
#16462=CARTESIAN_POINT('Ctrl Pts',(-20.5703082087302,63.6393771341005,25.4445324719662));
#16463=CARTESIAN_POINT('Ctrl Pts',(-21.9115053131723,64.8537201864073,25.3579523688262));
#16464=CARTESIAN_POINT('Ctrl Pts',(-22.0544477502527,65.767559331704,25.30841663835));
#16465=CARTESIAN_POINT('Ctrl Pts',(-22.0529265634941,65.9984939060226,25.2959252805377));
#16466=CARTESIAN_POINT('Ctrl Pts',(-22.0514168260403,65.9999504085468,26.0540747194623));
#16467=CARTESIAN_POINT('Ctrl Pts',(-22.0513428091222,66.3458999979507,26.0353896065614));
#16468=CARTESIAN_POINT('Ctrl Pts',(-21.8042540521266,67.3778154892877,25.9796601209967));
#16469=CARTESIAN_POINT('Ctrl Pts',(-20.1701400749251,68.4226485469194,25.8868862627681));
#16470=CARTESIAN_POINT('Ctrl Pts',(-18.0569489447748,67.4569397798106,25.7757531447766));
#16471=CARTESIAN_POINT('Ctrl Pts',(-17.7220731495743,65.1577888564038,25.664620026785));
#16472=CARTESIAN_POINT('Ctrl Pts',(-19.4721283434274,63.6294498117299,25.5534869087935));
#16473=CARTESIAN_POINT('Ctrl Pts',(-21.5520773549122,64.2267966310467,25.4499718063526));
#16474=CARTESIAN_POINT('Ctrl Pts',(-22.0504072989427,65.4596362929778,25.3835010765755));
#16475=CARTESIAN_POINT('Ctrl Pts',(-22.0554079166885,66.0018230931942,25.3540747194623));
#16476=CARTESIAN_POINT('Origin',(-20.,66.,37.5459252805377));
#16477=CARTESIAN_POINT('',(-22.0555312286582,65.9981936687081,26.7540747194623));
#16478=CARTESIAN_POINT('',(-22.0542236518071,66.0018654838724,26.6959252805377));
#16479=CARTESIAN_POINT('',(-22.05475,66.0000000000002,37.5459252805377));
#16480=CARTESIAN_POINT('Ctrl Pts',(-22.0542236518071,66.0018654838723,26.6959252805377));
#16481=CARTESIAN_POINT('Ctrl Pts',(-22.0558087689216,66.1797860011837,26.6862824436496));
#16482=CARTESIAN_POINT('Ctrl Pts',(-21.9531907145538,67.0394144619844,26.6395952340976));
#16483=CARTESIAN_POINT('Ctrl Pts',(-20.7492058435804,68.3101651333771,26.5558636518819));
#16484=CARTESIAN_POINT('Ctrl Pts',(-18.4655076477758,67.8824200236192,26.4447305338902));
#16485=CARTESIAN_POINT('Ctrl Pts',(-17.5862396422193,65.7318111728283,26.3335974158987));
#16486=CARTESIAN_POINT('Ctrl Pts',(-18.9161353509539,63.8266569879394,26.2224642979071));
#16487=CARTESIAN_POINT('Ctrl Pts',(-21.2380361565659,63.9106364641676,26.1113311799156));
#16488=CARTESIAN_POINT('Ctrl Pts',(-22.0457929795606,65.2670452373488,26.0358181741258));
#16489=CARTESIAN_POINT('Ctrl Pts',(-22.0580964866329,65.9733632723993,25.9973495409998));
#16490=CARTESIAN_POINT('Ctrl Pts',(-22.0580137571954,65.9995169080372,25.9959252805377));
#16491=CARTESIAN_POINT('Ctrl Pts',(-22.0555312286582,65.9981936687081,26.7540747194623));
#16492=CARTESIAN_POINT('Ctrl Pts',(-22.0505008107251,66.546259996983,26.7243225092112));
#16493=CARTESIAN_POINT('Ctrl Pts',(-21.5431050900676,67.7849445043772,26.6575259262963));
#16494=CARTESIAN_POINT('Ctrl Pts',(-19.4513023431397,68.3658195746722,26.5536849707175));
#16495=CARTESIAN_POINT('Ctrl Pts',(-17.714794155333,66.8221949683201,26.4425518527259));
#16496=CARTESIAN_POINT('Ctrl Pts',(-18.0697956411282,64.5260652687741,26.3314187347344));
#16497=CARTESIAN_POINT('Ctrl Pts',(-20.1913974446539,63.5789384432151,26.2202856167427));
#16498=CARTESIAN_POINT('Ctrl Pts',(-21.8105644780809,64.6343487755811,26.1278376116522));
#16499=CARTESIAN_POINT('Ctrl Pts',(-22.0514895521636,65.6600338979829,26.0724339792253));
#16500=CARTESIAN_POINT('Ctrl Pts',(-22.0514168260403,65.9999504085468,26.0540747194623));
#16501=CARTESIAN_POINT('Origin',(-20.,66.,37.5459252805377));
#16502=CARTESIAN_POINT('',(-22.0572927264517,66.0011828701741,27.4540747194623));
#16503=CARTESIAN_POINT('',(-22.0516085534354,65.9993486075168,27.3959252805377));
#16504=CARTESIAN_POINT('',(-22.05475,66.0000000000002,37.5459252805377));
#16505=CARTESIAN_POINT('Ctrl Pts',(-22.0516085534354,65.9993486075168,27.3959252805377));
#16506=CARTESIAN_POINT('Ctrl Pts',(-22.0505185253417,66.3826975370093,27.3752153462994));
#16507=CARTESIAN_POINT('Ctrl Pts',(-21.7633388146539,67.4532686773158,27.3174610393972));
#16508=CARTESIAN_POINT('Ctrl Pts',(-20.0378654061023,68.4283198539221,27.2226623598312));
#16509=CARTESIAN_POINT('Ctrl Pts',(-17.980425607167,67.3488848690413,27.1115292418396));
#16510=CARTESIAN_POINT('Ctrl Pts',(-17.7713798203235,65.0348973788296,27.0003961238481));
#16511=CARTESIAN_POINT('Ctrl Pts',(-19.6020548636007,63.6042097568846,26.8892630058565));
#16512=CARTESIAN_POINT('Ctrl Pts',(-21.6064981126984,64.3001233076535,26.787772724753));
#16513=CARTESIAN_POINT('Ctrl Pts',(-22.0497193089643,65.4962782301495,26.7233268163134));
#16514=CARTESIAN_POINT('Ctrl Pts',(-22.0542236518071,66.0018654838723,26.6959252805377));
#16515=CARTESIAN_POINT('Ctrl Pts',(-22.0572927264517,66.0011828701741,27.4540747194623));
#16516=CARTESIAN_POINT('Ctrl Pts',(-22.0577689201907,66.0705663114154,27.4502997845249));
#16517=CARTESIAN_POINT('Ctrl Pts',(-22.0231032579491,66.8203452154228,27.4094804769236));
#16518=CARTESIAN_POINT('Ctrl Pts',(-21.1033853710592,68.1634953045376,27.3316167966584));
#16519=CARTESIAN_POINT('Ctrl Pts',(-18.7808305400592,68.1004278233727,27.2204836786668));
#16520=CARTESIAN_POINT('Ctrl Pts',(-17.5741075901122,66.1149661254002,27.1093505606753));
#16521=CARTESIAN_POINT('Ctrl Pts',(-18.5876568453766,64.0242829060802,26.9982174426837));
#16522=CARTESIAN_POINT('Ctrl Pts',(-20.8938381659967,63.7418537313102,26.8870843246922));
#16523=CARTESIAN_POINT('Ctrl Pts',(-21.9835526554325,65.0484776377887,26.8057034169517));
#16524=CARTESIAN_POINT('Ctrl Pts',(-22.0567641664555,65.8638645333256,26.7613668818751));
#16525=CARTESIAN_POINT('Ctrl Pts',(-22.0555312286582,65.9981936687081,26.7540747194623));
#16526=CARTESIAN_POINT('Origin',(-20.,66.,37.5459252805377));
#16527=CARTESIAN_POINT('',(-22.0519546912208,66.0010551247961,28.1540747194623));
#16528=CARTESIAN_POINT('',(-22.0566098087376,65.9984792507726,28.0959252805377));
#16529=CARTESIAN_POINT('',(-22.05475,66.0000000000002,37.5459252805377));
#16530=CARTESIAN_POINT('Ctrl Pts',(-22.0566098087376,65.9984792507726,28.0959252805377));
#16531=CARTESIAN_POINT('Ctrl Pts',(-22.0517666752291,66.5830501214977,28.0641482489491));
#16532=CARTESIAN_POINT('Ctrl Pts',(-21.4848825436541,67.8572999709014,27.9953268446968));
#16533=CARTESIAN_POINT('Ctrl Pts',(-19.3231871914542,68.3324012329073,27.8894610677805));
#16534=CARTESIAN_POINT('Ctrl Pts',(-17.6733826257443,66.6964356994646,27.778327949789));
#16535=CARTESIAN_POINT('Ctrl Pts',(-18.1529898563275,64.4230648027232,27.6671948317974));
#16536=CARTESIAN_POINT('Ctrl Pts',(-20.3230534668011,63.5929670655095,27.5560617138059));
#16537=CARTESIAN_POINT('Ctrl Pts',(-21.8481481306761,64.7100347411471,27.4656385300526));
#16538=CARTESIAN_POINT('Ctrl Pts',(-22.0524682856091,65.6969918055957,27.4122597189632));
#16539=CARTESIAN_POINT('Ctrl Pts',(-22.0516085534354,65.9993486075168,27.3959252805377));
#16540=CARTESIAN_POINT('Ctrl Pts',(-22.0519546912208,66.0010551247961,28.1540747194623));
#16541=CARTESIAN_POINT('Ctrl Pts',(-22.0532325018955,66.2756710652459,28.1392326871747));
#16542=CARTESIAN_POINT('Ctrl Pts',(-21.8740722112356,67.2341046919512,28.0873462822231));
#16543=CARTESIAN_POINT('Ctrl Pts',(-20.4194990409278,68.3921103158831,27.9984155046077));
#16544=CARTESIAN_POINT('Ctrl Pts',(-18.2178370221936,67.6498685794103,27.8872823866162));
#16545=CARTESIAN_POINT('Ctrl Pts',(-17.647280706083,65.3976021808533,27.7761492686246));
#16546=CARTESIAN_POINT('Ctrl Pts',(-19.2300256897269,63.6966739765529,27.6650161506331));
#16547=CARTESIAN_POINT('Ctrl Pts',(-21.4397818870587,64.0900099051345,27.557657967579));
#16548=CARTESIAN_POINT('Ctrl Pts',(-22.0530959129415,65.3896893965474,27.4873441571887));
#16549=CARTESIAN_POINT('Ctrl Pts',(-22.0572927264517,66.0011828701741,27.4540747194623));
#16550=CARTESIAN_POINT('Origin',(-20.,66.,37.5459252805377));
#16551=CARTESIAN_POINT('',(-22.0534437738779,65.998246286058,28.8540747194623));
#16552=CARTESIAN_POINT('',(-22.0563385464768,66.0016161415221,28.7959252805377));
#16553=CARTESIAN_POINT('',(-22.05475,66.0000000000002,37.5459252805377));
#16554=CARTESIAN_POINT('Ctrl Pts',(-22.0563385464768,66.0016161415221,28.7959252805377));
#16555=CARTESIAN_POINT('Ctrl Pts',(-22.0572596900105,66.1083451864965,28.7901255242628));
#16556=CARTESIAN_POINT('Ctrl Pts',(-22.0011751206758,66.8958067777666,28.747281395324));
#16557=CARTESIAN_POINT('Ctrl Pts',(-20.9838410983712,68.2204116244866,28.6673928937214));
#16558=CARTESIAN_POINT('Ctrl Pts',(-18.6681747980826,68.0308650178038,28.5562597757299));
#16559=CARTESIAN_POINT('Ctrl Pts',(-17.5714473427131,65.9825908127564,28.4451266577384));
#16560=CARTESIAN_POINT('Ctrl Pts',(-18.6974268662034,63.9502501810978,28.3339935397467));
#16561=CARTESIAN_POINT('Ctrl Pts',(-21.015572590504,63.7939212610561,28.2228604217552));
#16562=CARTESIAN_POINT('Ctrl Pts',(-22.007159314054,65.1240507418666,28.1435043353522));
#16563=CARTESIAN_POINT('Ctrl Pts',(-22.0574126035484,65.9015811452894,28.101192621613));
#16564=CARTESIAN_POINT('Ctrl Pts',(-22.0566098087376,65.9984792507726,28.0959252805377));
#16565=CARTESIAN_POINT('Ctrl Pts',(-22.0534437738779,65.998246286058,28.8540747194623));
#16566=CARTESIAN_POINT('Ctrl Pts',(-22.0495560303119,66.4767579293803,28.8281655898244));
#16567=CARTESIAN_POINT('Ctrl Pts',(-21.6444560015232,67.6453699217003,28.7652120875227));
#16568=CARTESIAN_POINT('Ctrl Pts',(-19.6986309163782,68.4098439543111,28.665214212557));
#16569=CARTESIAN_POINT('Ctrl Pts',(-17.8119537217837,67.0538617998004,28.5540810945656));
#16570=CARTESIAN_POINT('Ctrl Pts',(-17.9278626016764,64.733343846516,28.442947976574));
#16571=CARTESIAN_POINT('Ctrl Pts',(-19.9402731870454,63.5721194600009,28.3318148585824));
#16572=CARTESIAN_POINT('Ctrl Pts',(-21.7312864460425,64.4913061059809,28.2355237728785));
#16573=CARTESIAN_POINT('Ctrl Pts',(-22.050043201811,65.590254469979,28.1762770598385));
#16574=CARTESIAN_POINT('Ctrl Pts',(-22.0519546912208,66.0010551247961,28.1540747194623));
#16575=CARTESIAN_POINT('Origin',(-20.,66.,37.5459252805377));
#16576=CARTESIAN_POINT('',(-22.0581541863218,65.9999766228665,29.5540747194623));
#16577=CARTESIAN_POINT('',(-22.051526238456,66.0004971808368,29.4959252805377));
#16578=CARTESIAN_POINT('',(-22.05475,66.0000000000002,37.5459252805377));
#16579=CARTESIAN_POINT('Ctrl Pts',(-22.051526238456,66.0004971808368,29.4959252805377));
#16580=CARTESIAN_POINT('Ctrl Pts',(-22.0522022874077,66.3127404725456,29.4790584269126));
#16581=CARTESIAN_POINT('Ctrl Pts',(-21.8385379867522,67.3098804665473,29.4251472006236));
#16582=CARTESIAN_POINT('Ctrl Pts',(-20.288512196013,68.4114169696994,29.3341916016708));
#16583=CARTESIAN_POINT('Ctrl Pts',(-18.1305721768482,67.5502937473358,29.2230584836793));
#16584=CARTESIAN_POINT('Ctrl Pts',(-17.683606081394,65.270280668443,29.1119253656876));
#16585=CARTESIAN_POINT('Ctrl Pts',(-19.3566948726244,63.6581354432645,29.0007922476961));
#16586=CARTESIAN_POINT('Ctrl Pts',(-21.5005207220627,64.1616337347749,28.8954588859794));
#16587=CARTESIAN_POINT('Ctrl Pts',(-22.0513761351298,65.4266423133588,28.8271698969266));
#16588=CARTESIAN_POINT('Ctrl Pts',(-22.0563385464768,66.0016161415221,28.7959252805377));
#16589=CARTESIAN_POINT('Ctrl Pts',(-22.0581540576791,65.9999766237499,29.5540747194623));
#16590=CARTESIAN_POINT('Ctrl Pts',(-22.0580399009054,66.6788457514294,29.5170984924742));
#16591=CARTESIAN_POINT('Ctrl Pts',(-21.31955436897,68.0380479292517,29.4430778928222));
#16592=CARTESIAN_POINT('Ctrl Pts',(-19.0043305992079,68.2151328748,29.3320129205065));
#16593=CARTESIAN_POINT('Ctrl Pts',(-17.5989621119428,66.3649496798285,29.2208798025149));
#16594=CARTESIAN_POINT('Ctrl Pts',(-18.391118003758,64.1807501735986,29.1097466845233));
#16595=CARTESIAN_POINT('Ctrl Pts',(-20.6557860235121,63.6615997134667,28.9986135665318));
#16596=CARTESIAN_POINT('Ctrl Pts',(-21.9322057363075,64.9047211795848,28.9133895781781));
#16597=CARTESIAN_POINT('Ctrl Pts',(-22.0551146509022,65.792591232661,28.8652099624883));
#16598=CARTESIAN_POINT('Ctrl Pts',(-22.0534437738779,65.998246286058,28.8540747194623));
#16599=CARTESIAN_POINT('Origin',(-20.,66.,37.5459252805377));
#16600=CARTESIAN_POINT('',(-22.0535119255156,66.0017684723631,30.2540747194623));
#16601=CARTESIAN_POINT('',(-22.0545157448452,65.9981221131555,30.1959252805377));
#16602=CARTESIAN_POINT('',(-22.05475,66.0000000000002,37.5459252805377));
#16603=CARTESIAN_POINT('Ctrl Pts',(-22.0545157448452,65.9981221131555,30.1959252805377));
#16604=CARTESIAN_POINT('Ctrl Pts',(-22.0498371642056,66.5133463182488,30.1679913295624));
#16605=CARTESIAN_POINT('Ctrl Pts',(-21.592529418229,67.7192337339074,30.1030130059232));
#16606=CARTESIAN_POINT('Ctrl Pts',(-19.5677489114844,68.3898389245888,30.0009903096202));
#16607=CARTESIAN_POINT('Ctrl Pts',(-17.7577727852529,66.9330531637854,29.8898571916286));
#16608=CARTESIAN_POINT('Ctrl Pts',(-17.9999712591612,64.6223004228711,29.7787240736371));
#16609=CARTESIAN_POINT('Ctrl Pts',(-20.0726747570493,63.5724725606719,29.6675909556455));
#16610=CARTESIAN_POINT('Ctrl Pts',(-21.7743809429352,64.56654600135,29.573324691279));
#16611=CARTESIAN_POINT('Ctrl Pts',(-22.0507174930375,65.626966046743,29.5161027995764));
#16612=CARTESIAN_POINT('Ctrl Pts',(-22.051526238456,66.0004971808368,29.4959252805377));
#16613=CARTESIAN_POINT('Ctrl Pts',(-22.0535119255156,66.0017684723631,30.2540747194623));
#16614=CARTESIAN_POINT('Ctrl Pts',(-22.0551802784048,66.2048893240828,30.2430757677879));
#16615=CARTESIAN_POINT('Ctrl Pts',(-21.9341784793424,67.090175672945,30.1950324434496));
#16616=CARTESIAN_POINT('Ctrl Pts',(-20.6643636219036,68.335977779557,30.1099447464473));
#16617=CARTESIAN_POINT('Ctrl Pts',(-18.3978055525618,67.8251422304279,29.9988116284558));
#16618=CARTESIAN_POINT('Ctrl Pts',(-17.5976389032744,65.643864675113,29.8876785104642));
#16619=CARTESIAN_POINT('Ctrl Pts',(-18.9962076857216,63.7885361864844,29.7765453924727));
#16620=CARTESIAN_POINT('Ctrl Pts',(-21.3134867030769,63.9572264223528,29.6654122744811));
#16621=CARTESIAN_POINT('Ctrl Pts',(-22.0575866779735,65.317354308492,29.5912553834777));
#16622=CARTESIAN_POINT('Ctrl Pts',(-22.0581542680654,65.9987254956813,29.5541428651381));
#16623=CARTESIAN_POINT('Ctrl Pts',(-22.0581540576791,65.9999766237499,29.5540747194623));
#16624=CARTESIAN_POINT('Origin',(-20.,66.,37.5459252805377));
#16625=CARTESIAN_POINT('',(-22.0519162775778,65.9989795847404,30.9540747194623));
#16626=CARTESIAN_POINT('',(-22.0579000785645,66.000654439173,30.8959252805377));
#16627=CARTESIAN_POINT('',(-22.05475,66.0000000000002,37.5459252805377));
#16628=CARTESIAN_POINT('Ctrl Pts',(-22.0579000785645,66.000654439173,30.8959252805377));
#16629=CARTESIAN_POINT('Ctrl Pts',(-22.058049874387,66.0365901201345,30.893968604876));
#16630=CARTESIAN_POINT('Ctrl Pts',(-22.0409121506992,66.7527251194839,30.8549675565505));
#16631=CARTESIAN_POINT('Ctrl Pts',(-21.2079497399452,68.1069002147157,30.778922135561));
#16632=CARTESIAN_POINT('Ctrl Pts',(-18.8850916049024,68.1575797458132,30.6677890175695));
#16633=CARTESIAN_POINT('Ctrl Pts',(-17.5826415154197,66.2335573720312,30.5566558995779));
#16634=CARTESIAN_POINT('Ctrl Pts',(-18.4926530573277,64.0957740986377,30.4455227815864));
#16635=CARTESIAN_POINT('Ctrl Pts',(-20.7822478497669,63.7008133197721,30.3343896635948));
#16636=CARTESIAN_POINT('Ctrl Pts',(-21.960352412273,64.9805048569412,30.2511904965786));
#16637=CARTESIAN_POINT('Ctrl Pts',(-22.0560416243231,65.830086099321,30.2050357022262));
#16638=CARTESIAN_POINT('Ctrl Pts',(-22.0545157448452,65.9981221131555,30.1959252805377));
#16639=CARTESIAN_POINT('Ctrl Pts',(-22.0519162775778,65.9989795847404,30.9540747194623));
#16640=CARTESIAN_POINT('Ctrl Pts',(-22.0500810490173,66.4072776271396,30.9320086704376));
#16641=CARTESIAN_POINT('Ctrl Pts',(-21.7342815225247,67.5036401694582,30.872898248749));
#16642=CARTESIAN_POINT('Ctrl Pts',(-19.9491839999498,68.4280833887723,30.7767434543968));
#16643=CARTESIAN_POINT('Ctrl Pts',(-17.9325252312672,67.2742524433354,30.6656103364051));
#16644=CARTESIAN_POINT('Ctrl Pts',(-17.8081007459427,64.9541755076705,30.5544772184136));
#16645=CARTESIAN_POINT('Ctrl Pts',(-19.6897887302455,63.5912783106364,30.4433441004221));
#16646=CARTESIAN_POINT('Ctrl Pts',(-21.6410622125122,64.3496381393588,30.3432099341049));
#16647=CARTESIAN_POINT('Ctrl Pts',(-22.0495612805229,65.5207800789832,30.2801201404517));
#16648=CARTESIAN_POINT('Ctrl Pts',(-22.0535119255156,66.0017684723631,30.2540747194623));
#16649=CARTESIAN_POINT('Origin',(-20.,66.,37.5459252805377));
#16650=CARTESIAN_POINT('',(-22.057236142177,65.998782267325,31.6540747194623));
#16651=CARTESIAN_POINT('',(-22.0525866339517,66.0014635244036,31.5959252805377));
#16652=CARTESIAN_POINT('',(-22.05475,66.0000000000002,37.5459252805377));
#16653=CARTESIAN_POINT('Ctrl Pts',(-22.0525866339517,66.0014635244036,31.5959252805377));
#16654=CARTESIAN_POINT('Ctrl Pts',(-22.0541717186706,66.2422509029639,31.5829015075258));
#16655=CARTESIAN_POINT('Ctrl Pts',(-21.9036808981398,67.1660076174918,31.5328333618501));
#16656=CARTESIAN_POINT('Ctrl Pts',(-20.5360719551439,68.3687122974119,31.4457208435104));
#16657=CARTESIAN_POINT('Ctrl Pts',(-18.3007213260338,67.7351147158636,31.3345877255189));
#16658=CARTESIAN_POINT('Ctrl Pts',(-17.6206174222944,65.513471852907,31.2234546075273));
#16659=CARTESIAN_POINT('Ctrl Pts',(-19.1182181052569,63.7371186997313,31.1123214895358));
#16660=CARTESIAN_POINT('Ctrl Pts',(-21.3822833862681,64.0266544774867,31.0031450472059));
#16661=CARTESIAN_POINT('Ctrl Pts',(-22.0552138947814,65.3562449901084,30.9310129775399));
#16662=CARTESIAN_POINT('Ctrl Pts',(-22.0579000785645,66.000654439173,30.8959252805377));
#16663=CARTESIAN_POINT('Ctrl Pts',(-22.057236142177,65.998782267325,31.6540747194623));
#16664=CARTESIAN_POINT('Ctrl Pts',(-22.0529596984944,66.6078147591637,31.6209415730874));
#16665=CARTESIAN_POINT('Ctrl Pts',(-21.443978487402,67.9052028120665,31.5507640540487));
#16666=CARTESIAN_POINT('Ctrl Pts',(-19.2384841663151,68.3061363454358,31.4435421623461));
#16667=CARTESIAN_POINT('Ctrl Pts',(-17.6495073727765,66.611028328362,31.3324090443545));
#16668=CARTESIAN_POINT('Ctrl Pts',(-18.2117939461611,64.3566831353306,31.221275926363));
#16669=CARTESIAN_POINT('Ctrl Pts',(-20.4107170831235,63.6063662171661,31.1101428083713));
#16670=CARTESIAN_POINT('Ctrl Pts',(-21.8717660929245,64.7607922201078,31.0210757394046));
#16671=CARTESIAN_POINT('Ctrl Pts',(-22.0531620215394,65.7218289170582,30.9690530431015));
#16672=CARTESIAN_POINT('Ctrl Pts',(-22.0519162775778,65.9989795847404,30.9540747194623));
#16673=CARTESIAN_POINT('Origin',(-20.,66.,37.5459252805377));
#16674=CARTESIAN_POINT('',(-22.0556068717584,66.0017938242738,32.3540747194623));
#16675=CARTESIAN_POINT('',(-22.0526152032265,65.9985230107867,32.2959252805377));
#16676=CARTESIAN_POINT('',(-22.05475,66.0000000000002,37.5459252805377));
#16677=CARTESIAN_POINT('Ctrl Pts',(-22.0526152032265,65.9985230107867,32.2959252805377));
#16678=CARTESIAN_POINT('Ctrl Pts',(-22.0496535487049,66.4439065819169,32.2718344101756));
#16679=CARTESIAN_POINT('Ctrl Pts',(-21.6883554661722,67.5785298398012,32.2106991671496));
#16680=CARTESIAN_POINT('Ctrl Pts',(-19.8169356517564,68.4217057074312,32.1125195514598));
#16681=CARTESIAN_POINT('Ctrl Pts',(-17.866154430883,67.1596871026972,32.0013864334682));
#16682=CARTESIAN_POINT('Ctrl Pts',(-17.8683526622086,64.8362772167352,31.8902533154766));
#16683=CARTESIAN_POINT('Ctrl Pts',(-19.8215184379026,63.5779522256995,31.7791201974851));
#16684=CARTESIAN_POINT('Ctrl Pts',(-21.6900011086861,64.4240617419441,31.6810108525054));
#16685=CARTESIAN_POINT('Ctrl Pts',(-22.0496631581345,65.557363553039,31.6199458801896));
#16686=CARTESIAN_POINT('Ctrl Pts',(-22.0525866339517,66.0014635244036,31.5959252805377));
#16687=CARTESIAN_POINT('Ctrl Pts',(-22.0556068717584,66.0017938242738,32.3540747194623));
#16688=CARTESIAN_POINT('Ctrl Pts',(-22.05681331218,66.1335998378205,32.3469188484011));
#16689=CARTESIAN_POINT('Ctrl Pts',(-21.98521449447,66.9464311753166,32.302718604676));
#16690=CARTESIAN_POINT('Ctrl Pts',(-20.9021196143316,68.2548506403159,32.221473988287));
#16691=CARTESIAN_POINT('Ctrl Pts',(-18.5949173170392,67.9808871403329,32.1103408702954));
#16692=CARTESIAN_POINT('Ctrl Pts',(-17.5737019947084,65.8939377625597,31.9992077523039));
#16693=CARTESIAN_POINT('Ctrl Pts',(-18.7731301049792,63.9040607190605,31.8880746343123));
#16694=CARTESIAN_POINT('Ctrl Pts',(-21.0954378323017,63.8324698008436,31.7769415163208));
#16695=CARTESIAN_POINT('Ctrl Pts',(-22.0216974132697,65.1745805506422,31.6989415447041));
#16696=CARTESIAN_POINT('Ctrl Pts',(-22.0577409580724,65.9268885852111,31.6579859457513));
#16697=CARTESIAN_POINT('Ctrl Pts',(-22.057236142177,65.998782267325,31.6540747194623));
#16698=CARTESIAN_POINT('Origin',(-20.,66.,37.5459252805377));
#16699=CARTESIAN_POINT('',(-22.051418808895,66.0000908847409,33.0540747194623));
#16700=CARTESIAN_POINT('',(-22.0579171903476,65.9993679635754,32.9959252805377));
#16701=CARTESIAN_POINT('',(-22.05475,66.0000000000002,37.5459252805377));
#16702=CARTESIAN_POINT('Ctrl Pts',(-22.0579171903476,65.9993679635754,32.9959252805377));
#16703=CARTESIAN_POINT('Ctrl Pts',(-22.055307325611,66.6450536664726,32.9607673128253));
#16704=CARTESIAN_POINT('Ctrl Pts',(-21.3800044610758,67.9757740072377,32.8885649724492));
#16705=CARTESIAN_POINT('Ctrl Pts',(-19.1139377600523,68.2612087024321,32.7793182594091));
#16706=CARTESIAN_POINT('Ctrl Pts',(-17.6197010520624,66.4820249033491,32.6681851414176));
#16707=CARTESIAN_POINT('Ctrl Pts',(-18.304007628879,64.2616729404111,32.557052023426));
#16708=CARTESIAN_POINT('Ctrl Pts',(-20.5405531773546,63.6323063222924,32.4459189054345));
#16709=CARTESIAN_POINT('Ctrl Pts',(-21.9047824951618,64.8366244321949,32.358876657805));
#16710=CARTESIAN_POINT('Ctrl Pts',(-22.0542076653537,65.7590431984314,32.3088787828394));
#16711=CARTESIAN_POINT('Ctrl Pts',(-22.0526152032265,65.9985230107867,32.2959252805377));
#16712=CARTESIAN_POINT('Ctrl Pts',(-22.051418808895,66.0000908847409,33.0540747194623));
#16713=CARTESIAN_POINT('Ctrl Pts',(-22.0515519357582,66.3374829967905,33.0358517510508));
#16714=CARTESIAN_POINT('Ctrl Pts',(-21.813184036767,67.3605620427844,32.9805844099755));
#16715=CARTESIAN_POINT('Ctrl Pts',(-20.2002808069203,68.4203427044879,32.8882726962364));
#16716=CARTESIAN_POINT('Ctrl Pts',(-18.0752184027424,67.4810087817272,32.7771395782448));
#16717=CARTESIAN_POINT('Ctrl Pts',(-17.7117918750668,65.1861973300252,32.6660064602532));
#16718=CARTESIAN_POINT('Ctrl Pts',(-19.4426234863108,63.6362101128286,32.5548733422617));
#16719=CARTESIAN_POINT('Ctrl Pts',(-21.5392921211705,64.2101565763925,32.4508960953313));
#16720=CARTESIAN_POINT('Ctrl Pts',(-22.0505678351178,65.4512690574914,32.3839632210649));
#16721=CARTESIAN_POINT('Ctrl Pts',(-22.0556068717584,66.0017938242738,32.3540747194623));
#16722=CARTESIAN_POINT('Origin',(-20.,66.,37.5459252805377));
#16723=CARTESIAN_POINT('',(-22.0552733065389,65.9981586635305,33.7540747194623));
#16724=CARTESIAN_POINT('',(-22.0544769197952,66.0018771064673,33.6959252805377));
#16725=CARTESIAN_POINT('',(-22.05475,66.0000000000002,37.5459252805377));
#16726=CARTESIAN_POINT('Ctrl Pts',(-22.0544769197952,66.0018771064673,33.6959252805377));
#16727=CARTESIAN_POINT('Ctrl Pts',(-22.0560114007709,66.1712173828127,33.686744588139));
#16728=CARTESIAN_POINT('Ctrl Pts',(-21.9594168493607,67.0221238303151,33.6405195230764));
#16729=CARTESIAN_POINT('Ctrl Pts',(-20.7778958267891,68.3006627675311,33.5572500853501));
#16730=CARTESIAN_POINT('Ctrl Pts',(-18.4890524956552,67.9013702240204,33.4461169673585));
#16731=CARTESIAN_POINT('Ctrl Pts',(-17.5830877907652,65.7618688136113,33.334983849367));
#16732=CARTESIAN_POINT('Ctrl Pts',(-18.8891762685279,63.8403144380744,33.2238507313753));
#16733=CARTESIAN_POINT('Ctrl Pts',(-21.2119343469181,63.8953892930382,33.1127176133839));
#16734=CARTESIAN_POINT('Ctrl Pts',(-22.0415654965746,65.2498853356985,33.0367424631046));
#16735=CARTESIAN_POINT('Ctrl Pts',(-22.0580572229514,65.9647236201639,32.9978116854892));
#16736=CARTESIAN_POINT('Ctrl Pts',(-22.0579171903476,65.9993679635754,32.9959252805377));
#16737=CARTESIAN_POINT('Ctrl Pts',(-22.0552733065389,65.9981586635305,33.7540747194623));
#16738=CARTESIAN_POINT('Ctrl Pts',(-22.0502920219753,66.5378859763281,33.7247846537006));
#16739=CARTESIAN_POINT('Ctrl Pts',(-21.5559212245969,67.7683043054681,33.6584502152751));
#16740=CARTESIAN_POINT('Ctrl Pts',(-19.4807858366348,68.3724645130774,33.5550714041857));
#16741=CARTESIAN_POINT('Ctrl Pts',(-17.7252025426939,66.8505690671885,33.4439382861941));
#16742=CARTESIAN_POINT('Ctrl Pts',(-18.0516034185067,64.550199335027,33.3328051682026));
#16743=CARTESIAN_POINT('Ctrl Pts',(-20.1612535330058,63.5767442339982,33.221672050211));
#16744=CARTESIAN_POINT('Ctrl Pts',(-21.8015900293923,64.6170979978703,33.1287619006309));
#16745=CARTESIAN_POINT('Ctrl Pts',(-22.0512813101927,65.651618934998,33.0728961237147));
#16746=CARTESIAN_POINT('Ctrl Pts',(-22.051418808895,66.0000908847409,33.0540747194623));
#16747=CARTESIAN_POINT('Origin',(-20.,66.,37.5459252805377));
#16748=CARTESIAN_POINT('',(-22.0574743337809,66.0010592828478,34.4540747194623));
#16749=CARTESIAN_POINT('',(-22.0515358230213,65.9994822145391,34.3959252805377));
#16750=CARTESIAN_POINT('',(-22.05475,66.0000000000002,37.5459252805377));
#16751=CARTESIAN_POINT('Ctrl Pts',(-22.0515358230213,65.9994822145391,34.3959252805377));
#16752=CARTESIAN_POINT('Ctrl Pts',(-22.0506904409372,66.3743098554946,34.3756774907888));
#16753=CARTESIAN_POINT('Ctrl Pts',(-21.7729352593099,67.4360704009606,34.318385328376));
#16754=CARTESIAN_POINT('Ctrl Pts',(-20.0680811507602,68.427660588213,34.2240487932995));
#16755=CARTESIAN_POINT('Ctrl Pts',(-17.9973678966875,67.3739125797871,34.1129156753078));
#16756=CARTESIAN_POINT('Ctrl Pts',(-17.7595423634621,65.0627056594589,34.0017825573163));
#16757=CARTESIAN_POINT('Ctrl Pts',(-19.572271844222,63.6093474323109,33.8906494393247));
#16758=CARTESIAN_POINT('Ctrl Pts',(-21.5943860347699,64.2833182629478,33.7886970137319));
#16759=CARTESIAN_POINT('Ctrl Pts',(-22.0498197234289,65.4879242245718,33.7237889608028));
#16760=CARTESIAN_POINT('Ctrl Pts',(-22.0544769197952,66.0018771064673,33.6959252805377));
#16761=CARTESIAN_POINT('Ctrl Pts',(-22.0574743337809,66.0010592828478,34.4540747194623));
#16762=CARTESIAN_POINT('Ctrl Pts',(-22.0578567313271,66.0619343402333,34.4507619290143));
#16763=CARTESIAN_POINT('Ctrl Pts',(-22.0277961568906,66.8031451110045,34.4104047659024));
#16764=CARTESIAN_POINT('Ctrl Pts',(-21.1302229490745,68.1495968002898,34.3330032301266));
#16765=CARTESIAN_POINT('Ctrl Pts',(-18.8070633085623,68.1154369356633,34.2218701121351));
#16766=CARTESIAN_POINT('Ctrl Pts',(-17.5757260722497,66.1451456629571,34.1107369941435));
#16767=CARTESIAN_POINT('Ctrl Pts',(-18.5631798581025,64.0420114979335,33.999603876152));
#16768=CARTESIAN_POINT('Ctrl Pts',(-20.8656679378464,63.730905409822,33.8884707581604));
#16769=CARTESIAN_POINT('Ctrl Pts',(-21.9778381799678,65.0312098882729,33.8066277059305));
#16770=CARTESIAN_POINT('Ctrl Pts',(-22.0565920611496,65.8552702432393,33.7618290263645));
#16771=CARTESIAN_POINT('Ctrl Pts',(-22.0552733065389,65.9981586635305,33.7540747194623));
#16772=CARTESIAN_POINT('Origin',(-20.,66.,37.5459252805377));
#16773=CARTESIAN_POINT('',(-22.0520910576133,66.0011644713934,35.1540747194623));
#16774=CARTESIAN_POINT('',(-22.0563748666992,65.9983937868295,35.0959252805377));
#16775=CARTESIAN_POINT('',(-22.05475,66.0000000000002,37.5459252805377));
#16776=CARTESIAN_POINT('Ctrl Pts',(-22.0563748666992,65.9983937868295,35.0959252805377));
#16777=CARTESIAN_POINT('Ctrl Pts',(-22.0514251053644,66.5746340067409,35.0646103934386));
#16778=CARTESIAN_POINT('Ctrl Pts',(-21.4984704235166,67.840871850344,34.9962511336756));
#16779=CARTESIAN_POINT('Ctrl Pts',(-19.3522645421998,68.3406415976227,34.8908475012488));
#16780=CARTESIAN_POINT('Ctrl Pts',(-17.6822294728015,66.7253355827527,34.7797143832572));
#16781=CARTESIAN_POINT('Ctrl Pts',(-18.1335090320871,64.4461712429531,34.6685812652656));
#16782=CARTESIAN_POINT('Ctrl Pts',(-20.2930746820505,63.5891334692323,34.5574481472741));
#16783=CARTESIAN_POINT('Ctrl Pts',(-21.8398173954859,64.6927475063844,34.4665628190315));
#16784=CARTESIAN_POINT('Ctrl Pts',(-22.0522371109369,65.6885434094548,34.4127218634526));
#16785=CARTESIAN_POINT('Ctrl Pts',(-22.0515358230213,65.9994822145391,34.3959252805377));
#16786=CARTESIAN_POINT('Ctrl Pts',(-22.0520910576133,66.0011644713934,35.1540747194623));
#16787=CARTESIAN_POINT('Ctrl Pts',(-22.0534710502056,66.2671875919197,35.1396948316641));
#16788=CARTESIAN_POINT('Ctrl Pts',(-21.8818112896055,67.2168117035418,35.088270571202));
#16789=CARTESIAN_POINT('Ctrl Pts',(-20.4492273182073,68.3866955695652,34.999801938076));
#16790=CARTESIAN_POINT('Ctrl Pts',(-18.2385101136685,67.6719231463612,34.8886688200844));
#16791=CARTESIAN_POINT('Ctrl Pts',(-17.6399646371577,65.4269244123525,34.7775357020929));
#16792=CARTESIAN_POINT('Ctrl Pts',(-19.2014230092252,63.706435258535,34.6664025841013));
#16793=CARTESIAN_POINT('Ctrl Pts',(-21.4254341990431,64.0738149167194,34.5585822565578));
#16794=CARTESIAN_POINT('Ctrl Pts',(-22.053580675407,65.3812156690452,34.4878063016781));
#16795=CARTESIAN_POINT('Ctrl Pts',(-22.0574743337809,66.0010592828478,34.4540747194623));
#16796=CARTESIAN_POINT('Origin',(-20.,66.,37.5459252805377));
#16797=CARTESIAN_POINT('',(-22.0526727182563,65.9976789726186,35.8540747194623));
#16798=CARTESIAN_POINT('',(-22.0565719673595,66.0014962574405,35.7959252805377));
#16799=CARTESIAN_POINT('',(-22.05475,66.0000000000002,37.5459252805377));
#16800=CARTESIAN_POINT('',(-20.5301702171886,64.0148256743283,36.));
#16801=CARTESIAN_POINT('Ctrl Pts',(-20.5301702171886,64.0148256743283,36.));
#16802=CARTESIAN_POINT('Ctrl Pts',(-21.1902595624181,64.1911123142463,35.9629556273362));
#16803=CARTESIAN_POINT('Ctrl Pts',(-21.9249295035175,64.8872096289435,35.9143138671569));
#16804=CARTESIAN_POINT('Ctrl Pts',(-22.0542897965232,65.7834100791695,35.8656721069777));
#16805=CARTESIAN_POINT('Ctrl Pts',(-22.0526727182563,65.9976789726186,35.8540747194623));
#16806=CARTESIAN_POINT('',(-19.4686891477661,64.0112682321016,36.));
#16807=CARTESIAN_POINT('Origin',(-20.,66.,36.));
#16808=CARTESIAN_POINT('Ctrl Pts',(-19.4686884555735,64.0112660732732,36.));
#16809=CARTESIAN_POINT('Ctrl Pts',(-20.1132090364839,63.839970256324,35.9636818543909));
#16810=CARTESIAN_POINT('Ctrl Pts',(-21.4929688632731,64.1592659283774,35.8956569479034));
#16811=CARTESIAN_POINT('Ctrl Pts',(-22.0517190735163,65.4183241148264,35.8276320414161));
#16812=CARTESIAN_POINT('Ctrl Pts',(-22.0565719673595,66.0014962574405,35.7959252805377));
#16813=CARTESIAN_POINT('Origin',(20.,66.,30.));
#16814=CARTESIAN_POINT('',(18.3313535993656,65.999608307577,25.7714803633902));
#16815=CARTESIAN_POINT('',(18.3334665914316,66.0014781595158,25.5785196366098));
#16816=CARTESIAN_POINT('',(18.334,66.,30.));
#16817=CARTESIAN_POINT('',(19.2300979593296,64.5225674811446,25.));
#16818=CARTESIAN_POINT('Ctrl Pts',(18.3334665914316,66.0014781595158,25.5785196366098));
#16819=CARTESIAN_POINT('Ctrl Pts',(18.3324169395493,66.1152855036548,25.5709016210591));
#16820=CARTESIAN_POINT('Ctrl Pts',(18.3430836336298,66.2288979300146,25.5632836055085));
#16821=CARTESIAN_POINT('Ctrl Pts',(18.3661914310208,66.3399235223684,25.5556655899578));
#16822=CARTESIAN_POINT('Ctrl Pts',(18.4785584710069,66.8798112911743,25.518621217294));
#16823=CARTESIAN_POINT('Ctrl Pts',(18.8851099357623,67.3585303472824,25.4815768446301));
#16824=CARTESIAN_POINT('Ctrl Pts',(19.3995345876311,67.5569678802536,25.4445324719663));
#16825=CARTESIAN_POINT('Ctrl Pts',(19.9139592394999,67.7554054132248,25.4074880993024));
#16826=CARTESIAN_POINT('Ctrl Pts',(20.536257078482,67.6735614230591,25.3704437266385));
#16827=CARTESIAN_POINT('Ctrl Pts',(20.9821828433076,67.3489732333682,25.3333993539747));
#16828=CARTESIAN_POINT('Ctrl Pts',(21.4281086081331,67.0243850436773,25.2963549813108));
#16829=CARTESIAN_POINT('Ctrl Pts',(21.697662298802,66.4570526544611,25.259310608647));
#16830=CARTESIAN_POINT('Ctrl Pts',(21.6664135722727,65.9064187957527,25.2222662359831));
#16831=CARTESIAN_POINT('Ctrl Pts',(21.6351648457434,65.3557849370443,25.1852218633193));
#16832=CARTESIAN_POINT('Ctrl Pts',(21.3031137020159,64.8218496088437,25.1481774906554));
#16833=CARTESIAN_POINT('Ctrl Pts',(20.8246620716843,64.5495453070113,25.1111331179916));
#16834=CARTESIAN_POINT('Ctrl Pts',(20.3462104413528,64.2772410051789,25.0740887453277));
#16835=CARTESIAN_POINT('Ctrl Pts',(19.7213583244172,64.2665677297147,25.0370443726639));
#16836=CARTESIAN_POINT('Ctrl Pts',(19.2300979593296,64.5225674811445,25.));
#16837=CARTESIAN_POINT('',(18.6629739994073,66.9990030778758,25.));
#16838=CARTESIAN_POINT('Origin',(20.,66.,25.));
#16839=CARTESIAN_POINT('',(18.3354783565503,65.9987788995443,25.0714803633902));
#16840=CARTESIAN_POINT('Ctrl Pts',(18.6629725798064,66.9990042518227,25.));
#16841=CARTESIAN_POINT('Ctrl Pts',(18.4510073780992,66.7145501177189,25.0238267877967));
#16842=CARTESIAN_POINT('Ctrl Pts',(18.3378311247794,66.3559373297411,25.0476535755935));
#16843=CARTESIAN_POINT('Ctrl Pts',(18.3354783565503,65.9987788995443,25.0714803633902));
#16844=CARTESIAN_POINT('',(18.334,66.,24.));
#16845=CARTESIAN_POINT('',(18.334,66.,30.));
#16846=CARTESIAN_POINT('Origin',(20.,66.,24.));
#16847=CARTESIAN_POINT('Ctrl Pts',(18.3354783565503,65.9987788995443,25.0714803633902));
#16848=CARTESIAN_POINT('Ctrl Pts',(18.3342449015815,65.8115361295435,25.0839717212025));
#16849=CARTESIAN_POINT('Ctrl Pts',(18.3634707598459,65.6246930829332,25.0964630790149));
#16850=CARTESIAN_POINT('Ctrl Pts',(18.4248899822037,65.4491448037961,25.1089544368272));
#16851=CARTESIAN_POINT('Ctrl Pts',(18.6070348375451,64.9285387999851,25.1459988094911));
#16852=CARTESIAN_POINT('Ctrl Pts',(19.0723133853053,64.5072678395834,25.1830431821549));
#16853=CARTESIAN_POINT('Ctrl Pts',(19.6082885066022,64.3778809436282,25.2200875548188));
#16854=CARTESIAN_POINT('Ctrl Pts',(20.144263627899,64.2484940476731,25.2571319274826));
#16855=CARTESIAN_POINT('Ctrl Pts',(20.7509353227326,64.4109912161645,25.2941763001465));
#16856=CARTESIAN_POINT('Ctrl Pts',(21.1504371661837,64.7911273133782,25.3312206728103));
#16857=CARTESIAN_POINT('Ctrl Pts',(21.5499390096347,65.1712634105918,25.3682650454742));
#16858=CARTESIAN_POINT('Ctrl Pts',(21.7422710017031,65.7690384365276,25.405309418138));
#16859=CARTESIAN_POINT('Ctrl Pts',(21.6395392863716,66.3108402179399,25.4423537908019));
#16860=CARTESIAN_POINT('Ctrl Pts',(21.5368075710401,66.8526419993522,25.4793981634657));
#16861=CARTESIAN_POINT('Ctrl Pts',(21.1390121483087,67.338470536241,25.5164425361296));
#16862=CARTESIAN_POINT('Ctrl Pts',(20.6281313316149,67.5460304956708,25.5534869087934));
#16863=CARTESIAN_POINT('Ctrl Pts',(20.1172505149211,67.7535904551005,25.5905312814573));
#16864=CARTESIAN_POINT('Ctrl Pts',(19.4932843042648,67.6828818370712,25.6275756541211));
#16865=CARTESIAN_POINT('Ctrl Pts',(19.0418023582524,67.3662475693096,25.664620026785));
#16866=CARTESIAN_POINT('Ctrl Pts',(18.6076787271156,67.0617870714379,25.7002401389867));
#16867=CARTESIAN_POINT('Ctrl Pts',(18.3330311784649,66.5299478078385,25.7358602511885));
#16868=CARTESIAN_POINT('Ctrl Pts',(18.3313535993656,65.999608307577,25.7714803633902));
#16869=CARTESIAN_POINT('Origin',(20.,66.,30.));
#16870=CARTESIAN_POINT('',(18.3344266367885,66.0015125423676,26.4714803633902));
#16871=CARTESIAN_POINT('',(18.336702599684,65.9999597908982,26.2785196366098));
#16872=CARTESIAN_POINT('',(18.334,66.,30.));
#16873=CARTESIAN_POINT('Ctrl Pts',(18.336702599684,65.9999597908982,26.2785196366098));
#16874=CARTESIAN_POINT('Ctrl Pts',(18.3367626127225,66.2804571745203,26.2598345237089));
#16875=CARTESIAN_POINT('Ctrl Pts',(18.403933281346,66.5609816891737,26.241149410808));
#16876=CARTESIAN_POINT('Ctrl Pts',(18.538053161419,66.8046575644459,26.2224642979072));
#16877=CARTESIAN_POINT('Ctrl Pts',(18.8039539801836,67.2877598063567,26.1854199252433));
#16878=CARTESIAN_POINT('Ctrl Pts',(19.3330018469889,67.6260267250789,26.1483755525794));
#16879=CARTESIAN_POINT('Ctrl Pts',(19.8830898233452,67.6646600613318,26.1113311799156));
#16880=CARTESIAN_POINT('Ctrl Pts',(20.4331777997015,67.7032933975846,26.0742868072517));
#16881=CARTESIAN_POINT('Ctrl Pts',(21.004305885609,67.4422931513682,26.0372424345879));
#16882=CARTESIAN_POINT('Ctrl Pts',(21.3351230484566,67.0010994880608,26.000198061924));
#16883=CARTESIAN_POINT('Ctrl Pts',(21.6659402113041,66.5599058247535,25.9631536892602));
#16884=CARTESIAN_POINT('Ctrl Pts',(21.7564464510919,65.9385187443552,25.9261093165963));
#16885=CARTESIAN_POINT('Ctrl Pts',(21.5652075467208,65.4212945794869,25.8890649439325));
#16886=CARTESIAN_POINT('Ctrl Pts',(21.3739686423498,64.9040704146186,25.8520205712686));
#16887=CARTESIAN_POINT('Ctrl Pts',(20.9009845938199,64.4910091652803,25.8149761986048));
#16888=CARTESIAN_POINT('Ctrl Pts',(20.3627356721069,64.3711410197133,25.7779318259409));
#16889=CARTESIAN_POINT('Ctrl Pts',(19.8244867503938,64.2512728741463,25.7408874532771));
#16890=CARTESIAN_POINT('Ctrl Pts',(19.2209729554976,64.4245978323507,25.7038430806132));
#16891=CARTESIAN_POINT('Ctrl Pts',(18.8283073656578,64.8117885522048,25.6667987079493));
#16892=CARTESIAN_POINT('Ctrl Pts',(18.5163917617,65.1193551695888,25.6373723508362));
#16893=CARTESIAN_POINT('Ctrl Pts',(18.3375211159894,65.5618708197218,25.607945993723));
#16894=CARTESIAN_POINT('Ctrl Pts',(18.3334665914316,66.0014781595158,25.5785196366098));
#16895=CARTESIAN_POINT('Ctrl Pts',(18.3313535993656,65.999608307577,25.7714803633902));
#16896=CARTESIAN_POINT('Ctrl Pts',(18.3312865218232,65.9784028274413,25.7729046238523));
#16897=CARTESIAN_POINT('Ctrl Pts',(18.3316558627703,65.9571997450949,25.7743288843144));
#16898=CARTESIAN_POINT('Ctrl Pts',(18.3324688774983,65.9360136919907,25.7757531447766));
#16899=CARTESIAN_POINT('Ctrl Pts',(18.3536150241253,65.3849739999272,25.8127975174404));
#16900=CARTESIAN_POINT('Ctrl Pts',(18.6749049987477,64.8454545332941,25.8498418901043));
#16901=CARTESIAN_POINT('Ctrl Pts',(19.1493178421315,64.5643463136364,25.8868862627681));
#16902=CARTESIAN_POINT('Ctrl Pts',(19.6237306855153,64.2832380939788,25.923930635432));
#16903=CARTESIAN_POINT('Ctrl Pts',(20.2512663976604,64.2605411212966,25.9609750080958));
#16904=CARTESIAN_POINT('Ctrl Pts',(20.7447484473589,64.5066438345424,25.9980193807597));
#16905=CARTESIAN_POINT('Ctrl Pts',(21.2382304970574,64.7527465477881,26.0350637534235));
#16906=CARTESIAN_POINT('Ctrl Pts',(21.5976588843092,65.2676489469618,26.0721081260874));
#16907=CARTESIAN_POINT('Ctrl Pts',(21.658554031172,65.8157206294381,26.1091524987512));
#16908=CARTESIAN_POINT('Ctrl Pts',(21.7194491780347,66.3637923119144,26.1461968714151));
#16909=CARTESIAN_POINT('Ctrl Pts',(21.4818110845084,66.9450332776934,26.1832412440789));
#16910=CARTESIAN_POINT('Ctrl Pts',(21.0543866531954,67.2934566893157,26.2202856167428));
#16911=CARTESIAN_POINT('Ctrl Pts',(20.6269622218823,67.641880100938,26.2573299894066));
#16912=CARTESIAN_POINT('Ctrl Pts',(20.0097514527824,67.7574859584036,26.2943743620705));
#16913=CARTESIAN_POINT('Ctrl Pts',(19.4852026247108,67.587370511937,26.3314187347344));
#16914=CARTESIAN_POINT('Ctrl Pts',(18.9606537966392,67.4172550654703,26.3684631073982));
#16915=CARTESIAN_POINT('Ctrl Pts',(18.5287669095959,66.9614183150713,26.4055074800621));
#16916=CARTESIAN_POINT('Ctrl Pts',(18.3871816596723,66.4284602460038,26.4425518527259));
#16917=CARTESIAN_POINT('Ctrl Pts',(18.3503263056037,66.2897285748037,26.452194689614));
#16918=CARTESIAN_POINT('Ctrl Pts',(18.3331414170134,66.145771262262,26.4618375265021));
#16919=CARTESIAN_POINT('Ctrl Pts',(18.3344266367885,66.0015125423676,26.4714803633902));
#16920=CARTESIAN_POINT('Origin',(20.,66.,30.));
#16921=CARTESIAN_POINT('',(18.3365469699001,65.9994718481762,27.1714803633902));
#16922=CARTESIAN_POINT('',(18.3333666250123,65.9985354189832,26.9785196366098));
#16923=CARTESIAN_POINT('',(18.334,66.,30.));
#16924=CARTESIAN_POINT('Ctrl Pts',(18.3333666250123,65.9985354189832,26.9785196366098));
#16925=CARTESIAN_POINT('Ctrl Pts',(18.3374453090457,66.4429099055735,26.9487674263587));
#16926=CARTESIAN_POINT('Ctrl Pts',(18.5206884737916,66.8902539804794,26.9190152161076));
#16927=CARTESIAN_POINT('Ctrl Pts',(18.8387597051665,67.1984497345904,26.8892630058565));
#16928=CARTESIAN_POINT('Ctrl Pts',(19.2347890801025,67.5821831874113,26.8522186331926));
#16929=CARTESIAN_POINT('Ctrl Pts',(19.8398377253218,67.7501998299206,26.8151742605288));
#16930=CARTESIAN_POINT('Ctrl Pts',(20.3770234062671,67.6256119294545,26.778129887865));
#16931=CARTESIAN_POINT('Ctrl Pts',(20.9142090872123,67.5010240289883,26.7410855152011));
#16932=CARTESIAN_POINT('Ctrl Pts',(21.3835318038834,67.0838315855467,26.7040411425372));
#16933=CARTESIAN_POINT('Ctrl Pts',(21.5702203790488,66.5649500924812,26.6669967698734));
#16934=CARTESIAN_POINT('Ctrl Pts',(21.7569089542143,66.0460685994156,26.6299523972095));
#16935=CARTESIAN_POINT('Ctrl Pts',(21.6609633878742,65.425498056726,26.5929080245457));
#16936=CARTESIAN_POINT('Ctrl Pts',(21.3262899920358,64.9872237156599,26.5558636518818));
#16937=CARTESIAN_POINT('Ctrl Pts',(20.9916165961973,64.5489493745937,26.518819279218));
#16938=CARTESIAN_POINT('Ctrl Pts',(20.4182153708605,64.292971235151,26.4817749065541));
#16939=CARTESIAN_POINT('Ctrl Pts',(19.8684865341392,64.3364300148676,26.4447305338903));
#16940=CARTESIAN_POINT('Ctrl Pts',(19.3187576974179,64.3798887945842,26.4076861612264));
#16941=CARTESIAN_POINT('Ctrl Pts',(18.792701249312,64.7227844934602,26.3706417885625));
#16942=CARTESIAN_POINT('Ctrl Pts',(18.5310499106212,65.2082011254479,26.3335974158987));
#16943=CARTESIAN_POINT('Ctrl Pts',(18.4013750221315,65.4487745080989,26.3152381561357));
#16944=CARTESIAN_POINT('Ctrl Pts',(18.336643633224,65.7243540530003,26.2968788963728));
#16945=CARTESIAN_POINT('Ctrl Pts',(18.336702599684,65.9999597908982,26.2785196366098));
#16946=CARTESIAN_POINT('Ctrl Pts',(18.3344266367885,66.0015125423676,26.4714803633902));
#16947=CARTESIAN_POINT('Ctrl Pts',(18.3380787773415,65.5915802247284,26.498881899166));
#16948=CARTESIAN_POINT('Ctrl Pts',(18.4908762313393,65.1792140559604,26.5262834349417));
#16949=CARTESIAN_POINT('Ctrl Pts',(18.7652753975701,64.8774063579416,26.5536849707175));
#16950=CARTESIAN_POINT('Ctrl Pts',(19.1362379981954,64.4693899266831,26.5907293433813));
#16951=CARTESIAN_POINT('Ctrl Pts',(19.72944681225,64.263436451902,26.6277737160452));
#16952=CARTESIAN_POINT('Ctrl Pts',(20.2734377511034,64.3537943263354,26.664818088709));
#16953=CARTESIAN_POINT('Ctrl Pts',(20.8174286899568,64.4441522007688,26.7018624613729));
#16954=CARTESIAN_POINT('Ctrl Pts',(21.3122017536091,64.8308214244166,26.7389068340368));
#16955=CARTESIAN_POINT('Ctrl Pts',(21.5313390817275,65.336854536141,26.7759512067006));
#16956=CARTESIAN_POINT('Ctrl Pts',(21.7504764098458,65.8428876478653,26.8129955793644));
#16957=CARTESIAN_POINT('Ctrl Pts',(21.6939780024301,66.4682846476661,26.8500399520283));
#16958=CARTESIAN_POINT('Ctrl Pts',(21.387698627229,66.9268515681741,26.8870843246921));
#16959=CARTESIAN_POINT('Ctrl Pts',(21.0814192520278,67.3854184886821,26.924128697356));
#16960=CARTESIAN_POINT('Ctrl Pts',(20.5253589090411,67.6771553298973,26.9611730700199));
#16961=CARTESIAN_POINT('Ctrl Pts',(19.973981762085,67.668557568227,26.9982174426837));
#16962=CARTESIAN_POINT('Ctrl Pts',(19.4226046151289,67.6599598065567,27.0352618153476));
#16963=CARTESIAN_POINT('Ctrl Pts',(18.8759106642033,67.3510274420009,27.0723061880114));
#16964=CARTESIAN_POINT('Ctrl Pts',(18.5840778162202,66.8831340061794,27.1093505606753));
#16965=CARTESIAN_POINT('Ctrl Pts',(18.4209264748504,66.6215546733526,27.1300604949136));
#16966=CARTESIAN_POINT('Ctrl Pts',(18.3374307693608,66.310292807312,27.1507704291519));
#16967=CARTESIAN_POINT('Ctrl Pts',(18.3365469699001,65.9994718481762,27.1714803633902));
#16968=CARTESIAN_POINT('Origin',(20.,66.,30.));
#16969=CARTESIAN_POINT('',(18.3324919306138,65.9987669699924,27.8714803633902));
#16970=CARTESIAN_POINT('',(18.3319383951835,66.0009590761175,27.6785196366098));
#16971=CARTESIAN_POINT('',(18.334,66.,30.));
#16972=CARTESIAN_POINT('Ctrl Pts',(18.3319383951835,66.0009590761175,27.6785196366098));
#16973=CARTESIAN_POINT('Ctrl Pts',(18.3315522952949,66.0572154624142,27.6747447016723));
#16974=CARTESIAN_POINT('Ctrl Pts',(18.3341516128123,66.1134357482357,27.6709697667349));
#16975=CARTESIAN_POINT('Ctrl Pts',(18.3398539528156,66.1693395171271,27.6671948317974));
#16976=CARTESIAN_POINT('Ctrl Pts',(18.3958124293553,66.7179370644852,27.6301504591336));
#16977=CARTESIAN_POINT('Ctrl Pts',(18.7505914623534,67.2360540833893,27.5931060864697));
#16978=CARTESIAN_POINT('Ctrl Pts',(19.2418371848642,67.4865900296292,27.5560617138059));
#16979=CARTESIAN_POINT('Ctrl Pts',(19.733082907375,67.7371259758691,27.519017341142));
#16980=CARTESIAN_POINT('Ctrl Pts',(20.3607953193985,67.7200808494449,27.4819729684782));
#16981=CARTESIAN_POINT('Ctrl Pts',(20.8377208668613,67.4432548354856,27.4449285958143));
#16982=CARTESIAN_POINT('Ctrl Pts',(21.3146464143242,67.1664288215262,27.4078842231505));
#16983=CARTESIAN_POINT('Ctrl Pts',(21.6407850972264,66.6298219200317,27.3708398504866));
#16984=CARTESIAN_POINT('Ctrl Pts',(21.6668894380612,66.0789960097809,27.3337954778227));
#16985=CARTESIAN_POINT('Ctrl Pts',(21.692993778896,65.52817009953,27.2967511051589));
#16986=CARTESIAN_POINT('Ctrl Pts',(21.4190637776633,64.9631251805227,27.259706732495));
#16987=CARTESIAN_POINT('Ctrl Pts',(20.970455189559,64.6424369270067,27.2226623598312));
#16988=CARTESIAN_POINT('Ctrl Pts',(20.5218466014546,64.3217486734907,27.1856179871673));
#16989=CARTESIAN_POINT('Ctrl Pts',(19.8985594264786,64.2454170854659,27.1485736145035));
#16990=CARTESIAN_POINT('Ctrl Pts',(19.3858221505611,64.4483730011308,27.1115292418396));
#16991=CARTESIAN_POINT('Ctrl Pts',(18.8730848746436,64.6513289167956,27.0744848691758));
#16992=CARTESIAN_POINT('Ctrl Pts',(18.4708974977846,65.1335723361501,27.0374404965119));
#16993=CARTESIAN_POINT('Ctrl Pts',(18.3633088616814,65.6744191773935,27.0003961238481));
#16994=CARTESIAN_POINT('Ctrl Pts',(18.3421301035647,65.7808845518395,26.9931039614353));
#16995=CARTESIAN_POINT('Ctrl Pts',(18.3323669538567,65.8896207904243,26.9858117990225));
#16996=CARTESIAN_POINT('Ctrl Pts',(18.3333666250123,65.9985354189832,26.9785196366098));
#16997=CARTESIAN_POINT('Ctrl Pts',(18.3365469699001,65.9994718481762,27.1714803633902));
#16998=CARTESIAN_POINT('Ctrl Pts',(18.3358498953606,65.7543196540673,27.1878148018157));
#16999=CARTESIAN_POINT('Ctrl Pts',(18.3865445959424,65.5094417423179,27.2041492402413));
#17000=CARTESIAN_POINT('Ctrl Pts',(18.4900815811632,65.2894314428002,27.2204836786668));
#17001=CARTESIAN_POINT('Ctrl Pts',(18.7248899391301,64.7904768223294,27.2575280513307));
#17002=CARTESIAN_POINT('Ctrl Pts',(19.2314784001046,64.419422088475,27.2945724239945));
#17003=CARTESIAN_POINT('Ctrl Pts',(19.7780221138092,64.3460691902049,27.3316167966584));
#17004=CARTESIAN_POINT('Ctrl Pts',(20.3245658275138,64.2727162919348,27.3686611693222));
#17005=CARTESIAN_POINT('Ctrl Pts',(20.9110647939486,64.497065229249,27.4057055419861));
#17006=CARTESIAN_POINT('Ctrl Pts',(21.2691255443732,64.9164495130527,27.4427499146499));
#17007=CARTESIAN_POINT('Ctrl Pts',(21.6271862947977,65.3358337968564,27.4797942873138));
#17008=CARTESIAN_POINT('Ctrl Pts',(21.756808829212,65.9502534271496,27.5168386599777));
#17009=CARTESIAN_POINT('Ctrl Pts',(21.598675324677,66.4785378895678,27.5538830326415));
#17010=CARTESIAN_POINT('Ctrl Pts',(21.4405418201421,67.006822351986,27.5909274053054));
#17011=CARTESIAN_POINT('Ctrl Pts',(20.9946522766579,67.4489716465293,27.6279717779692));
#17012=CARTESIAN_POINT('Ctrl Pts',(20.4650545244661,67.602649554542,27.6650161506331));
#17013=CARTESIAN_POINT('Ctrl Pts',(19.9354567722743,67.7563274625547,27.7020605232969));
#17014=CARTESIAN_POINT('Ctrl Pts',(19.3221508113749,67.6215339840369,27.7391048959608));
#17015=CARTESIAN_POINT('Ctrl Pts',(18.9057975191576,67.2599532674978,27.7761492686246));
#17016=CARTESIAN_POINT('Ctrl Pts',(18.5486455209627,66.949785729893,27.8079263002132));
#17017=CARTESIAN_POINT('Ctrl Pts',(18.3364187640716,66.4727395436526,27.8397033318017));
#17018=CARTESIAN_POINT('Ctrl Pts',(18.3324919306138,65.9987669699924,27.8714803633902));
#17019=CARTESIAN_POINT('Origin',(20.,66.,30.));
#17020=CARTESIAN_POINT('',(18.3327118712203,66.00131037449,28.5714803633902));
#17021=CARTESIAN_POINT('',(18.3362664966243,66.0008554996272,28.3785196366098));
#17022=CARTESIAN_POINT('',(18.334,66.,30.));
#17023=CARTESIAN_POINT('Ctrl Pts',(18.3362664966243,66.0008554996272,28.3785196366098));
#17024=CARTESIAN_POINT('Ctrl Pts',(18.335230442349,66.2235152604115,28.3636776043221));
#17025=CARTESIAN_POINT('Ctrl Pts',(18.3767829793478,66.4458041872034,28.3488355720344));
#17026=CARTESIAN_POINT('Ctrl Pts',(18.4627526155864,66.6493313864273,28.3339935397468));
#17027=CARTESIAN_POINT('Ctrl Pts',(18.6773250663718,67.157316901426,28.2969491670829));
#17028=CARTESIAN_POINT('Ctrl Pts',(19.1685967388456,67.5484250087499,28.2599047944191));
#17029=CARTESIAN_POINT('Ctrl Pts',(19.7117520475599,67.6436769415562,28.2228604217552));
#17030=CARTESIAN_POINT('Ctrl Pts',(20.2549073562742,67.7389288743626,28.1858160490914));
#17031=CARTESIAN_POINT('Ctrl Pts',(20.8499463012292,67.5383246326514,28.1487716764275));
#17032=CARTESIAN_POINT('Ctrl Pts',(21.2245673509439,67.1336646652802,28.1117273037636));
#17033=CARTESIAN_POINT('Ctrl Pts',(21.5991884006587,66.7290046979089,28.0746829310998));
#17034=CARTESIAN_POINT('Ctrl Pts',(21.7533915551334,66.1202890048776,28.037638558436));
#17035=CARTESIAN_POINT('Ctrl Pts',(21.6166104162258,65.5860778667307,28.0005941857721));
#17036=CARTESIAN_POINT('Ctrl Pts',(21.4798292773182,65.0518667285838,27.9635498131083));
#17037=CARTESIAN_POINT('Ctrl Pts',(21.0520638450283,64.5921601453213,27.9265054404444));
#17038=CARTESIAN_POINT('Ctrl Pts',(20.5290679994459,64.417328896371,27.8894610677805));
#17039=CARTESIAN_POINT('Ctrl Pts',(20.0060721538635,64.2424976474206,27.8524166951167));
#17040=CARTESIAN_POINT('Ctrl Pts',(19.3878458949885,64.3525417327825,27.8153723224528));
#17041=CARTESIAN_POINT('Ctrl Pts',(18.9573017255916,64.6971028133696,27.778327949789));
#17042=CARTESIAN_POINT('Ctrl Pts',(18.5706313246055,65.0065520654206,27.7450585120626));
#17043=CARTESIAN_POINT('Ctrl Pts',(18.3353411892483,65.5051575930141,27.7117890743362));
#17044=CARTESIAN_POINT('Ctrl Pts',(18.3319383951835,66.0009590761175,27.6785196366098));
#17045=CARTESIAN_POINT('Ctrl Pts',(18.3324919306138,65.9987669699924,27.8714803633902));
#17046=CARTESIAN_POINT('Ctrl Pts',(18.3318410211319,65.9202015697327,27.8767477044655));
#17047=CARTESIAN_POINT('Ctrl Pts',(18.3369133962315,65.8417206205816,27.8820150455409));
#17048=CARTESIAN_POINT('Ctrl Pts',(18.3479976916752,65.7640981587772,27.8872823866162));
#17049=CARTESIAN_POINT('Ctrl Pts',(18.425951779945,65.218191721156,27.92432675928));
#17050=CARTESIAN_POINT('Ctrl Pts',(18.8012605800197,64.714746800474,27.9613711319439));
#17051=CARTESIAN_POINT('Ctrl Pts',(19.3021753989644,64.4841497001422,27.9984155046077));
#17052=CARTESIAN_POINT('Ctrl Pts',(19.803090217909,64.2535525998103,28.0354598772716));
#17053=CARTESIAN_POINT('Ctrl Pts',(20.4296110557237,64.2958033198288,28.0725042499354));
#17054=CARTESIAN_POINT('Ctrl Pts',(20.8950296472222,64.5915670992272,28.1095486225993));
#17055=CARTESIAN_POINT('Ctrl Pts',(21.3604482387207,64.8873308786256,28.1465929952632));
#17056=CARTESIAN_POINT('Ctrl Pts',(21.664764583903,65.436607717404,28.183637367927));
#17057=CARTESIAN_POINT('Ctrl Pts',(21.6687175343226,65.9880377244764,28.2206817405909));
#17058=CARTESIAN_POINT('Ctrl Pts',(21.6726704847421,66.5394677315488,28.2577261132547));
#17059=CARTESIAN_POINT('Ctrl Pts',(21.3762600403988,67.0930509069152,28.2947704859186));
#17060=CARTESIAN_POINT('Ctrl Pts',(20.9151294539268,67.3954566951163,28.3318148585824));
#17061=CARTESIAN_POINT('Ctrl Pts',(20.4539988674548,67.6978624833174,28.3688592312463));
#17062=CARTESIAN_POINT('Ctrl Pts',(19.8281481388542,67.7490908843532,28.4059036039102));
#17063=CARTESIAN_POINT('Ctrl Pts',(19.3239788781539,67.525698773745,28.442947976574));
#17064=CARTESIAN_POINT('Ctrl Pts',(18.8198096174536,67.3023066631369,28.4799923492379));
#17065=CARTESIAN_POINT('Ctrl Pts',(18.4373218246536,66.8042940408847,28.5170367219017));
#17066=CARTESIAN_POINT('Ctrl Pts',(18.3515494410261,66.2595612837239,28.5540810945655));
#17067=CARTESIAN_POINT('Ctrl Pts',(18.3381207099022,66.1742766102555,28.5598808508404));
#17068=CARTESIAN_POINT('Ctrl Pts',(18.3319650040854,66.0878467427289,28.5656806071153));
#17069=CARTESIAN_POINT('Ctrl Pts',(18.3327118712203,66.00131037449,28.5714803633902));
#17070=CARTESIAN_POINT('Origin',(20.,66.,30.));
#17071=CARTESIAN_POINT('',(18.3366137112403,66.0004031163585,29.2714803633902));
#17072=CARTESIAN_POINT('',(18.3350591421361,65.9985780813516,29.0785196366098));
#17073=CARTESIAN_POINT('',(18.334,66.,30.));
#17074=CARTESIAN_POINT('Ctrl Pts',(18.3350591421361,65.9985780813516,29.0785196366098));
#17075=CARTESIAN_POINT('Ctrl Pts',(18.3382113409887,66.3865573365257,29.0526105069719));
#17076=CARTESIAN_POINT('Ctrl Pts',(18.4733909534641,66.7765166182576,29.026701377334));
#17077=CARTESIAN_POINT('Ctrl Pts',(18.7211704627318,67.0720801205599,29.0007922476961));
#17078=CARTESIAN_POINT('Ctrl Pts',(19.0754408148456,67.4946711021229,28.9637478750323));
#17079=CARTESIAN_POINT('Ctrl Pts',(19.6598960683787,67.7242913634506,28.9267035023684));
#17080=CARTESIAN_POINT('Ctrl Pts',(20.2070779973473,67.6558621540768,28.8896591297046));
#17081=CARTESIAN_POINT('Ctrl Pts',(20.7542599263159,67.587432944703,28.8526147570407));
#17082=CARTESIAN_POINT('Ctrl Pts',(21.2641685307198,67.2209542646277,28.8155703843768));
#17083=CARTESIAN_POINT('Ctrl Pts',(21.5034595982802,66.7241339700834,28.778526011713));
#17084=CARTESIAN_POINT('Ctrl Pts',(21.7427506658405,66.2273136755392,28.7414816390491));
#17085=CARTESIAN_POINT('Ctrl Pts',(21.7114241965572,65.600151766526,28.7044372663853));
#17086=CARTESIAN_POINT('Ctrl Pts',(21.4238157992737,65.1296498750344,28.6673928937215));
#17087=CARTESIAN_POINT('Ctrl Pts',(21.1362074019901,64.6591479835428,28.6303485210576));
#17088=CARTESIAN_POINT('Ctrl Pts',(20.5923170767064,64.3453061095728,28.5933041483937));
#17089=CARTESIAN_POINT('Ctrl Pts',(20.0410397399286,64.3317444710009,28.5562597757299));
#17090=CARTESIAN_POINT('Ctrl Pts',(19.4897624031508,64.318182832429,28.519215403066));
#17091=CARTESIAN_POINT('Ctrl Pts',(18.9310980548789,64.6049014292553,28.4821710304022));
#17092=CARTESIAN_POINT('Ctrl Pts',(18.6207024952914,65.0606921890052,28.4451266577383));
#17093=CARTESIAN_POINT('Ctrl Pts',(18.4346686291561,65.3338678661887,28.4229243173622));
#17094=CARTESIAN_POINT('Ctrl Pts',(18.337816340286,65.6677765990296,28.400721976986));
#17095=CARTESIAN_POINT('Ctrl Pts',(18.3362664966243,66.0008554996272,28.3785196366098));
#17096=CARTESIAN_POINT('Ctrl Pts',(18.3327118712203,66.00131037449,28.5714803633902));
#17097=CARTESIAN_POINT('Ctrl Pts',(18.3367354156621,65.5351191241736,28.6027249797792));
#17098=CARTESIAN_POINT('Ctrl Pts',(18.5410870786598,65.0658369847815,28.6339695961681));
#17099=CARTESIAN_POINT('Ctrl Pts',(18.8878468378532,64.7558630906061,28.6652142125571));
#17100=CARTESIAN_POINT('Ctrl Pts',(19.2989735927628,64.3883505467185,28.702258585221));
#17101=CARTESIAN_POINT('Ctrl Pts',(19.9102840770369,64.2447783510127,28.7393029578848));
#17102=CARTESIAN_POINT('Ctrl Pts',(20.4420305825988,64.3908479657171,28.7763473305487));
#17103=CARTESIAN_POINT('Ctrl Pts',(20.9737770881607,64.5369175804214,28.8133917032125));
#17104=CARTESIAN_POINT('Ctrl Pts',(21.4259596150103,64.9726290055359,28.8504360758764));
#17105=CARTESIAN_POINT('Ctrl Pts',(21.5916505399959,65.4985921182107,28.8874804485402));
#17106=CARTESIAN_POINT('Ctrl Pts',(21.7573414649814,66.0245552308856,28.9245248212041));
#17107=CARTESIAN_POINT('Ctrl Pts',(21.6365407881028,66.6407700311209,28.9615691938679));
#17108=CARTESIAN_POINT('Ctrl Pts',(21.2845292764339,67.0652444993399,28.9986135665318));
#17109=CARTESIAN_POINT('Ctrl Pts',(20.932517764765,67.4897189675588,29.0356579391956));
#17110=CARTESIAN_POINT('Ctrl Pts',(20.3492954183058,67.7224531037614,29.0727023118595));
#17111=CARTESIAN_POINT('Ctrl Pts',(19.8017562604999,67.6569431870581,29.1097466845233));
#17112=CARTESIAN_POINT('Ctrl Pts',(19.2542171026941,67.5914332703549,29.1467910571872));
#17113=CARTESIAN_POINT('Ctrl Pts',(18.7423611335417,67.2276793007459,29.183835429851));
#17114=CARTESIAN_POINT('Ctrl Pts',(18.500423717754,66.7321422533326,29.2208798025149));
#17115=CARTESIAN_POINT('Ctrl Pts',(18.3902660153803,66.5065168683279,29.23774665614));
#17116=CARTESIAN_POINT('Ctrl Pts',(18.3360655678455,66.2535713188655,29.2546135097651));
#17117=CARTESIAN_POINT('Ctrl Pts',(18.3366137112403,66.0004031163585,29.2714803633902));
#17118=CARTESIAN_POINT('Origin',(20.,66.,30.));
#17119=CARTESIAN_POINT('',(18.3341898066152,65.9984774012779,29.9714803633902));
#17120=CARTESIAN_POINT('',(18.331239919894,65.9999810457215,29.7785196366098));
#17121=CARTESIAN_POINT('',(18.334,66.,30.));
#17122=CARTESIAN_POINT('Ctrl Pts',(18.3312400241975,65.9999810464378,29.7785196366098));
#17123=CARTESIAN_POINT('Ctrl Pts',(18.3313325829903,66.5504109935318,29.7415434096217));
#17124=CARTESIAN_POINT('Ctrl Pts',(18.6304405504474,67.1009271285011,29.7045671826336));
#17125=CARTESIAN_POINT('Ctrl Pts',(19.0923261408273,67.400317441034,29.6675909556455));
#17126=CARTESIAN_POINT('Ctrl Pts',(19.5550629674809,67.7002595176819,29.6305465829816));
#17127=CARTESIAN_POINT('Ctrl Pts',(20.1811779549493,67.7481492896818,29.5935022103178));
#17128=CARTESIAN_POINT('Ctrl Pts',(20.6841485631442,67.5220714549051,29.5564578376539));
#17129=CARTESIAN_POINT('Ctrl Pts',(21.1871191713391,67.2959936201285,29.5194134649901));
#17130=CARTESIAN_POINT('Ctrl Pts',(21.5669454002605,66.7959481785752,29.4823690923262));
#17131=CARTESIAN_POINT('Ctrl Pts',(21.6498112926465,66.2507657650985,29.4453247196624));
#17132=CARTESIAN_POINT('Ctrl Pts',(21.7326771850326,65.7055833516217,29.4082803469985));
#17133=CARTESIAN_POINT('Ctrl Pts',(21.5185827408833,65.1152639662215,29.3712359743347));
#17134=CARTESIAN_POINT('Ctrl Pts',(21.105501791179,64.7499493770293,29.3341916016708));
#17135=CARTESIAN_POINT('Ctrl Pts',(20.6924208414747,64.3846347878371,29.2971472290069));
#17136=CARTESIAN_POINT('Ctrl Pts',(20.0803533862155,64.2443249948529,29.2601028563431));
#17137=CARTESIAN_POINT('Ctrl Pts',(19.549393538298,64.3932285206161,29.2230584836792));
#17138=CARTESIAN_POINT('Ctrl Pts',(19.0184336903805,64.5421320463792,29.1860141110154));
#17139=CARTESIAN_POINT('Ctrl Pts',(18.5685814498048,64.9802488908897,29.1489697383516));
#17140=CARTESIAN_POINT('Ctrl Pts',(18.4056980548641,65.5070881640441,29.1119253656877));
#17141=CARTESIAN_POINT('Ctrl Pts',(18.356736605199,65.6654518484674,29.1007901226617));
#17142=CARTESIAN_POINT('Ctrl Pts',(18.3337043880097,65.8318320981489,29.0896548796358));
#17143=CARTESIAN_POINT('Ctrl Pts',(18.3350591421361,65.9985780813516,29.0785196366098));
#17144=CARTESIAN_POINT('Ctrl Pts',(18.3366137112403,66.0004031163585,29.2714803633902));
#17145=CARTESIAN_POINT('Ctrl Pts',(18.3372694455005,65.6975424679157,29.291657882429));
#17146=CARTESIAN_POINT('Ctrl Pts',(18.4162754187729,65.3943631826101,29.3118354014677));
#17147=CARTESIAN_POINT('Ctrl Pts',(18.5715624112669,65.1372559125187,29.3320129205065));
#17148=CARTESIAN_POINT('Ctrl Pts',(18.8566573829902,64.6652267443359,29.3690572931703));
#17149=CARTESIAN_POINT('Ctrl Pts',(19.3988661888596,64.3484885331883,29.4061016658342));
#17150=CARTESIAN_POINT('Ctrl Pts',(19.950063408744,64.3319869178441,29.443146038498));
#17151=CARTESIAN_POINT('Ctrl Pts',(20.5012606286283,64.3154853024999,29.4801904111619));
#17152=CARTESIAN_POINT('Ctrl Pts',(21.0614462625275,64.5992202829592,29.5172347838257));
#17153=CARTESIAN_POINT('Ctrl Pts',(21.3742683400236,65.0533491483137,29.5542791564896));
#17154=CARTESIAN_POINT('Ctrl Pts',(21.6870904175196,65.5074780136683,29.5913235291534));
#17155=CARTESIAN_POINT('Ctrl Pts',(21.7525489386125,66.1320007639182,29.6283679018173));
#17156=CARTESIAN_POINT('Ctrl Pts',(21.5406887958389,66.6411234980611,29.6654122744811));
#17157=CARTESIAN_POINT('Ctrl Pts',(21.3288286530653,67.150246232204,29.702456647145));
#17158=CARTESIAN_POINT('Ctrl Pts',(20.8396498464252,67.5439689502399,29.7395010198089));
#17159=CARTESIAN_POINT('Ctrl Pts',(20.2970102247823,67.6421163880079,29.7765453924727));
#17160=CARTESIAN_POINT('Ctrl Pts',(19.7543706031394,67.740263825776,29.8135897651366));
#17161=CARTESIAN_POINT('Ctrl Pts',(19.1582701664937,67.5428359832763,29.8506341378004));
#17162=CARTESIAN_POINT('Ctrl Pts',(18.7814962057965,67.1401797265787,29.8876785104642));
#17163=CARTESIAN_POINT('Ctrl Pts',(18.4973832733844,66.8365498004747,29.9156124614396));
#17164=CARTESIAN_POINT('Ctrl Pts',(18.3379832198998,66.4162234004879,29.9435464124149));
#17165=CARTESIAN_POINT('Ctrl Pts',(18.3341898066152,65.9984774012779,29.9714803633902));
#17166=CARTESIAN_POINT('Origin',(20.,66.,30.));
#17167=CARTESIAN_POINT('',(18.3314457742944,66.0005306220934,30.6714803633902));
#17168=CARTESIAN_POINT('',(18.3350038845013,66.001433884838,30.4785196366098));
#17169=CARTESIAN_POINT('',(18.334,66.,30.));
#17170=CARTESIAN_POINT('Ctrl Pts',(18.3350038845013,66.001433884838,30.4785196366098));
#17171=CARTESIAN_POINT('Ctrl Pts',(18.3336511769542,66.1661251266506,30.4675206849353));
#17172=CARTESIAN_POINT('Ctrl Pts',(18.3561120206751,66.3304555620997,30.4565217332608));
#17173=CARTESIAN_POINT('Ctrl Pts',(18.4038997873377,66.4870573697509,30.4455227815864));
#17174=CARTESIAN_POINT('Ctrl Pts',(18.5648485658592,67.0144908828857,30.4084784089225));
#17175=CARTESIAN_POINT('Ctrl Pts',(19.0130898719618,67.4542557510803,30.3714340362587));
#17176=CARTESIAN_POINT('Ctrl Pts',(19.54349966267,67.6051069161607,30.3343896635948));
#17177=CARTESIAN_POINT('Ctrl Pts',(20.0739094533782,67.7559580812411,30.297345290931));
#17178=CARTESIAN_POINT('Ctrl Pts',(20.6864877286921,67.6178955432072,30.2603009182671));
#17179=CARTESIAN_POINT('Ctrl Pts',(21.1009066144049,67.2540994365077,30.2232565456033));
#17180=CARTESIAN_POINT('Ctrl Pts',(21.5153255001178,66.8903033298081,30.1862121729394));
#17181=CARTESIAN_POINT('Ctrl Pts',(21.7315849962297,66.3007736544428,30.1491678002756));
#17182=CARTESIAN_POINT('Ctrl Pts',(21.6507205013744,65.7552907916899,30.1121234276117));
#17183=CARTESIAN_POINT('Ctrl Pts',(21.5698560065191,65.2098079289371,30.0750790549479));
#17184=CARTESIAN_POINT('Ctrl Pts',(21.1918675206966,64.7083718787967,30.038034682284));
#17185=CARTESIAN_POINT('Ctrl Pts',(20.6897300137602,64.4804496459782,30.0009903096202));
#17186=CARTESIAN_POINT('Ctrl Pts',(20.1875925068238,64.2525274131597,29.9639459369563));
#17187=CARTESIAN_POINT('Ctrl Pts',(19.5613059787735,64.2981189976632,29.9269015642925));
#17188=CARTESIAN_POINT('Ctrl Pts',(19.0974714700439,64.5963607931863,29.8898571916286));
#17189=CARTESIAN_POINT('Ctrl Pts',(18.6327837057788,64.8951512250401,29.852744673289));
#17190=CARTESIAN_POINT('Ctrl Pts',(18.3311471242406,65.4475222595322,29.8156321549494));
#17191=CARTESIAN_POINT('Ctrl Pts',(18.3312400241975,65.9999810464378,29.7785196366098));
#17192=CARTESIAN_POINT('Ctrl Pts',(18.3341898066152,65.9984774012779,29.9714803633902));
#17193=CARTESIAN_POINT('Ctrl Pts',(18.3329526169784,65.8622330792747,29.9805907850787));
#17194=CARTESIAN_POINT('Ctrl Pts',(18.348267041402,65.72626323012,29.9897012067673));
#17195=CARTESIAN_POINT('Ctrl Pts',(18.3812048191077,65.5947057023479,29.9988116284558));
#17196=CARTESIAN_POINT('Ctrl Pts',(18.5151348778648,65.0597726057102,30.0358560011197));
#17197=CARTESIAN_POINT('Ctrl Pts',(18.9404424801278,64.59779108333,30.0729003737835));
#17198=CARTESIAN_POINT('Ctrl Pts',(19.462498497129,64.4201729715564,30.1099447464474));
#17199=CARTESIAN_POINT('Ctrl Pts',(19.9845545141302,64.2425548597828,30.1469891191112));
#17200=CARTESIAN_POINT('Ctrl Pts',(20.6033589458697,64.3493001586158,30.1840334917751));
#17201=CARTESIAN_POINT('Ctrl Pts',(21.0357347064309,64.6915601185824,30.2210778644389));
#17202=CARTESIAN_POINT('Ctrl Pts',(21.468110466992,65.033820078549,30.2581222371028));
#17203=CARTESIAN_POINT('Ctrl Pts',(21.7140575563749,65.6115946996491,30.2951666097666));
#17204=CARTESIAN_POINT('Ctrl Pts',(21.6610257462864,66.1604829447737,30.3322109824305));
#17205=CARTESIAN_POINT('Ctrl Pts',(21.6079939361978,66.7093711898982,30.3692553550943));
#17206=CARTESIAN_POINT('Ctrl Pts',(21.2559832266379,67.2293730590472,30.4062997277582));
#17207=CARTESIAN_POINT('Ctrl Pts',(20.7660806458043,67.4825254633609,30.4433441004221));
#17208=CARTESIAN_POINT('Ctrl Pts',(20.2761780649708,67.7356778676746,30.4803884730859));
#17209=CARTESIAN_POINT('Ctrl Pts',(19.6483836128637,67.7219808071531,30.5174328457497));
#17210=CARTESIAN_POINT('Ctrl Pts',(19.1699883856417,67.4477023262466,30.5544772184136));
#17211=CARTESIAN_POINT('Ctrl Pts',(18.6915931584198,67.1734238453401,30.5915215910774));
#17212=CARTESIAN_POINT('Ctrl Pts',(18.3625971560829,66.6385639440485,30.6285659637413));
#17213=CARTESIAN_POINT('Ctrl Pts',(18.3335554238786,66.0878850391431,30.6656103364052));
#17214=CARTESIAN_POINT('Ctrl Pts',(18.3320214459357,66.0587982998317,30.6675670120668));
#17215=CARTESIAN_POINT('Ctrl Pts',(18.3313243191979,66.0296674266187,30.6695236877285));
#17216=CARTESIAN_POINT('Ctrl Pts',(18.3314457742944,66.0005306220934,30.6714803633902));
#17217=CARTESIAN_POINT('Origin',(20.,66.,30.));
#17218=CARTESIAN_POINT('',(18.3357539380163,66.0011866318746,31.3714803633902));
#17219=CARTESIAN_POINT('',(18.3362976425678,65.9991726430109,31.1785196366098));
#17220=CARTESIAN_POINT('',(18.334,66.,30.));
#17221=CARTESIAN_POINT('Ctrl Pts',(18.3362976425678,65.9991726430109,31.1785196366098));
#17222=CARTESIAN_POINT('Ctrl Pts',(18.3377856536118,66.3302224149229,31.1564535875851));
#17223=CARTESIAN_POINT('Ctrl Pts',(18.4333702676718,66.662063920961,31.1343875385604));
#17224=CARTESIAN_POINT('Ctrl Pts',(18.6172644901874,66.9342394126736,31.1123214895358));
#17225=CARTESIAN_POINT('Ctrl Pts',(18.9259851905709,67.3911662659444,31.0752771168719));
#17226=CARTESIAN_POINT('Ctrl Pts',(19.4835935086859,67.6799332504904,31.038232744208));
#17227=CARTESIAN_POINT('Ctrl Pts',(20.0349169045382,67.6683949113045,31.0011883715442));
#17228=CARTESIAN_POINT('Ctrl Pts',(20.5862403003904,67.6568565721186,30.9641439988803));
#17229=CARTESIAN_POINT('Ctrl Pts',(21.13127877398,67.3450129092009,30.9270996262165));
#17230=CARTESIAN_POINT('Ctrl Pts',(21.4206119935396,66.8755697197258,30.8900552535526));
#17231=CARTESIAN_POINT('Ctrl Pts',(21.7099452130993,66.4061265302508,30.8530108808888));
#17232=CARTESIAN_POINT('Ctrl Pts',(21.743573178629,65.7790838142184,30.8159665082249));
#17233=CARTESIAN_POINT('Ctrl Pts',(21.5061070713104,65.2813886585656,30.7789221355611));
#17234=CARTESIAN_POINT('Ctrl Pts',(21.2686409639919,64.7836935029129,30.7418777628972));
#17235=CARTESIAN_POINT('Ctrl Pts',(20.7600807838251,64.4153459076396,30.7048333902334));
#17236=CARTESIAN_POINT('Ctrl Pts',(20.2131536776213,64.344908981353,30.6677890175695));
#17237=CARTESIAN_POINT('Ctrl Pts',(19.6662265714174,64.2744720550664,30.6307446449057));
#17238=CARTESIAN_POINT('Ctrl Pts',(19.0809325391764,64.5019457977663,30.5937002722418));
#17239=CARTESIAN_POINT('Ctrl Pts',(18.7251136485261,64.9232337481538,30.556655899578));
#17240=CARTESIAN_POINT('Ctrl Pts',(18.4749419723296,65.2194358764815,30.5306104785886));
#17241=CARTESIAN_POINT('Ctrl Pts',(18.3382070840956,65.6114464702889,30.5045650575992));
#17242=CARTESIAN_POINT('Ctrl Pts',(18.3350038845013,66.001433884838,30.4785196366098));
#17243=CARTESIAN_POINT('Ctrl Pts',(18.3314457742944,66.0005306220934,30.6714803633902));
#17244=CARTESIAN_POINT('Ctrl Pts',(18.3336237436472,65.478040672012,30.7065680603924));
#17245=CARTESIAN_POINT('Ctrl Pts',(18.5990309619734,64.9536434051272,30.7416557573945));
#17246=CARTESIAN_POINT('Ctrl Pts',(19.0223181288011,64.6476319050944,30.7767434543967));
#17247=CARTESIAN_POINT('Ctrl Pts',(19.4692100279994,64.3245555844701,30.8137878270606));
#17248=CARTESIAN_POINT('Ctrl Pts',(20.0920812884675,64.2449008517406,30.8508321997244));
#17249=CARTESIAN_POINT('Ctrl Pts',(20.6058937634283,64.4451192801928,30.8878765723883));
#17250=CARTESIAN_POINT('Ctrl Pts',(21.1197062383891,64.645337708645,30.9249209450521));
#17251=CARTESIAN_POINT('Ctrl Pts',(21.5244599278425,65.1254292982789,30.961965317716));
#17252=CARTESIAN_POINT('Ctrl Pts',(21.6349315780197,65.6656946895675,30.9990096903798));
#17253=CARTESIAN_POINT('Ctrl Pts',(21.745403228197,66.2059600808562,31.0360540630437));
#17254=CARTESIAN_POINT('Ctrl Pts',(21.561592839098,66.8063992737996,31.0730984357076));
#17255=CARTESIAN_POINT('Ctrl Pts',(21.1676156621277,67.1922394771788,31.1101428083714));
#17256=CARTESIAN_POINT('Ctrl Pts',(20.7736384851573,67.578079680558,31.1471871810353));
#17257=CARTESIAN_POINT('Ctrl Pts',(20.1694945203157,67.7493208943729,31.1842315536991));
#17258=CARTESIAN_POINT('Ctrl Pts',(19.6316519353517,67.6275997691876,31.221275926363));
#17259=CARTESIAN_POINT('Ctrl Pts',(19.0938093503877,67.5058786440022,31.2583202990268));
#17260=CARTESIAN_POINT('Ctrl Pts',(18.6222681453012,67.0911951798166,31.2953646716907));
#17261=CARTESIAN_POINT('Ctrl Pts',(18.4328148553804,66.5733166907331,31.3324090443545));
#17262=CARTESIAN_POINT('Ctrl Pts',(18.3662083381997,66.391244991186,31.3454328173664));
#17263=CARTESIAN_POINT('Ctrl Pts',(18.3344687445157,66.1964180729821,31.3584565903783));
#17264=CARTESIAN_POINT('Ctrl Pts',(18.3357539380163,66.0011866318746,31.3714803633902));
#17265=CARTESIAN_POINT('Origin',(20.,66.,30.));
#17266=CARTESIAN_POINT('',(18.3357307739255,65.9988024507997,32.0714803633902));
#17267=CARTESIAN_POINT('',(18.3319842739515,65.9990126572197,31.8785196366098));
#17268=CARTESIAN_POINT('',(18.334,66.,30.));
#17269=CARTESIAN_POINT('Ctrl Pts',(18.3319842739515,65.9990126572197,31.8785196366098));
#17270=CARTESIAN_POINT('Ctrl Pts',(18.3354516324952,66.4928187659276,31.8453864902349));
#17271=CARTESIAN_POINT('Ctrl Pts',(18.5685743286719,66.9894689012208,31.81225334386));
#17272=CARTESIAN_POINT('Ctrl Pts',(18.9525270673117,67.2990616711976,31.7791201974851));
#17273=CARTESIAN_POINT('Ctrl Pts',(19.3818037853917,67.6452005441947,31.7420758248213));
#17274=CARTESIAN_POINT('Ctrl Pts',(19.9996220148489,67.7575128015186,31.7050314521574));
#17275=CARTESIAN_POINT('Ctrl Pts',(20.5232559753395,67.5846021439342,31.6679870794935));
#17276=CARTESIAN_POINT('Ctrl Pts',(21.04688993583,67.4116914863498,31.6309427068297));
#17277=CARTESIAN_POINT('Ctrl Pts',(21.4763396273538,66.9535579138571,31.5938983341658));
#17278=CARTESIAN_POINT('Ctrl Pts',(21.615080419582,66.4198523652096,31.556853961502));
#17279=CARTESIAN_POINT('Ctrl Pts',(21.7538212118103,65.8861468165621,31.5198095888381));
#17280=CARTESIAN_POINT('Ctrl Pts',(21.601853104743,65.2768692917598,31.4827652161743));
#17281=CARTESIAN_POINT('Ctrl Pts',(21.2287196948773,64.8708371766171,31.4457208435104));
#17282=CARTESIAN_POINT('Ctrl Pts',(20.8555862850116,64.4648050614744,31.4086764708466));
#17283=CARTESIAN_POINT('Ctrl Pts',(20.2612875723476,64.2620183559913,31.3716320981827));
#17284=CARTESIAN_POINT('Ctrl Pts',(19.7177863434849,64.3552762474003,31.3345877255189));
#17285=CARTESIAN_POINT('Ctrl Pts',(19.1742851146223,64.4485341388093,31.297543352855));
#17286=CARTESIAN_POINT('Ctrl Pts',(18.681581369561,64.8378366271104,31.2604989801912));
#17287=CARTESIAN_POINT('Ctrl Pts',(18.4651460383564,65.3450312322588,31.2234546075273));
#17288=CARTESIAN_POINT('Ctrl Pts',(18.3776337333931,65.550107587928,31.2084762838881));
#17289=CARTESIAN_POINT('Ctrl Pts',(18.3352875881185,65.7744577147142,31.193497960249));
#17290=CARTESIAN_POINT('Ctrl Pts',(18.3362976425678,65.9991726430109,31.1785196366098));
#17291=CARTESIAN_POINT('Ctrl Pts',(18.3357539380163,66.0011866318746,31.3714803633902));
#17292=CARTESIAN_POINT('Ctrl Pts',(18.3381243047699,65.6411084669653,31.3955009630422));
#17293=CARTESIAN_POINT('Ctrl Pts',(18.4528345838942,65.2796542426953,31.4195215626941));
#17294=CARTESIAN_POINT('Ctrl Pts',(18.6683273035712,64.9943116113947,31.4435421623461));
#17295=CARTESIAN_POINT('Ctrl Pts',(19.000658416438,64.5542585351211,31.4805865350099));
#17296=CARTESIAN_POINT('Ctrl Pts',(19.5726860169266,64.295225896555,31.5176309076738));
#17297=CARTESIAN_POINT('Ctrl Pts',(20.1226390176602,64.3357521288171,31.5546752803376));
#17298=CARTESIAN_POINT('Ctrl Pts',(20.6725920183937,64.3762783610791,31.5917196530015));
#17299=CARTESIAN_POINT('Ctrl Pts',(21.2004704193721,64.7163634641693,31.6287640256654));
#17300=CARTESIAN_POINT('Ctrl Pts',(21.4647066757619,65.200377802104,31.6658083983292));
#17301=CARTESIAN_POINT('Ctrl Pts',(21.7289429321517,65.6843921400386,31.7028527709931));
#17302=CARTESIAN_POINT('Ctrl Pts',(21.7295370439529,66.3123357128176,31.7398971436569));
#17303=CARTESIAN_POINT('Ctrl Pts',(21.4662171339133,66.7968491837283,31.7769415163207));
#17304=CARTESIAN_POINT('Ctrl Pts',(21.2028972238738,67.281362654639,31.8139858889846));
#17305=CARTESIAN_POINT('Ctrl Pts',(20.6756632919933,67.6224460236814,31.8510302616485));
#17306=CARTESIAN_POINT('Ctrl Pts',(20.1257879613633,67.6640128287263,31.8880746343123));
#17307=CARTESIAN_POINT('Ctrl Pts',(19.5759126307332,67.7055796337712,31.9251190069762));
#17308=CARTESIAN_POINT('Ctrl Pts',(19.0033959013535,67.4476298748186,31.96216337964));
#17309=CARTESIAN_POINT('Ctrl Pts',(18.6702326956076,67.0082064379672,31.9992077523039));
#17310=CARTESIAN_POINT('Ctrl Pts',(18.4535684353736,66.7224385253258,32.023298622666));
#17311=CARTESIAN_POINT('Ctrl Pts',(18.3381320961367,66.3599213639141,32.0473894930281));
#17312=CARTESIAN_POINT('Ctrl Pts',(18.3357307739255,65.9988024507997,32.0714803633902));
#17313=CARTESIAN_POINT('Origin',(20.,66.,30.));
#17314=CARTESIAN_POINT('',(18.3314318999871,65.9994875421513,32.7714803633902));
#17315=CARTESIAN_POINT('',(18.3333052932669,66.0014544402739,32.5785196366098));
#17316=CARTESIAN_POINT('',(18.334,66.,30.));
#17317=CARTESIAN_POINT('Ctrl Pts',(18.3333052932669,66.0014544402739,32.5785196366098));
#17318=CARTESIAN_POINT('Ctrl Pts',(18.3323271062934,66.1083233110254,32.5713637655485));
#17319=CARTESIAN_POINT('Ctrl Pts',(18.3417256310295,66.2150208191139,32.5642078944873));
#17320=CARTESIAN_POINT('Ctrl Pts',(18.3621249858483,66.319571914139,32.557052023426));
#17321=CARTESIAN_POINT('Ctrl Pts',(18.4677279649323,66.8608099679505,32.5200076507622));
#17322=CARTESIAN_POINT('Ctrl Pts',(18.8681427916334,67.3445261805719,32.4829632780983));
#17323=CARTESIAN_POINT('Ctrl Pts',(19.3801317611667,67.5493624936648,32.4459189054345));
#17324=CARTESIAN_POINT('Ctrl Pts',(19.8921207307,67.7541988067578,32.4088745327706));
#17325=CARTESIAN_POINT('Ctrl Pts',(20.5156838430653,67.6801552203222,32.3718301601068));
#17326=CARTESIAN_POINT('Ctrl Pts',(20.9654663464417,67.3611155366749,32.3347857874429));
#17327=CARTESIAN_POINT('Ctrl Pts',(21.4152488498181,67.0420758530276,32.297741414779));
#17328=CARTESIAN_POINT('Ctrl Pts',(21.6912507442055,66.4780400721686,32.2606970421152));
#17329=CARTESIAN_POINT('Ctrl Pts',(21.667168131068,65.9271220675347,32.2236526694513));
#17330=CARTESIAN_POINT('Ctrl Pts',(21.6430855179306,65.3762040629009,32.1866082967875));
#17331=CARTESIAN_POINT('Ctrl Pts',(21.3189183972682,64.8384038344924,32.1495639241236));
#17332=CARTESIAN_POINT('Ctrl Pts',(20.8430120230428,64.5598293506342,32.1125195514598));
#17333=CARTESIAN_POINT('Ctrl Pts',(20.3671056488173,64.281254866776,32.0754751787959));
#17334=CARTESIAN_POINT('Ctrl Pts',(19.7394600210288,64.2619061274682,32.0384308061321));
#17335=CARTESIAN_POINT('Ctrl Pts',(19.2472981308988,64.5106374965976,32.0013864334682));
#17336=CARTESIAN_POINT('Ctrl Pts',(18.7551362407689,64.7593688657269,31.9643420608044));
#17337=CARTESIAN_POINT('Ctrl Pts',(18.3984580882975,65.2761803432934,31.9272976881405));
#17338=CARTESIAN_POINT('Ctrl Pts',(18.3404866154132,65.8245688264118,31.8902533154767));
#17339=CARTESIAN_POINT('Ctrl Pts',(18.3343658598854,65.8824688878111,31.8863420891877));
#17340=CARTESIAN_POINT('Ctrl Pts',(18.3315749670979,65.9407209570542,31.8824308628987));
#17341=CARTESIAN_POINT('Ctrl Pts',(18.3319842739515,65.9990126572197,31.8785196366098));
#17342=CARTESIAN_POINT('Ctrl Pts',(18.3357307739255,65.9988024507997,32.0714803633902));
#17343=CARTESIAN_POINT('Ctrl Pts',(18.3344395987906,65.8046311899893,32.0844338656919));
#17344=CARTESIAN_POINT('Ctrl Pts',(18.3658284528694,65.6108641826254,32.0973873679937));
#17345=CARTESIAN_POINT('Ctrl Pts',(18.431732805963,65.4296498325619,32.1103408702954));
#17346=CARTESIAN_POINT('Ctrl Pts',(18.620205804176,64.9114137787584,32.1473852429593));
#17347=CARTESIAN_POINT('Ctrl Pts',(19.0909614827139,64.4958387859018,32.1844296156231));
#17348=CARTESIAN_POINT('Ctrl Pts',(19.6285727786963,64.3731001491597,32.221473988287));
#17349=CARTESIAN_POINT('Ctrl Pts',(20.1661840746786,64.2503615124175,32.2585183609508));
#17350=CARTESIAN_POINT('Ctrl Pts',(20.7706509881054,64.4204592317899,32.2955627336147));
#17351=CARTESIAN_POINT('Ctrl Pts',(21.1653575635997,64.8055532434009,32.3326071062786));
#17352=CARTESIAN_POINT('Ctrl Pts',(21.5600641390939,65.190647255012,32.3696514789424));
#17353=CARTESIAN_POINT('Ctrl Pts',(21.7450103766556,65.7907375588616,32.4066958516063));
#17354=CARTESIAN_POINT('Ctrl Pts',(21.63556123827,66.3312110222473,32.4437402242701));
#17355=CARTESIAN_POINT('Ctrl Pts',(21.5261120998843,66.871684485633,32.480784596934));
#17356=CARTESIAN_POINT('Ctrl Pts',(21.1222675855513,67.3525411085547,32.5178289695978));
#17357=CARTESIAN_POINT('Ctrl Pts',(20.6088348926125,67.5537314371952,32.5548733422617));
#17358=CARTESIAN_POINT('Ctrl Pts',(20.0954021996737,67.7549217658357,32.5919177149255));
#17359=CARTESIAN_POINT('Ctrl Pts',(19.472381328129,67.676445800195,32.6289620875894));
#17360=CARTESIAN_POINT('Ctrl Pts',(19.0248788897283,67.3542156865465,32.6660064602532));
#17361=CARTESIAN_POINT('Ctrl Pts',(18.6001645498948,67.0483944479364,32.7011644279655));
#17362=CARTESIAN_POINT('Ctrl Pts',(18.3335479895291,66.5230122843236,32.7363223956779));
#17363=CARTESIAN_POINT('Ctrl Pts',(18.3314318999871,65.9994875421513,32.7714803633902));
#17364=CARTESIAN_POINT('Origin',(20.,66.,30.));
#17365=CARTESIAN_POINT('',(18.3342212861325,66.001521965989,33.4714803633902));
#17366=CARTESIAN_POINT('',(18.3367009922703,66.0000736897305,33.2785196366098));
#17367=CARTESIAN_POINT('',(18.334,66.,30.));
#17368=CARTESIAN_POINT('Ctrl Pts',(18.3367009922703,66.0000736897305,33.2785196366098));
#17369=CARTESIAN_POINT('Ctrl Pts',(18.3365930524491,66.2736326347662,33.2602966681983));
#17370=CARTESIAN_POINT('Ctrl Pts',(18.4003187084924,66.5471442261593,33.2420736997869));
#17371=CARTESIAN_POINT('Ctrl Pts',(18.5281535749071,66.7864024867719,33.2238507313754));
#17372=CARTESIAN_POINT('Ctrl Pts',(18.7880213595606,67.2727761646991,33.1868063587115));
#17373=CARTESIAN_POINT('Ctrl Pts',(19.3128164190146,67.6176001101629,33.1497619860477));
#17374=CARTESIAN_POINT('Ctrl Pts',(19.8623822062184,67.6630760996231,33.1127176133838));
#17375=CARTESIAN_POINT('Ctrl Pts',(20.4119479934222,67.7085520890833,33.07567324072));
#17376=CARTESIAN_POINT('Ctrl Pts',(20.9862845083758,67.4546801225399,33.0386288680561));
#17377=CARTESIAN_POINT('Ctrl Pts',(21.3225640589931,67.0176370080482,33.0015844953923));
#17378=CARTESIAN_POINT('Ctrl Pts',(21.6588436096103,66.5805938935566,32.9645401227284));
#17379=CARTESIAN_POINT('Ctrl Pts',(21.7570661958914,65.9603796311168,32.9274957500646));
#17380=CARTESIAN_POINT('Ctrl Pts',(21.5722832293577,65.4408164729121,32.8904513774007));
#17381=CARTESIAN_POINT('Ctrl Pts',(21.387500262824,64.9212533147075,32.8534070047369));
#17382=CARTESIAN_POINT('Ctrl Pts',(20.9197117434757,64.5023412607381,32.816362632073));
#17383=CARTESIAN_POINT('Ctrl Pts',(20.382986903752,64.3757827110126,32.7793182594091));
#17384=CARTESIAN_POINT('Ctrl Pts',(19.8462620640284,64.2492241612871,32.7422738867453));
#17385=CARTESIAN_POINT('Ctrl Pts',(19.2406009039295,64.4150191158055,32.7052295140814));
#17386=CARTESIAN_POINT('Ctrl Pts',(18.8431658896135,64.7972965405656,32.6681851414176));
#17387=CARTESIAN_POINT('Ctrl Pts',(18.5225034999409,65.1057293361823,32.638296639815));
#17388=CARTESIAN_POINT('Ctrl Pts',(18.337390965392,65.555086641388,32.6084081382124));
#17389=CARTESIAN_POINT('Ctrl Pts',(18.3333052932669,66.0014544402739,32.5785196366098));
#17390=CARTESIAN_POINT('Ctrl Pts',(18.3314318999871,65.9994875421513,32.7714803633902));
#17391=CARTESIAN_POINT('Ctrl Pts',(18.3313183609503,65.9713977596598,32.7733667683417));
#17392=CARTESIAN_POINT('Ctrl Pts',(18.3319662848669,65.9433133244466,32.7752531732933));
#17393=CARTESIAN_POINT('Ctrl Pts',(18.3333921073574,65.9152684381647,32.7771395782448));
#17394=CARTESIAN_POINT('Ctrl Pts',(18.3613917686438,65.3645355650877,32.8141839509086));
#17395=CARTESIAN_POINT('Ctrl Pts',(18.6893750964734,64.82905408059,32.8512283235725));
#17396=CARTESIAN_POINT('Ctrl Pts',(19.167250465381,64.5538708501677,32.8882726962364));
#17397=CARTESIAN_POINT('Ctrl Pts',(19.6451258342887,64.2786876197455,32.9253170689002));
#17398=CARTESIAN_POINT('Ctrl Pts',(20.2728932442745,64.2638026433987,32.9623614415641));
#17399=CARTESIAN_POINT('Ctrl Pts',(20.763273974189,64.5160275792031,32.9994058142279));
#17400=CARTESIAN_POINT('Ctrl Pts',(21.2536547041036,64.7682525150074,33.0364501868918));
#17401=CARTESIAN_POINT('Ctrl Pts',(21.6066487539469,65.2875873629629,33.0734945595556));
#17402=CARTESIAN_POINT('Ctrl Pts',(21.6607190996507,65.8363742763029,33.1105389322195));
#17403=CARTESIAN_POINT('Ctrl Pts',(21.7147894453546,66.3851611896429,33.1475833048833));
#17404=CARTESIAN_POINT('Ctrl Pts',(21.4699360869189,66.9634001683674,33.1846276775472));
#17405=CARTESIAN_POINT('Ctrl Pts',(21.0382087398405,67.3064776760442,33.221672050211));
#17406=CARTESIAN_POINT('Ctrl Pts',(20.6064813927622,67.649555183721,33.2587164228749));
#17407=CARTESIAN_POINT('Ctrl Pts',(19.9878800570411,67.75747122035,33.2957607955387));
#17408=CARTESIAN_POINT('Ctrl Pts',(19.46548887784,67.5808412840736,33.3328051682026));
#17409=CARTESIAN_POINT('Ctrl Pts',(18.9430976986389,67.4042113477973,33.3698495408664));
#17410=CARTESIAN_POINT('Ctrl Pts',(18.5169166759577,66.9430354386155,33.4068939135303));
#17411=CARTESIAN_POINT('Ctrl Pts',(18.3819746329741,66.4083567278835,33.4439382861942));
#17412=CARTESIAN_POINT('Ctrl Pts',(18.3485319992028,66.2758475119791,33.4531189785928));
#17413=CARTESIAN_POINT('Ctrl Pts',(18.3329771223643,66.1388237896396,33.4622996709915));
#17414=CARTESIAN_POINT('Ctrl Pts',(18.3342212861325,66.001521965989,33.4714803633902));
#17415=CARTESIAN_POINT('Origin',(20.,66.,30.));
#17416=CARTESIAN_POINT('',(18.3366059400397,65.999580177369,34.1714803633902));
#17417=CARTESIAN_POINT('',(18.3335757493505,65.9985070366392,33.9785196366098));
#17418=CARTESIAN_POINT('',(18.334,66.,30.));
#17419=CARTESIAN_POINT('Ctrl Pts',(18.3335757493505,65.9985070366392,33.9785196366098));
#17420=CARTESIAN_POINT('Ctrl Pts',(18.3376145958483,66.4361202143717,33.9492295708481));
#17421=CARTESIAN_POINT('Ctrl Pts',(18.5146051520986,66.8766244384234,33.9199395050864));
#17422=CARTESIAN_POINT('Ctrl Pts',(18.8239357934279,67.1839061408327,33.8906494393247));
#17423=CARTESIAN_POINT('Ctrl Pts',(19.2151592084583,67.5725381770135,33.8536050666609));
#17424=CARTESIAN_POINT('Ctrl Pts',(19.8180701191298,67.7480711967276,33.816560693997));
#17425=CARTESIAN_POINT('Ctrl Pts',(20.3567646288979,67.6301778340091,33.7795163213331));
#17426=CARTESIAN_POINT('Ctrl Pts',(20.895459138666,67.5122844712905,33.7424719486693));
#17427=CARTESIAN_POINT('Ctrl Pts',(21.3699372475307,67.1009647261393,33.7054275760055));
#17428=CARTESIAN_POINT('Ctrl Pts',(21.5630684345601,66.5844466094772,33.6683832033416));
#17429=CARTESIAN_POINT('Ctrl Pts',(21.7561996215896,66.0679284928152,33.6313388306778));
#17430=CARTESIAN_POINT('Ctrl Pts',(21.6679838867839,65.4462120046424,33.5942944580139));
#17431=CARTESIAN_POINT('Ctrl Pts',(21.3387904867984,65.0038068447832,33.55725008535));
#17432=CARTESIAN_POINT('Ctrl Pts',(21.009597086813,64.5614016849239,33.5202057126862));
#17433=CARTESIAN_POINT('Ctrl Pts',(20.4394260216479,64.2983078533782,33.4831613400223));
#17434=CARTESIAN_POINT('Ctrl Pts',(19.8891987914095,64.3349222653105,33.4461169673585));
#17435=CARTESIAN_POINT('Ctrl Pts',(19.3389715611711,64.3715366772429,33.4090725946947));
#17436=CARTESIAN_POINT('Ctrl Pts',(18.8086881658594,64.7078593326534,33.3720282220308));
#17437=CARTESIAN_POINT('Ctrl Pts',(18.54101672313,65.1899823655538,33.3349838493669));
#17438=CARTESIAN_POINT('Ctrl Pts',(18.4050189434904,65.4349381266877,33.3161624451146));
#17439=CARTESIAN_POINT('Ctrl Pts',(18.3368124767972,65.7175311656414,33.2973410408622));
#17440=CARTESIAN_POINT('Ctrl Pts',(18.3367009922703,66.0000736897305,33.2785196366098));
#17441=CARTESIAN_POINT('Ctrl Pts',(18.3342212861325,66.001521965989,33.4714803633902));
#17442=CARTESIAN_POINT('Ctrl Pts',(18.3379973609565,65.5848067610909,33.4993440436554));
#17443=CARTESIAN_POINT('Ctrl Pts',(18.4965162756366,65.1655298511734,33.5272077239205));
#17444=CARTESIAN_POINT('Ctrl Pts',(18.779340888906,64.8621280210291,33.5550714041857));
#17445=CARTESIAN_POINT('Ctrl Pts',(19.1553522511079,64.4587595371892,33.5921157768496));
#17446=CARTESIAN_POINT('Ctrl Pts',(19.7510780387978,64.2602040817917,33.6291601495134));
#17447=CARTESIAN_POINT('Ctrl Pts',(20.29390240791,64.3573245366126,33.6662045221773));
#17448=CARTESIAN_POINT('Ctrl Pts',(20.8367267770223,64.4544449914334,33.7032488948411));
#17449=CARTESIAN_POINT('Ctrl Pts',(21.3266497275569,64.8472413564726,33.740293267505));
#17450=CARTESIAN_POINT('Ctrl Pts',(21.5394728754595,65.3559622892128,33.7773376401688));
#17451=CARTESIAN_POINT('Ctrl Pts',(21.7522960233621,65.864683221953,33.8143820128327));
#17452=CARTESIAN_POINT('Ctrl Pts',(21.6880193686326,66.4893287223942,33.8514263854965));
#17453=CARTESIAN_POINT('Ctrl Pts',(21.3760571740258,66.944048708093,33.8884707581604));
#17454=CARTESIAN_POINT('Ctrl Pts',(21.0640949794191,67.3987686937919,33.9255151308242));
#17455=CARTESIAN_POINT('Ctrl Pts',(20.5044472449351,67.6835631647483,33.9625595034881));
#17456=CARTESIAN_POINT('Ctrl Pts',(19.9532197864407,67.6681045833766,33.9996038761519));
#17457=CARTESIAN_POINT('Ctrl Pts',(19.4019923279463,67.6526460020049,34.0366482488158));
#17458=CARTESIAN_POINT('Ctrl Pts',(18.8591851454414,67.3369343683051,34.0736926214796));
#17459=CARTESIAN_POINT('Ctrl Pts',(18.5731974903607,66.8654455050557,34.1107369941435));
#17460=CARTESIAN_POINT('Ctrl Pts',(18.4168817669606,66.607738148026,34.1309847838924));
#17461=CARTESIAN_POINT('Ctrl Pts',(18.337291379463,66.3034920391225,34.1512325736413));
#17462=CARTESIAN_POINT('Ctrl Pts',(18.3366059400397,65.999580177369,34.1714803633902));
#17463=CARTESIAN_POINT('Origin',(20.,66.,30.));
#17464=CARTESIAN_POINT('',(18.332682423241,65.9986976781594,34.8714803633902));
#17465=CARTESIAN_POINT('',(18.3317911471719,66.0008588710395,34.6785196366098));
#17466=CARTESIAN_POINT('',(18.334,66.,30.));
#17467=CARTESIAN_POINT('Ctrl Pts',(18.3317911471719,66.0008588710395,34.6785196366098));
#17468=CARTESIAN_POINT('Ctrl Pts',(18.3314810976279,66.050216623889,34.6752068461617));
#17469=CARTESIAN_POINT('Ctrl Pts',(18.3334818189716,66.0995488884736,34.6718940557137));
#17470=CARTESIAN_POINT('Ctrl Pts',(18.3378751477734,66.1486671473684,34.6685812652656));
#17471=CARTESIAN_POINT('Ctrl Pts',(18.3870023448957,66.6979186365989,34.6315368926018));
#17472=CARTESIAN_POINT('Ctrl Pts',(18.73530640953,67.220410386499,34.594492519938));
#17473=CARTESIAN_POINT('Ctrl Pts',(19.2233963781913,67.4770401011375,34.5574481472741));
#17474=CARTESIAN_POINT('Ctrl Pts',(19.7114863468526,67.7336698157761,34.5204037746102));
#17475=CARTESIAN_POINT('Ctrl Pts',(20.3393622195409,67.7244374951531,34.4833594019464));
#17476=CARTESIAN_POINT('Ctrl Pts',(20.8196957251835,67.4535679248572,34.4463150292825));
#17477=CARTESIAN_POINT('Ctrl Pts',(21.300029230826,67.1826983545613,34.4092706566187));
#17478=CARTESIAN_POINT('Ctrl Pts',(21.6328203694228,66.6501915345925,34.3722262839548));
#17479=CARTESIAN_POINT('Ctrl Pts',(21.6657773241773,66.0997331185797,34.335181911291));
#17480=CARTESIAN_POINT('Ctrl Pts',(21.6987342789318,65.5492747025669,34.2981375386271));
#17481=CARTESIAN_POINT('Ctrl Pts',(21.4318570498441,64.9808646905101,34.2610931659632));
#17482=CARTESIAN_POINT('Ctrl Pts',(20.9872739303598,64.6546186634519,34.2240487932994));
#17483=CARTESIAN_POINT('Ctrl Pts',(20.5426908108755,64.3283726363937,34.1870044206355));
#17484=CARTESIAN_POINT('Ctrl Pts',(19.9204018009947,64.2442905943341,34.1499600479717));
#17485=CARTESIAN_POINT('Ctrl Pts',(19.4051785874718,64.440850147818,34.1129156753078));
#17486=CARTESIAN_POINT('Ctrl Pts',(18.8899553739489,64.6374097013019,34.075871302644));
#17487=CARTESIAN_POINT('Ctrl Pts',(18.481797956784,65.1146108503293,34.0388269299801));
#17488=CARTESIAN_POINT('Ctrl Pts',(18.3674872078961,65.6540769511668,34.0017825573163));
#17489=CARTESIAN_POINT('Ctrl Pts',(18.3435591301517,65.7670005994404,33.9940282504141));
#17490=CARTESIAN_POINT('Ctrl Pts',(18.3325064975594,65.8826525038369,33.986273943512));
#17491=CARTESIAN_POINT('Ctrl Pts',(18.3335757493505,65.9985070366392,33.9785196366098));
#17492=CARTESIAN_POINT('Ctrl Pts',(18.3366059400397,65.999580177369,34.1714803633902));
#17493=CARTESIAN_POINT('Ctrl Pts',(18.3360373327868,65.7474696582416,34.1882769463052));
#17494=CARTESIAN_POINT('Ctrl Pts',(18.3897676052821,65.4955891531532,34.2050735292201));
#17495=CARTESIAN_POINT('Ctrl Pts',(18.4990410118861,65.2706966028902,34.2218701121351));
#17496=CARTESIAN_POINT('Ctrl Pts',(18.7400403161485,64.7747026567731,34.2589144847989));
#17497=CARTESIAN_POINT('Ctrl Pts',(19.2512070523296,64.4099808573381,34.2959588574628));
#17498=CARTESIAN_POINT('Ctrl Pts',(19.7986212717497,64.3434349426867,34.3330032301266));
#17499=CARTESIAN_POINT('Ctrl Pts',(20.3460354911699,64.2768890280352,34.3700476027905));
#17500=CARTESIAN_POINT('Ctrl Pts',(20.929697193829,64.5085189981672,34.4070919754543));
#17501=CARTESIAN_POINT('Ctrl Pts',(21.2825112793764,64.932326689458,34.4441363481182));
#17502=CARTESIAN_POINT('Ctrl Pts',(21.6353253649239,65.3561343807487,34.481180720782));
#17503=CARTESIAN_POINT('Ctrl Pts',(21.7572918333596,65.9721197931981,34.5182250934459));
#17504=CARTESIAN_POINT('Ctrl Pts',(21.5925964660647,66.498395342926,34.5552694661097));
#17505=CARTESIAN_POINT('Ctrl Pts',(21.4279010987698,67.0246708926539,34.5923138387736));
#17506=CARTESIAN_POINT('Ctrl Pts',(20.9765438957441,67.4612365796603,34.6293582114374));
#17507=CARTESIAN_POINT('Ctrl Pts',(20.4450747207132,67.6083124241619,34.6664025841013));
#17508=CARTESIAN_POINT('Ctrl Pts',(19.9136055456824,67.7553882686635,34.7034469567651));
#17509=CARTESIAN_POINT('Ctrl Pts',(19.3020243986463,67.6129742706603,34.740491329429));
#17510=CARTESIAN_POINT('Ctrl Pts',(18.8902029978432,67.2462397444944,34.7775357020928));
#17511=CARTESIAN_POINT('Ctrl Pts',(18.5420761503954,66.9362263887159,34.808850589192));
#17512=CARTESIAN_POINT('Ctrl Pts',(18.3366957110857,66.465915724442,34.8401654762911));
#17513=CARTESIAN_POINT('Ctrl Pts',(18.332682423241,65.9986976781594,34.8714803633902));
#17514=CARTESIAN_POINT('Origin',(20.,66.,30.));
#17515=CARTESIAN_POINT('',(18.3325226254757,66.0012132166996,35.5714803633902));
#17516=CARTESIAN_POINT('',(18.3361559304958,66.0009441564151,35.3785196366098));
#17517=CARTESIAN_POINT('',(18.334,66.,30.));
#17518=CARTESIAN_POINT('',(21.2690708798523,67.0793586530486,36.));
#17519=CARTESIAN_POINT('Ctrl Pts',(18.3325226254757,66.0012132166996,35.5714803633902));
#17520=CARTESIAN_POINT('Ctrl Pts',(18.3364573202891,65.5283746677229,35.6031871242686));
#17521=CARTESIAN_POINT('Ctrl Pts',(18.5476201467709,65.0525511517719,35.6348938851469));
#17522=CARTESIAN_POINT('Ctrl Pts',(18.9034043931841,64.742267480559,35.6666006460253));
#17523=CARTESIAN_POINT('Ctrl Pts',(19.3190824330385,64.3797497200092,35.7036450186892));
#17524=CARTESIAN_POINT('Ctrl Pts',(19.9321723852594,64.2431980531274,35.7406893913531));
#17525=CARTESIAN_POINT('Ctrl Pts',(20.4620470219442,64.396190694787,35.7777337640169));
#17526=CARTESIAN_POINT('Ctrl Pts',(20.991921658629,64.5491833364465,35.8147781366808));
#17527=CARTESIAN_POINT('Ctrl Pts',(21.4385809797777,64.9917202866474,35.8518225093446));
#17528=CARTESIAN_POINT('Ctrl Pts',(21.5975925396924,65.518769581225,35.8888668820084));
#17529=CARTESIAN_POINT('Ctrl Pts',(21.7566040996072,66.0458188758026,35.9259112546723));
#17530=CARTESIAN_POINT('Ctrl Pts',(21.627967898288,66.6573805147569,35.9629556273362));
#17531=CARTESIAN_POINT('Ctrl Pts',(21.2690708798523,67.0793586530486,36.));
#17532=CARTESIAN_POINT('',(18.7285278825024,67.0812050123663,36.));
#17533=CARTESIAN_POINT('Origin',(20.,66.,36.));
#17534=CARTESIAN_POINT('Ctrl Pts',(18.7285264260868,67.0812061322332,36.));
#17535=CARTESIAN_POINT('Ctrl Pts',(19.0793427026358,67.4926761270889,35.9636818543909));
#17536=CARTESIAN_POINT('Ctrl Pts',(19.6492096450092,67.7187174715531,35.9273637087819));
#17537=CARTESIAN_POINT('Ctrl Pts',(20.1865491476251,67.6581952048996,35.8910455631728));
#17538=CARTESIAN_POINT('Ctrl Pts',(20.7346334302361,67.596462719312,35.8540011905089));
#17539=CARTESIAN_POINT('Ctrl Pts',(21.2488764127446,67.2365916395225,35.8169568178451));
#17540=CARTESIAN_POINT('Ctrl Pts',(21.4942849783746,66.7428459429767,35.7799124451812));
#17541=CARTESIAN_POINT('Ctrl Pts',(21.7396935440046,66.249100246431,35.7428680725174));
#17542=CARTESIAN_POINT('Ctrl Pts',(21.7162676927562,65.6214799331291,35.7058236998535));
#17543=CARTESIAN_POINT('Ctrl Pts',(21.4345599518354,65.1474062012195,35.6687793271897));
#17544=CARTESIAN_POINT('Ctrl Pts',(21.1528522109146,64.6733324693098,35.6317349545258));
#17545=CARTESIAN_POINT('Ctrl Pts',(20.6128625803214,64.3528053187923,35.594690581862));
#17546=CARTESIAN_POINT('Ctrl Pts',(20.0617849940283,64.3323991219251,35.5576462091981));
#17547=CARTESIAN_POINT('Ctrl Pts',(19.5107074077351,64.3119929250578,35.5206018365343));
#17548=CARTESIAN_POINT('Ctrl Pts',(18.948541865742,64.5917076818407,35.4835574638704));
#17549=CARTESIAN_POINT('Ctrl Pts',(18.6325042241011,65.0435931575014,35.4465130912065));
#17550=CARTESIAN_POINT('Ctrl Pts',(18.4391461016429,65.32006568997,35.423848606341));
#17551=CARTESIAN_POINT('Ctrl Pts',(18.3379194624106,65.6609857867967,35.4011841214754));
#17552=CARTESIAN_POINT('Ctrl Pts',(18.3361559304958,66.0009441564151,35.3785196366098));
#17553=CARTESIAN_POINT('Origin',(20.,66.,37.5459252805377));
#17554=CARTESIAN_POINT('',(17.9445921240961,66.0018230781907,25.3540747194623));
#17555=CARTESIAN_POINT('',(17.9470733212015,65.9984939638888,25.2959252805377));
#17556=CARTESIAN_POINT('',(17.94525,66.0000000000002,37.5459252805377));
#17557=CARTESIAN_POINT('',(21.8174278887594,66.9586205879593,25.));
#17558=CARTESIAN_POINT('Ctrl Pts',(17.9470733212015,65.9984939638888,25.2959252805377));
#17559=CARTESIAN_POINT('Ctrl Pts',(17.9500635365654,66.4524190943363,25.2713722656862));
#17560=CARTESIAN_POINT('Ctrl Pts',(18.3216914342811,67.5959824757237,25.2097748781708));
#17561=CARTESIAN_POINT('Ctrl Pts',(20.2159933450493,68.4179588201339,25.1111331179916));
#17562=CARTESIAN_POINT('Ctrl Pts',(21.4986774253635,67.5629326473988,25.0370443726639));
#17563=CARTESIAN_POINT('Ctrl Pts',(21.8174278887594,66.9586205879593,25.));
#17564=CARTESIAN_POINT('',(22.0570978955383,65.924544719602,25.));
#17565=CARTESIAN_POINT('Origin',(20.,66.,25.));
#17566=CARTESIAN_POINT('Ctrl Pts',(17.9445921240961,66.0018230781907,25.3540747194623));
#17567=CARTESIAN_POINT('Ctrl Pts',(17.9432975429406,66.1421866078242,25.3464567039116));
#17568=CARTESIAN_POINT('Ctrl Pts',(18.0204258713679,66.9636910465588,25.3017943156971));
#17569=CARTESIAN_POINT('Ctrl Pts',(19.1263753077513,68.2659593106943,25.2200875548188));
#17570=CARTESIAN_POINT('Ctrl Pts',(21.4138495931967,67.965112977645,25.109680663882));
#17571=CARTESIAN_POINT('Ctrl Pts',(22.080681931349,66.5910225805,25.0363181456091));
#17572=CARTESIAN_POINT('Ctrl Pts',(22.0571001530702,65.9245445252813,25.));
#17573=CARTESIAN_POINT('Origin',(20.,66.,37.5459252805377));
#17574=CARTESIAN_POINT('',(17.9485832333138,65.9999504083724,26.0540747194623));
#17575=CARTESIAN_POINT('',(17.9419860794096,65.9995169087598,25.9959252805377));
#17576=CARTESIAN_POINT('',(17.94525,66.0000000000002,37.5459252805377));
#17577=CARTESIAN_POINT('Ctrl Pts',(17.9419860794096,65.9995169087598,25.9959252805377));
#17578=CARTESIAN_POINT('Ctrl Pts',(17.9440551104146,66.6536075979329,25.9603051683359));
#17579=CARTESIAN_POINT('Ctrl Pts',(18.6350687743765,67.991716020834,25.8876406834704));
#17580=CARTESIAN_POINT('Ctrl Pts',(20.9141747100121,68.249987107151,25.7779318259409));
#17581=CARTESIAN_POINT('Ctrl Pts',(22.3860297127563,66.4524069399739,25.6667987079494));
#17582=CARTESIAN_POINT('Ctrl Pts',(21.6743955698345,64.2406214035846,25.5556655899578));
#17583=CARTESIAN_POINT('Ctrl Pts',(19.4296920915163,63.6393770033003,25.4445324719662));
#17584=CARTESIAN_POINT('Ctrl Pts',(18.0884941577881,64.8537199906368,25.3579523688262));
#17585=CARTESIAN_POINT('Ctrl Pts',(17.9455520477338,65.7675593410441,25.30841663835));
#17586=CARTESIAN_POINT('Ctrl Pts',(17.9470733212015,65.9984939638888,25.2959252805377));
#17587=CARTESIAN_POINT('Ctrl Pts',(17.9485832333138,65.9999504083724,26.0540747194623));
#17588=CARTESIAN_POINT('Ctrl Pts',(17.948657249995,66.3458999876025,26.0353896065614));
#17589=CARTESIAN_POINT('Ctrl Pts',(18.1957459993379,67.3778154487128,25.9796601209967));
#17590=CARTESIAN_POINT('Ctrl Pts',(19.8298599336245,68.4226484781515,25.8868862627681));
#17591=CARTESIAN_POINT('Ctrl Pts',(21.9430509921809,67.4569397340099,25.7757531447766));
#17592=CARTESIAN_POINT('Ctrl Pts',(22.2779267956692,65.1577888874642,25.664620026785));
#17593=CARTESIAN_POINT('Ctrl Pts',(20.5278716209092,63.6294498681163,25.5534869087934));
#17594=CARTESIAN_POINT('Ctrl Pts',(18.4479227214906,64.22679670444,25.4499718063526));
#17595=CARTESIAN_POINT('Ctrl Pts',(17.9495927449455,65.459636294612,25.3835010765755));
#17596=CARTESIAN_POINT('Ctrl Pts',(17.9445921240961,66.0018230781907,25.3540747194623));
#17597=CARTESIAN_POINT('Origin',(20.,66.,37.5459252805377));
#17598=CARTESIAN_POINT('',(17.9444688311789,65.998193668761,26.7540747194623));
#17599=CARTESIAN_POINT('',(17.9457761896405,66.0018654840515,26.6959252805377));
#17600=CARTESIAN_POINT('',(17.94525,66.0000000000002,37.5459252805377));
#17601=CARTESIAN_POINT('Ctrl Pts',(17.9457761896405,66.0018654840515,26.6959252805377));
#17602=CARTESIAN_POINT('Ctrl Pts',(17.9441910723939,66.1797860150858,26.6862824436496));
#17603=CARTESIAN_POINT('Ctrl Pts',(18.0468091346947,67.0394145421733,26.6395952340976));
#17604=CARTESIAN_POINT('Ctrl Pts',(19.2507940995179,68.310165311319,26.5558636518818));
#17605=CARTESIAN_POINT('Ctrl Pts',(21.5344924689199,67.8824201691326,26.4447305338903));
#17606=CARTESIAN_POINT('Ctrl Pts',(22.4137605469628,65.7318111515436,26.3335974158987));
#17607=CARTESIAN_POINT('Ctrl Pts',(21.0838647269646,63.8266568213479,26.2224642979072));
#17608=CARTESIAN_POINT('Ctrl Pts',(18.7619637584228,63.9106363014535,26.1113311799156));
#17609=CARTESIAN_POINT('Ctrl Pts',(17.9542068529918,65.2670451819344,26.0358181741258));
#17610=CARTESIAN_POINT('Ctrl Pts',(17.9419033497697,65.9733632711195,25.9973495409998));
#17611=CARTESIAN_POINT('Ctrl Pts',(17.9419860794096,65.9995169087598,25.9959252805377));
#17612=CARTESIAN_POINT('Ctrl Pts',(17.9444688311789,65.998193668761,26.7540747194623));
#17613=CARTESIAN_POINT('Ctrl Pts',(17.9494992489566,66.5462599810788,26.7243225092112));
#17614=CARTESIAN_POINT('Ctrl Pts',(18.4568949548124,67.7849444524044,26.6575259262962));
#17615=CARTESIAN_POINT('Ctrl Pts',(20.5486976409782,68.3658195058375,26.5536849707175));
#17616=CARTESIAN_POINT('Ctrl Pts',(22.2852057779767,66.8221949443221,26.4425518527259));
#17617=CARTESIAN_POINT('Ctrl Pts',(21.9302043029995,64.5260653118046,26.3314187347344));
#17618=CARTESIAN_POINT('Ctrl Pts',(19.8086025603331,63.5789385134492,26.2202856167428));
#17619=CARTESIAN_POINT('Ctrl Pts',(18.1894355754228,64.6343488156836,26.1278376116521));
#17620=CARTESIAN_POINT('Ctrl Pts',(17.9485105074231,65.6600339078047,26.0724339792253));
#17621=CARTESIAN_POINT('Ctrl Pts',(17.9485832333138,65.9999504083724,26.0540747194623));
#17622=CARTESIAN_POINT('Origin',(20.,66.,37.5459252805377));
#17623=CARTESIAN_POINT('',(17.9427073334353,66.0011828701398,27.4540747194623));
#17624=CARTESIAN_POINT('',(17.9483912883566,65.9993486074671,27.3959252805377));
#17625=CARTESIAN_POINT('',(17.94525,66.0000000000002,37.5459252805377));
#17626=CARTESIAN_POINT('Ctrl Pts',(17.9483912883566,65.999348607467,27.3959252805377));
#17627=CARTESIAN_POINT('Ctrl Pts',(17.9494813165331,66.3826975665212,27.3752153462993));
#17628=CARTESIAN_POINT('Ctrl Pts',(18.2366610493634,67.453268789384,27.3174610393972));
#17629=CARTESIAN_POINT('Ctrl Pts',(19.9621345909966,68.4283200411723,27.2226623598312));
#17630=CARTESIAN_POINT('Ctrl Pts',(22.0195745485331,67.3488849730689,27.1115292418396));
#17631=CARTESIAN_POINT('Ctrl Pts',(22.2286203516014,65.0348973043881,27.0003961238481));
#17632=CARTESIAN_POINT('Ctrl Pts',(20.3979451669564,63.6042095721724,26.8892630058565));
#17633=CARTESIAN_POINT('Ctrl Pts',(18.3935017636324,64.300123176515,26.787772724753));
#17634=CARTESIAN_POINT('Ctrl Pts',(17.9502805328587,65.496278191333,26.7233268163134));
#17635=CARTESIAN_POINT('Ctrl Pts',(17.9457761896405,66.0018654840515,26.6959252805377));
#17636=CARTESIAN_POINT('Ctrl Pts',(17.9427073334353,66.0011828701398,27.4540747194623));
#17637=CARTESIAN_POINT('Ctrl Pts',(17.9422311397102,66.0705663093613,27.4502997845249));
#17638=CARTESIAN_POINT('Ctrl Pts',(17.9768968009426,66.8203451915429,27.4094804769235));
#17639=CARTESIAN_POINT('Ctrl Pts',(18.8966146610587,68.1634952415589,27.3316167966584));
#17640=CARTESIAN_POINT('Ctrl Pts',(21.2191694244532,68.1004277622309,27.2204836786668));
#17641=CARTESIAN_POINT('Ctrl Pts',(22.4258923392674,66.1149661220525,27.1093505606753));
#17642=CARTESIAN_POINT('Ctrl Pts',(21.4123431135179,64.0242829635948,26.9982174426837));
#17643=CARTESIAN_POINT('Ctrl Pts',(19.1061618600091,63.7418537970392,26.8870843246921));
#17644=CARTESIAN_POINT('Ctrl Pts',(18.0164474023229,65.0484776654923,26.8057034169517));
#17645=CARTESIAN_POINT('Ctrl Pts',(17.9432358934196,65.8638645372895,26.7613668818751));
#17646=CARTESIAN_POINT('Ctrl Pts',(17.9444688311789,65.998193668761,26.7540747194623));
#17647=CARTESIAN_POINT('Origin',(20.,66.,37.5459252805377));
#17648=CARTESIAN_POINT('',(17.9480453685107,66.0010551247654,28.1540747194623));
#17649=CARTESIAN_POINT('',(17.9433900326703,65.9984792506554,28.0959252805377));
#17650=CARTESIAN_POINT('',(17.94525,66.0000000000002,37.5459252805377));
#17651=CARTESIAN_POINT('Ctrl Pts',(17.9433900326703,65.9984792506554,28.0959252805377));
#17652=CARTESIAN_POINT('Ctrl Pts',(17.9482331665523,66.5830501664587,28.0641482489491));
#17653=CARTESIAN_POINT('Ctrl Pts',(18.5151173418414,67.8573001141241,27.9953268446968));
#17654=CARTESIAN_POINT('Ctrl Pts',(20.6768128607374,68.3324014127664,27.8894610677805));
#17655=CARTESIAN_POINT('Ctrl Pts',(22.3266175536682,66.6964357531696,27.778327949789));
#17656=CARTESIAN_POINT('Ctrl Pts',(21.8470102861031,64.4230646811199,27.6671948317974));
#17657=CARTESIAN_POINT('Ctrl Pts',(19.6769465082846,63.592966879896,27.5560617138059));
#17658=CARTESIAN_POINT('Ctrl Pts',(18.1518517268107,64.7100346416723,27.4656385300526));
#17659=CARTESIAN_POINT('Ctrl Pts',(17.9475315561177,65.6969917822298,27.4122597189632));
#17660=CARTESIAN_POINT('Ctrl Pts',(17.9483912883566,65.999348607467,27.3959252805377));
#17661=CARTESIAN_POINT('Ctrl Pts',(17.9480453685107,66.0010551247654,28.1540747194623));
#17662=CARTESIAN_POINT('Ctrl Pts',(17.9467675578732,66.2756710572213,28.1392326871747));
#17663=CARTESIAN_POINT('Ctrl Pts',(18.1259278433178,67.2341046560269,28.0873462822231));
#17664=CARTESIAN_POINT('Ctrl Pts',(19.5805009712835,68.3921102462499,27.9984155046077));
#17665=CARTESIAN_POINT('Ctrl Pts',(21.7821629259284,67.6498685313834,27.8872823866162));
#17666=CARTESIAN_POINT('Ctrl Pts',(22.3527192254304,65.3976021983889,27.7761492686246));
#17667=CARTESIAN_POINT('Ctrl Pts',(20.7699742878597,63.6966740436017,27.6650161506331));
#17668=CARTESIAN_POINT('Ctrl Pts',(18.5602181548524,64.0900099607333,27.557657967579));
#17669=CARTESIAN_POINT('Ctrl Pts',(17.9469041468234,65.3896894143134,27.4873441571887));
#17670=CARTESIAN_POINT('Ctrl Pts',(17.9427073334353,66.0011828701398,27.4540747194623));
#17671=CARTESIAN_POINT('Origin',(20.,66.,37.5459252805377));
#17672=CARTESIAN_POINT('',(17.9465562858968,65.9982462861091,28.8540747194623));
#17673=CARTESIAN_POINT('',(17.943661294952,66.0016161416468,28.7959252805377));
#17674=CARTESIAN_POINT('',(17.94525,66.0000000000002,37.5459252805377));
#17675=CARTESIAN_POINT('Ctrl Pts',(17.943661294952,66.0016161416468,28.7959252805377));
#17676=CARTESIAN_POINT('Ctrl Pts',(17.9427401513473,66.1083451948514,28.7901255242628));
#17677=CARTESIAN_POINT('Ctrl Pts',(17.9988247250069,66.8958068468452,28.747281395324));
#17678=CARTESIAN_POINT('Ctrl Pts',(19.0161588257614,68.2204117957101,28.6673928937215));
#17679=CARTESIAN_POINT('Ctrl Pts',(21.3318253046188,68.0308651744107,28.5562597757299));
#17680=CARTESIAN_POINT('Ctrl Pts',(22.4285528445608,65.982590811414,28.4451266577383));
#17681=CARTESIAN_POINT('Ctrl Pts',(21.3025732342425,63.9502500230349,28.3339935397468));
#17682=CARTESIAN_POINT('Ctrl Pts',(18.9844273311818,63.7939210909379,28.2228604217552));
#17683=CARTESIAN_POINT('Ctrl Pts',(17.9928405311673,65.1240506743191,28.1435043353522));
#17684=CARTESIAN_POINT('Ctrl Pts',(17.9425872377976,65.9015811377,28.101192621613));
#17685=CARTESIAN_POINT('Ctrl Pts',(17.9433900326703,65.9984792506554,28.0959252805377));
#17686=CARTESIAN_POINT('Ctrl Pts',(17.9465562858968,65.9982462861091,28.8540747194623));
#17687=CARTESIAN_POINT('Ctrl Pts',(17.9504440293497,66.476757915502,28.8281655898244));
#17688=CARTESIAN_POINT('Ctrl Pts',(18.3555440463461,67.6453698738043,28.7652120875227));
#17689=CARTESIAN_POINT('Ctrl Pts',(20.301369074849,68.4098438841618,28.6652142125571));
#17690=CARTESIAN_POINT('Ctrl Pts',(22.1880462145232,67.053861769123,28.5540810945655));
#17691=CARTESIAN_POINT('Ctrl Pts',(22.0721373380047,64.7333438833879,28.442947976574));
#17692=CARTESIAN_POINT('Ctrl Pts',(20.059726811216,63.5721195306752,28.3318148585824));
#17693=CARTESIAN_POINT('Ctrl Pts',(18.2687136043545,64.4913061498983,28.2355237728786));
#17694=CARTESIAN_POINT('Ctrl Pts',(17.9499568578648,65.5902544819065,28.1762770598385));
#17695=CARTESIAN_POINT('Ctrl Pts',(17.9480453685107,66.0010551247654,28.1540747194623));
#17696=CARTESIAN_POINT('Origin',(20.,66.,37.5459252805377));
#17697=CARTESIAN_POINT('',(17.9418458735908,65.9999766228671,29.5540747194623));
#17698=CARTESIAN_POINT('',(17.9484736033439,66.000497180875,29.4959252805377));
#17699=CARTESIAN_POINT('',(17.94525,66.0000000000002,37.5459252805377));
#17700=CARTESIAN_POINT('Ctrl Pts',(17.9484736033439,66.000497180875,29.4959252805377));
#17701=CARTESIAN_POINT('Ctrl Pts',(17.94779755434,66.312740496662,29.4790584269126));
#17702=CARTESIAN_POINT('Ctrl Pts',(18.1614618714719,67.3098805675566,29.4251472006236));
#17703=CARTESIAN_POINT('Ctrl Pts',(19.7114877817388,68.4114171556518,29.3341916016708));
#17704=CARTESIAN_POINT('Ctrl Pts',(21.8694279673096,67.5502938668842,29.2230584836792));
#17705=CARTESIAN_POINT('Ctrl Pts',(22.316394097231,65.2702806121721,29.1119253656877));
#17706=CARTESIAN_POINT('Ctrl Pts',(20.6433051769832,63.6581352626753,29.0007922476961));
#17707=CARTESIAN_POINT('Ctrl Pts',(18.4994791622271,64.1616335930124,28.8954588859795));
#17708=CARTESIAN_POINT('Ctrl Pts',(17.9486237066817,65.4266422691452,28.8271698969266));
#17709=CARTESIAN_POINT('Ctrl Pts',(17.943661294952,66.0016161416468,28.7959252805377));
#17710=CARTESIAN_POINT('Ctrl Pts',(17.9418460022328,65.9999766237505,29.5540747194623));
#17711=CARTESIAN_POINT('Ctrl Pts',(17.9419601590032,66.6788457316685,29.5170984924742));
#17712=CARTESIAN_POINT('Ctrl Pts',(18.6804456694416,68.0380478699251,29.4430778928223));
#17713=CARTESIAN_POINT('Ctrl Pts',(20.9956693718085,68.2151328103185,29.3320129205064));
#17714=CARTESIAN_POINT('Ctrl Pts',(22.4010378181641,66.3649496692051,29.2208798025149));
#17715=CARTESIAN_POINT('Ctrl Pts',(21.6088819494082,64.1807502265562,29.1097466845233));
#17716=CARTESIAN_POINT('Ctrl Pts',(19.3442139955776,63.6615997815364,28.9986135665318));
#17717=CARTESIAN_POINT('Ctrl Pts',(18.0677943199381,64.9047212114679,28.9133895781781));
#17718=CARTESIAN_POINT('Ctrl Pts',(17.9448854089212,65.7925912386986,28.8652099624883));
#17719=CARTESIAN_POINT('Ctrl Pts',(17.9465562858968,65.9982462861091,28.8540747194623));
#17720=CARTESIAN_POINT('Origin',(20.,66.,37.5459252805377));
#17721=CARTESIAN_POINT('',(17.9464881342612,66.0017684723116,30.2540747194623));
#17722=CARTESIAN_POINT('',(17.9454840967242,65.9981221130107,30.1959252805377));
#17723=CARTESIAN_POINT('',(17.94525,66.0000000000002,37.5459252805377));
#17724=CARTESIAN_POINT('Ctrl Pts',(17.9454840967242,65.9981221130106,30.1959252805377));
#17725=CARTESIAN_POINT('Ctrl Pts',(17.9501626777246,66.5133463578346,30.1679913295624));
#17726=CARTESIAN_POINT('Ctrl Pts',(18.4074704589656,67.7192338664832,30.1030130059232));
#17727=CARTESIAN_POINT('Ctrl Pts',(20.4322511218479,68.3898391088773,30.0009903096202));
#17728=CARTESIAN_POINT('Ctrl Pts',(22.2422273876527,66.9330532357364,29.8898571916286));
#17729=CARTESIAN_POINT('Ctrl Pts',(22.0000288950678,64.622300316632,29.778724073637));
#17730=CARTESIAN_POINT('Ctrl Pts',(19.9273252373466,63.5724723734772,29.6675909556455));
#17731=CARTESIAN_POINT('Ctrl Pts',(18.2256189202363,64.5665458908114,29.573324691279));
#17732=CARTESIAN_POINT('Ctrl Pts',(17.9492823488248,65.626966017977,29.5161027995764));
#17733=CARTESIAN_POINT('Ctrl Pts',(17.9484736033439,66.000497180875,29.4959252805377));
#17734=CARTESIAN_POINT('Ctrl Pts',(17.9464881342612,66.0017684723116,30.2540747194623));
#17735=CARTESIAN_POINT('Ctrl Pts',(17.9448197814205,66.2048893181186,30.2430757677879));
#17736=CARTESIAN_POINT('Ctrl Pts',(18.0658215769606,67.0901756412105,30.1950324434495));
#17737=CARTESIAN_POINT('Ctrl Pts',(19.3356363974357,68.3359777115578,30.1099447464474));
#17738=CARTESIAN_POINT('Ctrl Pts',(21.602194400799,67.8251421772989,29.9988116284558));
#17739=CARTESIAN_POINT('Ctrl Pts',(22.402361026794,65.6438646854799,29.8876785104642));
#17740=CARTESIAN_POINT('Ctrl Pts',(21.0037922850585,63.7885362508592,29.7765453924727));
#17741=CARTESIAN_POINT('Ctrl Pts',(18.6865133351581,63.957226481817,29.6654122744811));
#17742=CARTESIAN_POINT('Ctrl Pts',(17.9424133819219,65.3173543283634,29.5912553834777));
#17743=CARTESIAN_POINT('Ctrl Pts',(17.9418457918466,65.9987254957184,29.5541428651381));
#17744=CARTESIAN_POINT('Ctrl Pts',(17.9418460022328,65.9999766237505,29.5540747194623));
#17745=CARTESIAN_POINT('Origin',(20.,66.,37.5459252805377));
#17746=CARTESIAN_POINT('',(17.9480837821526,65.9989795847701,30.9540747194623));
#17747=CARTESIAN_POINT('',(17.9420997627439,66.0006544392236,30.8959252805377));
#17748=CARTESIAN_POINT('',(17.94525,66.0000000000002,37.5459252805377));
#17749=CARTESIAN_POINT('Ctrl Pts',(17.9420997627439,66.0006544392236,30.8959252805377));
#17750=CARTESIAN_POINT('Ctrl Pts',(17.9419499669099,66.0365901229561,30.893968604876));
#17751=CARTESIAN_POINT('Ctrl Pts',(17.9590876919192,66.752725177529,30.8549675565505));
#17752=CARTESIAN_POINT('Ctrl Pts',(18.7920501669056,68.1069003771858,30.7789221355611));
#17753=CARTESIAN_POINT('Ctrl Pts',(21.1149084810719,68.1575799121915,30.6677890175695));
#17754=CARTESIAN_POINT('Ctrl Pts',(22.4173586709909,66.2335573900417,30.556655899578));
#17755=CARTESIAN_POINT('Ctrl Pts',(21.507347058909,64.0957739517965,30.4455227815864));
#17756=CARTESIAN_POINT('Ctrl Pts',(19.2177520899114,63.700813142474,30.3343896635948));
#17757=CARTESIAN_POINT('Ctrl Pts',(18.0396474365576,64.9805047783244,30.2511904965786));
#17758=CARTESIAN_POINT('Ctrl Pts',(17.9439582171286,65.8300860862183,30.2050357022262));
#17759=CARTESIAN_POINT('Ctrl Pts',(17.9454840967242,65.9981221130106,30.1959252805377));
#17760=CARTESIAN_POINT('Ctrl Pts',(17.9480837821526,65.9989795847701,30.9540747194623));
#17761=CARTESIAN_POINT('Ctrl Pts',(17.9499190106596,66.407277615284,30.9320086704376));
#17762=CARTESIAN_POINT('Ctrl Pts',(18.2657185279594,67.503640125688,30.8728982487491));
#17763=CARTESIAN_POINT('Ctrl Pts',(20.0508159985709,68.4280833180919,30.7767434543967));
#17764=CARTESIAN_POINT('Ctrl Pts',(22.0674747085496,67.2742524062426,30.6656103364052));
#17765=CARTESIAN_POINT('Ctrl Pts',(22.1918991902521,64.954175538114,30.5544772184136));
#17766=CARTESIAN_POINT('Ctrl Pts',(20.3102112607245,63.5912783807532,30.4433441004221));
#17767=CARTESIAN_POINT('Ctrl Pts',(18.3589378352584,64.3496381873999,30.3432099341049));
#17768=CARTESIAN_POINT('Ctrl Pts',(17.9504387791389,65.520780092933,30.2801201404517));
#17769=CARTESIAN_POINT('Ctrl Pts',(17.9464881342612,66.0017684723116,30.2540747194623));
#17770=CARTESIAN_POINT('Origin',(20.,66.,37.5459252805377));
#17771=CARTESIAN_POINT('',(17.9427639177081,65.9987822673605,31.6540747194623));
#17772=CARTESIAN_POINT('',(17.9474132077665,66.0014635245165,31.5959252805377));
#17773=CARTESIAN_POINT('',(17.94525,66.0000000000002,37.5459252805377));
#17774=CARTESIAN_POINT('Ctrl Pts',(17.9474132077665,66.0014635245165,31.5959252805377));
#17775=CARTESIAN_POINT('Ctrl Pts',(17.9458281229253,66.2422509216447,31.5829015075258));
#17776=CARTESIAN_POINT('Ctrl Pts',(18.0963189550609,67.1660077074065,31.53283336185));
#17777=CARTESIAN_POINT('Ctrl Pts',(19.4639280035177,68.3687124800713,31.4457208435104));
#17778=CARTESIAN_POINT('Ctrl Pts',(21.6992788050032,67.7351148496642,31.3345877255189));
#17779=CARTESIAN_POINT('Ctrl Pts',(22.3793827611878,65.5134718153893,31.2234546075273));
#17780=CARTESIAN_POINT('Ctrl Pts',(20.8817819627404,63.737118525233,31.1123214895358));
#17781=CARTESIAN_POINT('Ctrl Pts',(18.6177165071394,64.0266543253153,31.0031450472058));
#17782=CARTESIAN_POINT('Ctrl Pts',(17.9447859467341,65.3562449404663,30.9310129775398));
#17783=CARTESIAN_POINT('Ctrl Pts',(17.9420997627439,66.0006544392236,30.8959252805377));
#17784=CARTESIAN_POINT('Ctrl Pts',(17.9427639177081,65.9987822673605,31.6540747194623));
#17785=CARTESIAN_POINT('Ctrl Pts',(17.9470403612663,66.6078147414705,31.6209415730874));
#17786=CARTESIAN_POINT('Ctrl Pts',(18.5560215546316,67.9052027566069,31.5507640540487));
#17787=CARTESIAN_POINT('Ctrl Pts',(20.7615158115174,68.3061362783054,31.4435421623461));
#17788=CARTESIAN_POINT('Ctrl Pts',(22.3504925588018,66.6110283105753,31.3324090443545));
#17789=CARTESIAN_POINT('Ctrl Pts',(21.7882060017851,64.3566831831669,31.2212759263629));
#17790=CARTESIAN_POINT('Ctrl Pts',(19.5892829288324,63.6063662868436,31.1101428083714));
#17791=CARTESIAN_POINT('Ctrl Pts',(18.1282339615618,64.7607922561806,31.0210757394045));
#17792=CARTESIAN_POINT('Ctrl Pts',(17.9468380382272,65.7218289251557,30.9690530431015));
#17793=CARTESIAN_POINT('Ctrl Pts',(17.9480837821526,65.9989795847701,30.9540747194623));
#17794=CARTESIAN_POINT('Origin',(20.,66.,37.5459252805377));
#17795=CARTESIAN_POINT('',(17.9443931880793,66.0017938242215,32.3540747194623));
#17796=CARTESIAN_POINT('',(17.9473846384895,65.9985230106727,32.2959252805377));
#17797=CARTESIAN_POINT('',(17.94525,66.0000000000002,37.5459252805377));
#17798=CARTESIAN_POINT('Ctrl Pts',(17.9473846384895,65.9985230106727,32.2959252805377));
#17799=CARTESIAN_POINT('Ctrl Pts',(17.9503462932394,66.443906616148,32.2718344101756));
#17800=CARTESIAN_POINT('Ctrl Pts',(18.311644403633,67.5785299615268,32.2106991671496));
#17801=CARTESIAN_POINT('Ctrl Pts',(20.1830643623602,68.4217058941771,32.1125195514598));
#17802=CARTESIAN_POINT('Ctrl Pts',(22.133845733665,67.1596871921246,32.0013864334682));
#17803=CARTESIAN_POINT('Ctrl Pts',(22.1316475021699,64.8362771269967,31.8902533154767));
#17804=CARTESIAN_POINT('Ctrl Pts',(20.1784815758609,63.5779520389273,31.7791201974851));
#17805=CARTESIAN_POINT('Ctrl Pts',(18.3099987609922,64.4240616204181,31.6810108525055));
#17806=CARTESIAN_POINT('Ctrl Pts',(17.9503366838091,65.5573635189058,31.6199458801896));
#17807=CARTESIAN_POINT('Ctrl Pts',(17.9474132077665,66.0014635245165,31.5959252805377));
#17808=CARTESIAN_POINT('Ctrl Pts',(17.9443931880793,66.0017938242215,32.3540747194623));
#17809=CARTESIAN_POINT('Ctrl Pts',(17.9431867476929,66.1335998339314,32.3469188484011));
#17810=CARTESIAN_POINT('Ctrl Pts',(18.0147855633186,66.9464311477664,32.302718604676));
#17811=CARTESIAN_POINT('Ctrl Pts',(19.0978804119286,68.2548505746783,32.221473988287));
#17812=CARTESIAN_POINT('Ctrl Pts',(21.4050826420595,67.9808870826703,32.1103408702955));
#17813=CARTESIAN_POINT('Ctrl Pts',(22.4262979346632,65.8939377656472,31.9992077523039));
#17814=CARTESIAN_POINT('Ctrl Pts',(21.2268698593072,63.9040607800724,31.8880746343123));
#17815=CARTESIAN_POINT('Ctrl Pts',(18.9045621995861,63.8324698639393,31.7769415163208));
#17816=CARTESIAN_POINT('Ctrl Pts',(17.978302645581,65.1745805746697,31.6989415447041));
#17817=CARTESIAN_POINT('Ctrl Pts',(17.9422591018274,65.9268885873393,31.6579859457513));
#17818=CARTESIAN_POINT('Ctrl Pts',(17.9427639177081,65.9987822673605,31.6540747194623));
#17819=CARTESIAN_POINT('Origin',(20.,66.,37.5459252805377));
#17820=CARTESIAN_POINT('',(17.9485812508208,66.0000908847383,33.0540747194623));
#17821=CARTESIAN_POINT('',(17.9420826509595,65.9993679635266,32.9959252805377));
#17822=CARTESIAN_POINT('',(17.94525,66.0000000000002,37.5459252805377));
#17823=CARTESIAN_POINT('Ctrl Pts',(17.9420826509595,65.9993679635266,32.9959252805377));
#17824=CARTESIAN_POINT('Ctrl Pts',(17.9446925158973,66.6450537162148,32.9607673128253));
#17825=CARTESIAN_POINT('Ctrl Pts',(18.6199954325073,67.9757741595962,32.8885649724491));
#17826=CARTESIAN_POINT('Ctrl Pts',(20.8860623082748,68.2612088768015,32.7793182594092));
#17827=CARTESIAN_POINT('Ctrl Pts',(22.3802991314904,66.4820249405198,32.6681851414175));
#17828=CARTESIAN_POINT('Ctrl Pts',(21.6959925019048,64.261672806363,32.5570520234261));
#17829=CARTESIAN_POINT('Ctrl Pts',(19.4594467809617,63.6323061397115,32.4459189054344));
#17830=CARTESIAN_POINT('Ctrl Pts',(18.0952173579541,64.836624342483,32.358876657805));
#17831=CARTESIAN_POINT('Ctrl Pts',(17.9457921762395,65.7590431798503,32.3088787828394));
#17832=CARTESIAN_POINT('Ctrl Pts',(17.9473846384895,65.9985230106727,32.2959252805377));
#17833=CARTESIAN_POINT('Ctrl Pts',(17.9485812508208,66.0000908847383,33.0540747194623));
#17834=CARTESIAN_POINT('Ctrl Pts',(17.9484481239615,66.3374829869665,33.0358517510509));
#17835=CARTESIAN_POINT('Ctrl Pts',(18.1868160160139,67.360562003179,32.9805844099755));
#17836=CARTESIAN_POINT('Ctrl Pts',(19.7997191989097,68.420342634033,32.8882726962363));
#17837=CARTESIAN_POINT('Ctrl Pts',(21.924781541228,67.4810087386156,32.7771395782448));
#17838=CARTESIAN_POINT('Ctrl Pts',(22.2882080583246,65.1861973537148,32.6660064602532));
#17839=CARTESIAN_POINT('Ctrl Pts',(20.5573764974643,63.6362101816373,32.5548733422617));
#17840=CARTESIAN_POINT('Ctrl Pts',(18.4607079236377,64.210156628494,32.4508960953314));
#17841=CARTESIAN_POINT('Ctrl Pts',(17.9494322245733,65.4512690734646,32.3839632210649));
#17842=CARTESIAN_POINT('Ctrl Pts',(17.9443931880793,66.0017938242215,32.3540747194623));
#17843=CARTESIAN_POINT('Origin',(20.,66.,37.5459252805377));
#17844=CARTESIAN_POINT('',(17.944726753288,65.9981586635862,33.7540747194623));
#17845=CARTESIAN_POINT('',(17.9455229217772,66.0018771066122,33.6959252805377));
#17846=CARTESIAN_POINT('',(17.94525,66.0000000000002,37.5459252805377));
#17847=CARTESIAN_POINT('Ctrl Pts',(17.9455229217772,66.0018771066122,33.6959252805377));
#17848=CARTESIAN_POINT('Ctrl Pts',(17.9439884406831,66.1712173960156,33.686744588139));
#17849=CARTESIAN_POINT('Ctrl Pts',(18.0405829995419,67.0221239091327,33.6405195230765));
#17850=CARTESIAN_POINT('Ctrl Pts',(19.2221041132247,68.3006629449443,33.55725008535));
#17851=CARTESIAN_POINT('Ctrl Pts',(21.5109476208589,67.9013703706408,33.4461169673585));
#17852=CARTESIAN_POINT('Ctrl Pts',(22.416912395611,65.7618687952487,33.3349838493669));
#17853=CARTESIAN_POINT('Ctrl Pts',(21.1108238171316,63.8403142715337,33.2238507313754));
#17854=CARTESIAN_POINT('Ctrl Pts',(18.7880655596257,63.8953891307446,33.1127176133838));
#17855=CARTESIAN_POINT('Ctrl Pts',(17.9584343459935,65.2498852778546,33.0367424631046));
#17856=CARTESIAN_POINT('Ctrl Pts',(17.9419426183449,65.9647236174436,32.9978116854892));
#17857=CARTESIAN_POINT('Ctrl Pts',(17.9420826509595,65.9993679635266,32.9959252805377));
#17858=CARTESIAN_POINT('Ctrl Pts',(17.944726753288,65.9981586635862,33.7540747194623));
#17859=CARTESIAN_POINT('Ctrl Pts',(17.9497080377066,66.5378859606725,33.7247846537006));
#17860=CARTESIAN_POINT('Ctrl Pts',(18.4440788206969,67.7683042539906,33.6584502152751));
#17861=CARTESIAN_POINT('Ctrl Pts',(20.5192141482499,68.3724644440178,33.5550714041857));
#17862=CARTESIAN_POINT('Ctrl Pts',(22.2747973910883,66.850569042428,33.4439382861942));
#17863=CARTESIAN_POINT('Ctrl Pts',(21.9483965247762,64.5501993772306,33.3328051682026));
#17864=CARTESIAN_POINT('Ctrl Pts',(19.8387464716884,63.5767443045379,33.221672050211));
#17865=CARTESIAN_POINT('Ctrl Pts',(18.1984100230512,64.617098038126,33.1287619006309));
#17866=CARTESIAN_POINT('Ctrl Pts',(17.9487187495192,65.6516189451392,33.0728961237147));
#17867=CARTESIAN_POINT('Ctrl Pts',(17.9485812508208,66.0000908847383,33.0540747194623));
#17868=CARTESIAN_POINT('Origin',(20.,66.,37.5459252805377));
#17869=CARTESIAN_POINT('',(17.9425257260813,66.0010592828743,34.4540747194623));
#17870=CARTESIAN_POINT('',(17.9484640187855,65.9994822145552,34.3959252805377));
#17871=CARTESIAN_POINT('',(17.94525,66.0000000000002,37.5459252805377));
#17872=CARTESIAN_POINT('Ctrl Pts',(17.9484640187855,65.9994822145552,34.3959252805377));
#17873=CARTESIAN_POINT('Ctrl Pts',(17.9493094009313,66.3743098843859,34.3756774907888));
#17874=CARTESIAN_POINT('Ctrl Pts',(18.227064603961,67.4360705115979,34.318385328376));
#17875=CARTESIAN_POINT('Ctrl Pts',(19.9319188439973,68.4276607754887,34.2240487932994));
#17876=CARTESIAN_POINT('Ctrl Pts',(22.0026322577385,67.3739126856969,34.1129156753079));
#17877=CARTESIAN_POINT('Ctrl Pts',(22.2404578093089,65.0627055872007,34.0017825573163));
#17878=CARTESIAN_POINT('Ctrl Pts',(20.4277281887608,63.6093472479493,33.8906494393247));
#17879=CARTESIAN_POINT('Ctrl Pts',(18.4056138422819,64.2833181305728,33.7886970137318));
#17880=CARTESIAN_POINT('Ctrl Pts',(17.9501801185026,65.487924185085,33.7237889608028));
#17881=CARTESIAN_POINT('Ctrl Pts',(17.9455229217772,66.0018771066122,33.6959252805377));
#17882=CARTESIAN_POINT('Ctrl Pts',(17.9425257260813,66.0010592828744,34.4540747194623));
#17883=CARTESIAN_POINT('Ctrl Pts',(17.942143328542,66.061934338497,34.4507619290142));
#17884=CARTESIAN_POINT('Ctrl Pts',(17.972203902059,66.8031450877885,34.4104047659023));
#17885=CARTESIAN_POINT('Ctrl Pts',(18.869777083907,68.1495967375546,34.3330032301266));
#17886=CARTESIAN_POINT('Ctrl Pts',(21.1929366566675,68.1154368741692,34.221870112135));
#17887=CARTESIAN_POINT('Ctrl Pts',(22.4242738572048,66.1451456586872,34.1107369941435));
#17888=CARTESIAN_POINT('Ctrl Pts',(21.4368201000595,64.0420115549533,33.9996038761519));
#17889=CARTESIAN_POINT('Ctrl Pts',(19.1343320873597,63.7309054758618,33.8884707581604));
#17890=CARTESIAN_POINT('Ctrl Pts',(18.0221618776052,65.0312099164754,33.8066277059305));
#17891=CARTESIAN_POINT('Ctrl Pts',(17.9434079987156,65.8552702474544,33.7618290263645));
#17892=CARTESIAN_POINT('Ctrl Pts',(17.944726753288,65.9981586635862,33.7540747194623));
#17893=CARTESIAN_POINT('Origin',(20.,66.,37.5459252805377));
#17894=CARTESIAN_POINT('',(17.9479090025127,66.0011644690241,35.1540747194623));
#17895=CARTESIAN_POINT('',(17.9436249754829,65.9983937900349,35.0959252805377));
#17896=CARTESIAN_POINT('',(17.94525,66.0000000000002,37.5459252805377));
#17897=CARTESIAN_POINT('Ctrl Pts',(17.9436249754829,65.9983937900349,35.0959252805377));
#17898=CARTESIAN_POINT('Ctrl Pts',(17.9485747373069,66.5746340545001,35.0646103934386));
#17899=CARTESIAN_POINT('Ctrl Pts',(18.5015294598482,67.8408719871184,34.9962511336756));
#17900=CARTESIAN_POINT('Ctrl Pts',(20.6477355083213,68.3406417811724,34.8908475012488));
#17901=CARTESIAN_POINT('Ctrl Pts',(22.3177707056507,66.7253356370374,34.7797143832572));
#17902=CARTESIAN_POINT('Ctrl Pts',(21.8664911119801,64.4461711240172,34.6685812652656));
#17903=CARTESIAN_POINT('Ctrl Pts',(19.7069252952836,63.5891332828492,34.5574481472741));
#17904=CARTESIAN_POINT('Ctrl Pts',(18.1601824626538,64.6927474056976,34.4665628190314));
#17905=CARTESIAN_POINT('Ctrl Pts',(17.9477627308186,65.6885433855173,34.4127218634526));
#17906=CARTESIAN_POINT('Ctrl Pts',(17.9484640187855,65.9994822145552,34.3959252805377));
#17907=CARTESIAN_POINT('Ctrl Pts',(17.9479090025127,66.0011644690241,35.1540747194623));
#17908=CARTESIAN_POINT('Ctrl Pts',(17.9465290092682,66.2671875841058,35.139694831664));
#17909=CARTESIAN_POINT('Ctrl Pts',(18.1181887624162,67.2168116767709,35.0882705712019));
#17910=CARTESIAN_POINT('Ctrl Pts',(19.5507726973617,68.3866954932114,34.999801938076));
#17911=CARTESIAN_POINT('Ctrl Pts',(21.761489833587,67.6719231014153,34.8886688200844));
#17912=CARTESIAN_POINT('Ctrl Pts',(22.3600352949887,65.4269244270303,34.7775357020928));
#17913=CARTESIAN_POINT('Ctrl Pts',(20.7985769670495,63.7064353263736,34.6664025841013));
#17914=CARTESIAN_POINT('Ctrl Pts',(18.5745658426963,64.0738149722658,34.5585822565578));
#17915=CARTESIAN_POINT('Ctrl Pts',(17.9464193843856,65.3812156870209,34.4878063016781));
#17916=CARTESIAN_POINT('Ctrl Pts',(17.9425257260813,66.0010592828744,34.4540747194623));
#17917=CARTESIAN_POINT('Origin',(20.,66.,37.5459252805377));
#17918=CARTESIAN_POINT('',(17.9473272485919,65.9976786215907,35.8540747194623));
#17919=CARTESIAN_POINT('',(17.9434278899737,66.0014963127332,35.7959252805377));
#17920=CARTESIAN_POINT('',(17.94525,66.0000000000002,37.5459252805377));
#17921=CARTESIAN_POINT('',(19.4698297828115,64.0148256743283,36.));
#17922=CARTESIAN_POINT('Ctrl Pts',(19.4698297828115,64.0148256743282,36.));
#17923=CARTESIAN_POINT('Ctrl Pts',(18.809740437582,64.1911123142462,35.9629556273362));
#17924=CARTESIAN_POINT('Ctrl Pts',(18.0750704080787,64.8872090652857,35.9143138671569));
#17925=CARTESIAN_POINT('Ctrl Pts',(17.94571015716,65.7834096722511,35.8656721069777));
#17926=CARTESIAN_POINT('Ctrl Pts',(17.9473272485919,65.9976786215907,35.8540747194623));
#17927=CARTESIAN_POINT('',(20.5313110481438,64.0112682685522,36.));
#17928=CARTESIAN_POINT('Origin',(20.,66.,36.));
#17929=CARTESIAN_POINT('Ctrl Pts',(20.5313117419429,64.0112661051077,36.));
#17930=CARTESIAN_POINT('Ctrl Pts',(19.886791318144,63.8399704354172,35.9636818543909));
#17931=CARTESIAN_POINT('Ctrl Pts',(18.5070307177422,64.1592653630963,35.8956569479035));
#17932=CARTESIAN_POINT('Ctrl Pts',(17.9482807196063,65.4183240387177,35.8276320414161));
#17933=CARTESIAN_POINT('Ctrl Pts',(17.9434278899737,66.0014963127332,35.7959252805377));
#17934=CARTESIAN_POINT('Origin',(20.,50.,-32.));
#17935=CARTESIAN_POINT('',(22.5134612402277,50.000273003858,-25.387416697508));
#17936=CARTESIAN_POINT('',(22.5157646541248,49.9966173859026,-25.112583302492));
#17937=CARTESIAN_POINT('',(22.5175,50.,-32.));
#17938=CARTESIAN_POINT('',(21.9134659966651,51.6359872033749,-25.));
#17939=CARTESIAN_POINT('Ctrl Pts',(22.5157646541248,49.9966173859026,-25.112583302492));
#17940=CARTESIAN_POINT('Ctrl Pts',(22.5105547734392,50.5891788966502,-25.0750555349947));
#17941=CARTESIAN_POINT('Ctrl Pts',(22.2992218280841,51.1848035603044,-25.0375277674973));
#17942=CARTESIAN_POINT('Ctrl Pts',(21.9134659966651,51.6359872033749,-25.));
#17943=CARTESIAN_POINT('',(22.5175,50.,-25.));
#17944=CARTESIAN_POINT('Origin',(20.,50.,-25.));
#17945=CARTESIAN_POINT('',(17.4825,50.,-25.));
#17946=CARTESIAN_POINT('Ctrl Pts',(22.5175,50.,-25.));
#17947=CARTESIAN_POINT('Ctrl Pts',(22.5175,50.3222180082023,-25.));
#17948=CARTESIAN_POINT('Ctrl Pts',(22.4519182005811,50.6620957154615,-24.965994767533));
#17949=CARTESIAN_POINT('Ctrl Pts',(22.1930921359231,51.2808669639972,-24.8434341672334));
#17950=CARTESIAN_POINT('Ctrl Pts',(22.0001401774783,51.560142465796,-24.75619390213));
#17951=CARTESIAN_POINT('Ctrl Pts',(21.5595215410958,52.0007611021785,-24.5883213994305));
#17952=CARTESIAN_POINT('Ctrl Pts',(21.2804542351089,52.1932581515168,-24.4956547875015));
#17953=CARTESIAN_POINT('Ctrl Pts',(20.6625974062016,52.4517149721102,-24.3600905047278));
#17954=CARTESIAN_POINT('Ctrl Pts',(20.3231274362054,52.5175,-24.3199761284063));
#17955=CARTESIAN_POINT('Ctrl Pts',(20.,52.5175,-24.3199761284063));
#17956=CARTESIAN_POINT('Ctrl Pts',(19.6768725637946,52.5175,-24.3199761284063));
#17957=CARTESIAN_POINT('Ctrl Pts',(19.3374025937983,52.4517149721102,-24.3600905047278));
#17958=CARTESIAN_POINT('Ctrl Pts',(18.719545764891,52.1932581515168,-24.4956547875015));
#17959=CARTESIAN_POINT('Ctrl Pts',(18.4404784589043,52.0007611021785,-24.5883213994305));
#17960=CARTESIAN_POINT('Ctrl Pts',(17.9998598225217,51.560142465796,-24.75619390213));
#17961=CARTESIAN_POINT('Ctrl Pts',(17.8069078640769,51.2808669639972,-24.8434341672334));
#17962=CARTESIAN_POINT('Ctrl Pts',(17.5480817994189,50.6620957154614,-24.965994767533));
#17963=CARTESIAN_POINT('Ctrl Pts',(17.4825,50.3222180082023,-25.));
#17964=CARTESIAN_POINT('Ctrl Pts',(17.4825,50.,-25.));
#17965=CARTESIAN_POINT('',(18.0829273529947,51.6385409730469,-25.));
#17966=CARTESIAN_POINT('Origin',(20.,50.,-25.));
#17967=CARTESIAN_POINT('Ctrl Pts',(18.0829198466036,51.6385462881155,-25.));
#17968=CARTESIAN_POINT('Ctrl Pts',(18.6057517157272,52.2473168557604,-25.0509462733027));
#17969=CARTESIAN_POINT('Ctrl Pts',(19.445447411393,52.5873619676629,-25.1018925466053));
#17970=CARTESIAN_POINT('Ctrl Pts',(20.2440955124524,52.5095730776923,-25.152838819908));
#17971=CARTESIAN_POINT('Ctrl Pts',(21.0694439951791,52.4291835516607,-25.2054883276388));
#17972=CARTESIAN_POINT('Ctrl Pts',(21.8509544003932,51.9025549819737,-25.2581378353696));
#17973=CARTESIAN_POINT('Ctrl Pts',(22.2348332639616,51.1677991119336,-25.3107873431004));
#17974=CARTESIAN_POINT('Ctrl Pts',(22.4210736218415,50.8113293784386,-25.3363304612363));
#17975=CARTESIAN_POINT('Ctrl Pts',(22.5137217010458,50.4058718100902,-25.3618735793722));
#17976=CARTESIAN_POINT('Ctrl Pts',(22.5134612402277,50.000273003858,-25.387416697508));
#17977=CARTESIAN_POINT('Origin',(20.,50.,-32.));
#17978=CARTESIAN_POINT('',(22.5187558030321,49.9979044734253,-26.387416697508));
#17979=CARTESIAN_POINT('',(22.5213591508609,50.0006703125801,-26.112583302492));
#17980=CARTESIAN_POINT('',(22.5175,50.,-32.));
#17981=CARTESIAN_POINT('Ctrl Pts',(22.5213591508609,50.0006703125801,-26.112583302492));
#17982=CARTESIAN_POINT('Ctrl Pts',(22.5214869459678,50.0371266568132,-26.1102687557771));
#17983=CARTESIAN_POINT('Ctrl Pts',(22.5207639649754,50.0735777470678,-26.1079542090622));
#17984=CARTESIAN_POINT('Ctrl Pts',(22.5191743291001,50.1099909212014,-26.1056396623473));
#17985=CARTESIAN_POINT('Ctrl Pts',(22.4830145290993,50.9382894734454,-26.0529901546165));
#17986=CARTESIAN_POINT('Ctrl Pts',(21.9984162027216,51.7469688557767,-26.0003406468856));
#17987=CARTESIAN_POINT('Ctrl Pts',(21.2850580716506,52.1695270068173,-25.9476911391548));
#17988=CARTESIAN_POINT('Ctrl Pts',(20.5716999405796,52.592085157858,-25.895041631424));
#17989=CARTESIAN_POINT('Ctrl Pts',(19.6295820048153,52.6285220776079,-25.8423921236932));
#17990=CARTESIAN_POINT('Ctrl Pts',(18.8858121581489,52.2621196683134,-25.7897426159623));
#17991=CARTESIAN_POINT('Ctrl Pts',(18.1420423114825,51.8957172590189,-25.7370931082315));
#17992=CARTESIAN_POINT('Ctrl Pts',(17.596620553914,51.1264755206799,-25.6844436005007));
#17993=CARTESIAN_POINT('Ctrl Pts',(17.4967796369456,50.303516827856,-25.6317940927699));
#17994=CARTESIAN_POINT('Ctrl Pts',(17.3969387199773,49.4805581350321,-25.5791445850391));
#17995=CARTESIAN_POINT('Ctrl Pts',(17.7426786436092,48.6038824877232,-25.5264950773082));
#17996=CARTESIAN_POINT('Ctrl Pts',(18.3773140075671,48.0701216980594,-25.4738455695774));
#17997=CARTESIAN_POINT('Ctrl Pts',(19.0119493715251,47.5363609083956,-25.4211960618466));
#17998=CARTESIAN_POINT('Ctrl Pts',(19.935480175809,47.3455149763769,-25.3685465541158));
#17999=CARTESIAN_POINT('Ctrl Pts',(20.7291490582878,47.5857187856067,-25.3158970463849));
#18000=CARTESIAN_POINT('Ctrl Pts',(21.5228179407665,47.8259225948365,-25.2632475386541));
#18001=CARTESIAN_POINT('Ctrl Pts',(22.1866249014401,48.4971761453148,-25.2105980309233));
#18002=CARTESIAN_POINT('Ctrl Pts',(22.4195857619951,49.291445495894,-25.1579485231925));
#18003=CARTESIAN_POINT('Ctrl Pts',(22.4864956680838,49.5195717465001,-25.142826782959));
#18004=CARTESIAN_POINT('Ctrl Pts',(22.5178639653183,49.7578458885432,-25.1277050427255));
#18005=CARTESIAN_POINT('Ctrl Pts',(22.5157646541248,49.9966173859026,-25.112583302492));
#18006=CARTESIAN_POINT('Ctrl Pts',(22.5134612402277,50.000273003858,-25.387416697508));
#18007=CARTESIAN_POINT('Ctrl Pts',(22.5131848388748,49.569851032566,-25.414523087103));
#18008=CARTESIAN_POINT('Ctrl Pts',(22.408279656946,49.1392700064923,-25.4416294766979));
#18009=CARTESIAN_POINT('Ctrl Pts',(22.1995628098958,48.766905021273,-25.4687358662929));
#18010=CARTESIAN_POINT('Ctrl Pts',(21.7941661703386,48.0436499710456,-25.5213853740237));
#18011=CARTESIAN_POINT('Ctrl Pts',(20.9971255693015,47.5400230409839,-25.5740348817546));
#18012=CARTESIAN_POINT('Ctrl Pts',(20.169891281729,47.4841783887763,-25.6266843894854));
#18013=CARTESIAN_POINT('Ctrl Pts',(19.3426569941565,47.4283337365687,-25.6793338972162));
#18014=CARTESIAN_POINT('Ctrl Pts',(18.4852290200485,47.8202713622153,-25.731983404947));
#18015=CARTESIAN_POINT('Ctrl Pts',(17.9862469875704,48.4823913860756,-25.7846329126778));
#18016=CARTESIAN_POINT('Ctrl Pts',(17.4872649550924,49.1445114099359,-25.8372824204087));
#18017=CARTESIAN_POINT('Ctrl Pts',(17.3467288642442,50.07681383201,-25.8899319281395));
#18018=CARTESIAN_POINT('Ctrl Pts',(17.6283799117207,50.856613802331,-25.9425814358703));
#18019=CARTESIAN_POINT('Ctrl Pts',(17.9100309591972,51.6364137726519,-25.9952309436011));
#18020=CARTESIAN_POINT('Ctrl Pts',(18.6138691449983,52.2637112912197,-26.0478804513319));
#18021=CARTESIAN_POINT('Ctrl Pts',(19.4208044095907,52.4541505214686,-26.1005299590628));
#18022=CARTESIAN_POINT('Ctrl Pts',(20.227739674183,52.6445897517174,-26.1531794667936));
#18023=CARTESIAN_POINT('Ctrl Pts',(21.1377720175666,52.3981706936473,-26.2058289745244));
#18024=CARTESIAN_POINT('Ctrl Pts',(21.7383600126164,51.8265936565345,-26.2584784822553));
#18025=CARTESIAN_POINT('Ctrl Pts',(22.2286383806489,51.3599978216689,-26.3014578873395));
#18026=CARTESIAN_POINT('Ctrl Pts',(22.5127043733564,50.6767181159384,-26.3444372924238));
#18027=CARTESIAN_POINT('Ctrl Pts',(22.5187558030321,49.9979044734253,-26.387416697508));
#18028=CARTESIAN_POINT('Origin',(20.,50.,-32.));
#18029=CARTESIAN_POINT('',(22.5196059184078,50.0018577146135,-27.387416697508));
#18030=CARTESIAN_POINT('',(22.514511951768,50.001528002557,-27.112583302492));
#18031=CARTESIAN_POINT('',(22.5175,50.,-32.));
#18032=CARTESIAN_POINT('Ctrl Pts',(22.514511951768,50.001528002557,-27.112583302492));
#18033=CARTESIAN_POINT('Ctrl Pts',(22.5162681753221,50.3148132588407,-27.0928324688287));
#18034=CARTESIAN_POINT('Ctrl Pts',(22.4619720370514,50.6275116919841,-27.0730816351654));
#18035=CARTESIAN_POINT('Ctrl Pts',(22.3488346564514,50.9172322204891,-27.0533308015021));
#18036=CARTESIAN_POINT('Ctrl Pts',(22.0472459996842,51.6895359857549,-27.0006812937713));
#18037=CARTESIAN_POINT('Ctrl Pts',(21.327538634317,52.2985615564516,-26.9480317860404));
#18038=CARTESIAN_POINT('Ctrl Pts',(20.5159808446024,52.4682180646552,-26.8953822783096));
#18039=CARTESIAN_POINT('Ctrl Pts',(19.7044230548878,52.6378745728588,-26.8427327705788));
#18040=CARTESIAN_POINT('Ctrl Pts',(18.8010148408259,52.3681620185693,-26.790083262848));
#18041=CARTESIAN_POINT('Ctrl Pts',(18.2153027880988,51.7813472751723,-26.7374337551172));
#18042=CARTESIAN_POINT('Ctrl Pts',(17.6295907353717,51.1945325317753,-26.6847842473863));
#18043=CARTESIAN_POINT('Ctrl Pts',(17.3615748439794,50.2906155992708,-26.6321347396555));
#18044=CARTESIAN_POINT('Ctrl Pts',(17.5327556249479,49.4793798671285,-26.5794852319247));
#18045=CARTESIAN_POINT('Ctrl Pts',(17.7039364059165,48.6681441349862,-26.5268357241938));
#18046=CARTESIAN_POINT('Ctrl Pts',(18.3143138592458,47.9495896032061,-26.474186216463));
#18047=CARTESIAN_POINT('Ctrl Pts',(19.0871834798727,47.6494493128525,-26.4215367087322));
#18048=CARTESIAN_POINT('Ctrl Pts',(19.8600531004996,47.3493090224989,-26.3688872010014));
#18049=CARTESIAN_POINT('Ctrl Pts',(20.795414888424,47.4675829735717,-26.3162376932706));
#18050=CARTESIAN_POINT('Ctrl Pts',(21.4692351455743,47.9506788101863,-26.2635881855397));
#18051=CARTESIAN_POINT('Ctrl Pts',(22.1134333126076,48.4125370715641,-26.2132532245238));
#18052=CARTESIAN_POINT('Ctrl Pts',(22.5185799623133,49.207846104737,-26.1629182635079));
#18053=CARTESIAN_POINT('Ctrl Pts',(22.5213591508609,50.0006703125801,-26.112583302492));
#18054=CARTESIAN_POINT('Ctrl Pts',(22.5187558030321,49.9979044734253,-26.387416697508));
#18055=CARTESIAN_POINT('Ctrl Pts',(22.5201173376092,49.8451755655187,-26.3970868001546));
#18056=CARTESIAN_POINT('Ctrl Pts',(22.5074051519233,49.6926727397414,-26.4067569028011));
#18057=CARTESIAN_POINT('Ctrl Pts',(22.4798014410344,49.5429148261515,-26.4164270054477));
#18058=CARTESIAN_POINT('Ctrl Pts',(22.3295112276869,48.7275480490366,-26.4690765131785));
#18059=CARTESIAN_POINT('Ctrl Pts',(21.737787154276,47.9935495109622,-26.5217260209094));
#18060=CARTESIAN_POINT('Ctrl Pts',(20.9728803238817,47.6736637582043,-26.5743755286402));
#18061=CARTESIAN_POINT('Ctrl Pts',(20.2079734934874,47.3537780054464,-26.627025036371));
#18062=CARTESIAN_POINT('Ctrl Pts',(19.2698839061096,47.4480050380052,-26.6796745441019));
#18063=CARTESIAN_POINT('Ctrl Pts',(18.5838792098904,47.9136297340241,-26.7323240518327));
#18064=CARTESIAN_POINT('Ctrl Pts',(17.8978745136712,48.3792544300429,-26.7849735595635));
#18065=CARTESIAN_POINT('Ctrl Pts',(17.4639547086106,49.216276789522,-26.8376230672943));
#18066=CARTESIAN_POINT('Ctrl Pts',(17.4788312425904,50.0452448160541,-26.8902725750251));
#18067=CARTESIAN_POINT('Ctrl Pts',(17.4937077765703,50.8742128425862,-26.9429220827559));
#18068=CARTESIAN_POINT('Ctrl Pts',(17.9573806495906,51.6951265361713,-26.9955715904868));
#18069=CARTESIAN_POINT('Ctrl Pts',(18.6596505630897,52.1358374778744,-27.0482210982176));
#18070=CARTESIAN_POINT('Ctrl Pts',(19.3619204765888,52.5765484195774,-27.1008706059484));
#18071=CARTESIAN_POINT('Ctrl Pts',(20.3027874305667,52.6370566093984,-27.1535201136792));
#18072=CARTESIAN_POINT('Ctrl Pts',(21.0557238258934,52.289931418589,-27.2061696214101));
#18073=CARTESIAN_POINT('Ctrl Pts',(21.80866022122,51.9428062277797,-27.2588191291409));
#18074=CARTESIAN_POINT('Ctrl Pts',(22.3736660578954,51.18804765634,-27.3114686368717));
#18075=CARTESIAN_POINT('Ctrl Pts',(22.494604468072,50.3678141060487,-27.3641181446025));
#18076=CARTESIAN_POINT('Ctrl Pts',(22.5124437608419,50.2468237075311,-27.3718843289044));
#18077=CARTESIAN_POINT('Ctrl Pts',(22.5206208613874,50.1244086788925,-27.3796505132062));
#18078=CARTESIAN_POINT('Ctrl Pts',(22.5196059184078,50.0018577146135,-27.387416697508));
#18079=CARTESIAN_POINT('Origin',(20.,50.,-32.));
#18080=CARTESIAN_POINT('',(22.5135351409985,50.0002853817648,-28.387416697508));
#18081=CARTESIAN_POINT('',(22.5160872418661,49.9978763965905,-28.112583302492));
#18082=CARTESIAN_POINT('',(22.5175,50.,-32.));
#18083=CARTESIAN_POINT('Ctrl Pts',(22.5160872418661,49.9978763965905,-28.112583302492));
#18084=CARTESIAN_POINT('Ctrl Pts',(22.5112878705318,50.5868020213575,-28.0753961818803));
#18085=CARTESIAN_POINT('Ctrl Pts',(22.3047333820125,51.1787611658199,-28.0382090612686));
#18086=CARTESIAN_POINT('Ctrl Pts',(21.9270451822179,51.6262950900966,-28.0010219406569));
#18087=CARTESIAN_POINT('Ctrl Pts',(21.3923144080189,52.2599134079022,-27.9483724329261));
#18088=CARTESIAN_POINT('Ctrl Pts',(20.5145481122645,52.6040330619851,-27.8957229251952));
#18089=CARTESIAN_POINT('Ctrl Pts',(19.6916682954148,52.5026526660411,-27.8430734174644));
#18090=CARTESIAN_POINT('Ctrl Pts',(18.8687884785652,52.4012722700971,-27.7904239097336));
#18091=CARTESIAN_POINT('Ctrl Pts',(18.1007951406203,51.8543918241262,-27.7377744020028));
#18092=CARTESIAN_POINT('Ctrl Pts',(17.7358463859764,51.1099312104162,-27.685124894272));
#18093=CARTESIAN_POINT('Ctrl Pts',(17.3708976313326,50.3654705967061,-27.6324753865411));
#18094=CARTESIAN_POINT('Ctrl Pts',(17.4089934599897,49.4234298152568,-27.5798258788103));
#18095=CARTESIAN_POINT('Ctrl Pts',(17.8328637006338,48.7108688315972,-27.5271763710795));
#18096=CARTESIAN_POINT('Ctrl Pts',(18.2567339412778,47.9983078479377,-27.4745268633487));
#18097=CARTESIAN_POINT('Ctrl Pts',(19.0663785939088,47.5152266620678,-27.4218773556178));
#18098=CARTESIAN_POINT('Ctrl Pts',(19.8947575807264,47.4806225790254,-27.369227847887));
#18099=CARTESIAN_POINT('Ctrl Pts',(20.723136567544,47.446018495983,-27.3165783401562));
#18100=CARTESIAN_POINT('Ctrl Pts',(21.5702498885484,47.8598915157682,-27.2639288324254));
#18101=CARTESIAN_POINT('Ctrl Pts',(22.052071574967,48.5346190055783,-27.2112793246946));
#18102=CARTESIAN_POINT('Ctrl Pts',(22.3531436134977,48.9562305405835,-27.178380650627));
#18103=CARTESIAN_POINT('Ctrl Pts',(22.5115866359416,49.4796933442159,-27.1454819765595));
#18104=CARTESIAN_POINT('Ctrl Pts',(22.514511951768,50.001528002557,-27.112583302492));
#18105=CARTESIAN_POINT('Ctrl Pts',(22.5196059184078,50.0018577146135,-27.387416697508));
#18106=CARTESIAN_POINT('Ctrl Pts',(22.5137402304142,49.2935955420337,-27.432300020937));
#18107=CARTESIAN_POINT('Ctrl Pts',(22.2008545185939,48.5807930337343,-27.477183344366));
#18108=CARTESIAN_POINT('Ctrl Pts',(21.6717030769048,48.1122109708708,-27.522066667795));
#18109=CARTESIAN_POINT('Ctrl Pts',(21.0509922918832,47.5625499151274,-27.5747161755258));
#18110=CARTESIAN_POINT('Ctrl Pts',(20.1326997381625,47.3489363327836,-27.6273656832566));
#18111=CARTESIAN_POINT('Ctrl Pts',(19.3331193645885,47.5682087134236,-27.6800151909875));
#18112=CARTESIAN_POINT('Ctrl Pts',(18.5335389910145,47.7874810940636,-27.7326646987183));
#18113=CARTESIAN_POINT('Ctrl Pts',(17.8526707975874,48.4396394376874,-27.7853142064491));
#18114=CARTESIAN_POINT('Ctrl Pts',(17.5991760340398,49.2290376662104,-27.8379637141799));
#18115=CARTESIAN_POINT('Ctrl Pts',(17.3456812704923,50.0184358947333,-27.8906132219108));
#18116=CARTESIAN_POINT('Ctrl Pts',(17.5195599368243,50.9450740081554,-27.9432627296416));
#18117=CARTESIAN_POINT('Ctrl Pts',(18.041986779737,51.588874714119,-27.9959122373724));
#18118=CARTESIAN_POINT('Ctrl Pts',(18.5644136226497,52.2326754200825,-28.0485617451032));
#18119=CARTESIAN_POINT('Ctrl Pts',(19.4353886421431,52.5936387185874,-28.101211252834));
#18120=CARTESIAN_POINT('Ctrl Pts',(20.260068559922,52.5081273847708,-28.1538607605649));
#18121=CARTESIAN_POINT('Ctrl Pts',(21.0847484777008,52.4226160509542,-28.2065102682957));
#18122=CARTESIAN_POINT('Ctrl Pts',(21.8631332937651,51.8906300848161,-28.2591597760265));
#18123=CARTESIAN_POINT('Ctrl Pts',(22.2423540874804,51.1533372355938,-28.3118092837573));
#18124=CARTESIAN_POINT('Ctrl Pts',(22.423880972783,50.8004070252958,-28.3370117550076));
#18125=CARTESIAN_POINT('Ctrl Pts',(22.5139441053345,50.400433151388,-28.3622142262578));
#18126=CARTESIAN_POINT('Ctrl Pts',(22.5135351409985,50.0002853817648,-28.387416697508));
#18127=CARTESIAN_POINT('Origin',(20.,50.,-32.));
#18128=CARTESIAN_POINT('',(22.5185977288488,49.9978738300597,-29.387416697508));
#18129=CARTESIAN_POINT('',(22.5214168327014,50.00056091356,-29.112583302492));
#18130=CARTESIAN_POINT('',(22.5175,50.,-32.));
#18131=CARTESIAN_POINT('Ctrl Pts',(22.5214168327014,50.00056091356,-29.112583302492));
#18132=CARTESIAN_POINT('Ctrl Pts',(22.5215115546983,50.0316502586541,-29.1106094026627));
#18133=CARTESIAN_POINT('Ctrl Pts',(22.5209857633104,50.0627363262992,-29.1086355028334));
#18134=CARTESIAN_POINT('Ctrl Pts',(22.5198294794022,50.0937989242928,-29.1066616030042));
#18135=CARTESIAN_POINT('Ctrl Pts',(22.4889881075843,50.9223265268352,-29.0540120952734));
#18136=CARTESIAN_POINT('Ctrl Pts',(22.0095890011769,51.7341568754072,-29.0013625875425));
#18137=CARTESIAN_POINT('Ctrl Pts',(21.298960454951,52.1612590266266,-28.9487130798117));
#18138=CARTESIAN_POINT('Ctrl Pts',(20.588331908725,52.588361177846,-28.8960635720809));
#18139=CARTESIAN_POINT('Ctrl Pts',(19.6464739226806,52.6307351317128,-28.8434140643501));
#18140=CARTESIAN_POINT('Ctrl Pts',(18.9003634921058,52.2691713010304,-28.7907645566192));
#18141=CARTESIAN_POINT('Ctrl Pts',(18.1542530615311,51.9076074703479,-28.7381150488884));
#18142=CARTESIAN_POINT('Ctrl Pts',(17.603890186426,51.1421058551164,-28.6854655411576));
#18143=CARTESIAN_POINT('Ctrl Pts',(17.4987735070085,50.3196949709328,-28.6328160334268));
#18144=CARTESIAN_POINT('Ctrl Pts',(17.3936568275909,49.4972840867492,-28.5801665256959));
#18145=CARTESIAN_POINT('Ctrl Pts',(17.733786343861,48.6179639336134,-28.5275170179651));
#18146=CARTESIAN_POINT('Ctrl Pts',(18.3649695117957,48.0803609329424,-28.4748675102343));
#18147=CARTESIAN_POINT('Ctrl Pts',(18.9961526797304,47.5427579322714,-28.4222180025035));
#18148=CARTESIAN_POINT('Ctrl Pts',(19.9183894993297,47.3468720840651,-28.3695684947727));
#18149=CARTESIAN_POINT('Ctrl Pts',(20.7135979329253,47.5815052555246,-28.3169189870418));
#18150=CARTESIAN_POINT('Ctrl Pts',(21.5088063665209,47.816138426984,-28.264269479311));
#18151=CARTESIAN_POINT('Ctrl Pts',(22.1769864141127,48.4812906181093,-28.2116199715802));
#18152=CARTESIAN_POINT('Ctrl Pts',(22.4152288115867,49.275425204436,-28.1589704638494));
#18153=CARTESIAN_POINT('Ctrl Pts',(22.4851971044864,49.508650868411,-28.1435080767302));
#18154=CARTESIAN_POINT('Ctrl Pts',(22.5180828181915,49.7530014010348,-28.1280456896111));
#18155=CARTESIAN_POINT('Ctrl Pts',(22.5160872418661,49.9978763965905,-28.112583302492));
#18156=CARTESIAN_POINT('Ctrl Pts',(22.5135351409985,50.0002853817648,-28.387416697508));
#18157=CARTESIAN_POINT('Ctrl Pts',(22.513089753761,49.5644999255914,-28.4148637339886));
#18158=CARTESIAN_POINT('Ctrl Pts',(22.4053395245617,49.1285082196138,-28.4423107704692));
#18159=CARTESIAN_POINT('Ctrl Pts',(22.1915653615212,48.7528512927249,-28.4697578069498));
#18160=CARTESIAN_POINT('Ctrl Pts',(21.7814990704807,48.0322579313851,-28.5224073146806));
#18161=CARTESIAN_POINT('Ctrl Pts',(20.9813097170337,47.533670941012,-28.5750568224115));
#18162=CARTESIAN_POINT('Ctrl Pts',(20.1537509759774,47.4831171521003,-28.6277063301423));
#18163=CARTESIAN_POINT('Ctrl Pts',(19.3261922349211,47.4325633631885,-28.6803558378731));
#18164=CARTESIAN_POINT('Ctrl Pts',(18.4712641062555,47.8300427757381,-28.7330053456039));
#18165=CARTESIAN_POINT('Ctrl Pts',(17.9765352565092,48.4953641422999,-28.7856548533347));
#18166=CARTESIAN_POINT('Ctrl Pts',(17.4818064067629,49.1606855088617,-28.8383043610656));
#18167=CARTESIAN_POINT('Ctrl Pts',(17.3472768359358,50.0938488294357,-28.8909538687964));
#18168=CARTESIAN_POINT('Ctrl Pts',(17.6339334791313,50.8718187031622,-28.9436033765272));
#18169=CARTESIAN_POINT('Ctrl Pts',(17.9205901223267,51.6497885768887,-28.996252884258));
#18170=CARTESIAN_POINT('Ctrl Pts',(18.6284329795446,52.2725650037676,-29.0489023919889));
#18171=CARTESIAN_POINT('Ctrl Pts',(19.4365722555317,52.4578217610763,-29.1015518997197));
#18172=CARTESIAN_POINT('Ctrl Pts',(20.2447115315189,52.643078518385,-29.1542014074505));
#18173=CARTESIAN_POINT('Ctrl Pts',(21.1531472262752,52.3908156061234,-29.2068509151813));
#18174=CARTESIAN_POINT('Ctrl Pts',(21.7500538319779,51.8153925794714,-29.2595004229121));
#18175=CARTESIAN_POINT('Ctrl Pts',(22.2334649316189,51.3493801825317,-29.3021391811108));
#18176=CARTESIAN_POINT('Ctrl Pts',(22.5125521775403,50.671415443866,-29.3447779393094));
#18177=CARTESIAN_POINT('Ctrl Pts',(22.5185977288488,49.9978738300597,-29.387416697508));
#18178=CARTESIAN_POINT('Origin',(20.,50.,-32.));
#18179=CARTESIAN_POINT('',(22.5197498940917,50.0018038620106,-30.387416697508));
#18180=CARTESIAN_POINT('',(22.5146148548194,50.0015907043193,-30.112583302492));
#18181=CARTESIAN_POINT('',(22.5175,50.,-32.));
#18182=CARTESIAN_POINT('Ctrl Pts',(22.5146148548194,50.0015907043193,-30.112583302492));
#18183=CARTESIAN_POINT('Ctrl Pts',(22.5164165725427,50.3094409506913,-30.0931731157143));
#18184=CARTESIAN_POINT('Ctrl Pts',(22.4640313740575,50.6166994268775,-30.0737629289367));
#18185=CARTESIAN_POINT('Ctrl Pts',(22.3546757956077,50.9021312216285,-30.054352742159));
#18186=CARTESIAN_POINT('Ctrl Pts',(22.0580523040901,51.6763557902278,-30.0017032344282));
#18187=CARTESIAN_POINT('Ctrl Pts',(21.3422702745872,52.2899909457831,-29.9490537266973));
#18188=CARTESIAN_POINT('Ctrl Pts',(20.5318186054112,52.4648545219549,-29.8964042189665));
#18189=CARTESIAN_POINT('Ctrl Pts',(19.7213669362353,52.6397180981267,-29.8437547112357));
#18190=CARTESIAN_POINT('Ctrl Pts',(18.8162456273862,52.375810094915,-29.7911052035048));
#18191=CARTESIAN_POINT('Ctrl Pts',(18.2267776602203,51.792769192383,-29.738455695774));
#18192=CARTESIAN_POINT('Ctrl Pts',(17.6373096930544,51.209728289851,-29.6858061880432));
#18193=CARTESIAN_POINT('Ctrl Pts',(17.3634950675715,50.3075544879986,-29.6331566803124));
#18194=CARTESIAN_POINT('Ctrl Pts',(17.5294634803876,49.4952345606944,-29.5805071725816));
#18195=CARTESIAN_POINT('Ctrl Pts',(17.6954318932037,48.6829146333902,-29.5278576648508));
#18196=CARTESIAN_POINT('Ctrl Pts',(18.3011833443186,47.9604485806342,-29.4752081571199));
#18197=CARTESIAN_POINT('Ctrl Pts',(19.0721096249166,47.655355401064,-29.4225586493891));
#18198=CARTESIAN_POINT('Ctrl Pts',(19.8430359055145,47.3502622214937,-29.3699091416583));
#18199=CARTESIAN_POINT('Ctrl Pts',(20.7791370155955,47.4625419151092,-29.3172596339275));
#18200=CARTESIAN_POINT('Ctrl Pts',(21.4560457520219,47.9412941901733,-29.2646101261967));
#18201=CARTESIAN_POINT('Ctrl Pts',(22.1075762827091,48.4020974078818,-29.2139345182951));
#18202=CARTESIAN_POINT('Ctrl Pts',(22.518985050346,49.2024092350691,-29.1632589103935));
#18203=CARTESIAN_POINT('Ctrl Pts',(22.5214168327014,50.00056091356,-29.112583302492));
#18204=CARTESIAN_POINT('Ctrl Pts',(22.5185977288488,49.9978738300597,-29.387416697508));
#18205=CARTESIAN_POINT('Ctrl Pts',(22.5200171064876,49.8397393843069,-29.3974274470402));
#18206=CARTESIAN_POINT('Ctrl Pts',(22.5063859100399,49.6818487495533,-29.4074381965724));
#18207=CARTESIAN_POINT('Ctrl Pts',(22.4768148244427,49.5270021587398,-29.4174489461046));
#18208=CARTESIAN_POINT('Ctrl Pts',(22.3212916945558,48.7126179057026,-29.4700984538354));
#18209=CARTESIAN_POINT('Ctrl Pts',(21.7248679181332,47.9824325406707,-29.5227479615663));
#18210=CARTESIAN_POINT('Ctrl Pts',(20.9579231445072,47.6674644950945,-29.5753974692971));
#18211=CARTESIAN_POINT('Ctrl Pts',(20.1909783708812,47.3524964495183,-29.6280469770279));
#18212=CARTESIAN_POINT('Ctrl Pts',(19.2535126000518,47.4527457233978,-29.6806964847587));
#18213=CARTESIAN_POINT('Ctrl Pts',(18.5705116833604,47.922765832889,-29.7333459924896));
#18214=CARTESIAN_POINT('Ctrl Pts',(17.887510766669,48.3927859423803,-29.7859955002204));
#18215=CARTESIAN_POINT('Ctrl Pts',(17.4589747041155,49.2325768874833,-29.8386450079512));
#18216=CARTESIAN_POINT('Ctrl Pts',(17.4791738029899,50.0614322137804,-29.891294515682));
#18217=CARTESIAN_POINT('Ctrl Pts',(17.4993729018644,50.8902875400776,-29.9439440234128));
#18218=CARTESIAN_POINT('Ctrl Pts',(17.9683071621667,51.7082072475688,-29.9965935311437));
#18219=CARTESIAN_POINT('Ctrl Pts',(18.6733923679848,52.1443998748141,-30.0492430388745));
#18220=CARTESIAN_POINT('Ctrl Pts',(19.378477573803,52.5805925020594,-30.1018925466053));
#18221=CARTESIAN_POINT('Ctrl Pts',(20.3197137251369,52.6350580490587,-30.1545420543361));
#18222=CARTESIAN_POINT('Ctrl Pts',(21.0704057259808,52.2831053883275,-30.207191562067));
#18223=CARTESIAN_POINT('Ctrl Pts',(21.8210977268248,51.9311527275964,-30.2598410697978));
#18224=CARTESIAN_POINT('Ctrl Pts',(22.3812455771788,51.1727818591349,-30.3124905775286));
#18225=CARTESIAN_POINT('Ctrl Pts',(22.4969147671484,50.3517886837562,-30.3651400852594));
#18226=CARTESIAN_POINT('Ctrl Pts',(22.5132284220151,50.2359981321448,-30.3725656226756));
#18227=CARTESIAN_POINT('Ctrl Pts',(22.5207007373935,50.1189619300123,-30.3799911600918));
#18228=CARTESIAN_POINT('Ctrl Pts',(22.5197498940917,50.0018038620106,-30.387416697508));
#18229=CARTESIAN_POINT('Origin',(20.,50.,-32.));
#18230=CARTESIAN_POINT('',(22.5135563364326,50.0003713189448,-31.387416697508));
#18231=CARTESIAN_POINT('',(22.5159430076381,49.9979064240735,-31.112583302492));
#18232=CARTESIAN_POINT('',(22.5175,50.,-32.));
#18233=CARTESIAN_POINT('Ctrl Pts',(22.5159430076381,49.9979064240735,-31.112583302492));
#18234=CARTESIAN_POINT('Ctrl Pts',(22.5112750114203,50.5815220951261,-31.0757368287659));
#18235=CARTESIAN_POINT('Ctrl Pts',(22.3088213343573,51.1680598664448,-31.0388903550399));
#18236=CARTESIAN_POINT('Ctrl Pts',(21.9374478949046,51.6138880066437,-31.0020438813138));
#18237=CARTESIAN_POINT('Ctrl Pts',(21.406796606077,52.2509267715613,-30.949394373583));
#18238=CARTESIAN_POINT('Ctrl Pts',(20.5312579962154,52.6006754821119,-30.8967448658522));
#18239=CARTESIAN_POINT('Ctrl Pts',(19.7077441799491,52.5045808789307,-30.8440953581213));
#18240=CARTESIAN_POINT('Ctrl Pts',(18.8842303636827,52.4084862757494,-30.7914458503905));
#18241=CARTESIAN_POINT('Ctrl Pts',(18.1127413410116,51.8665483588361,-30.7387963426597));
#18242=CARTESIAN_POINT('Ctrl Pts',(17.7430199284747,51.1244464416753,-30.6861468349288));
#18243=CARTESIAN_POINT('Ctrl Pts',(17.3732985159378,50.3823445245144,-30.633497327198));
#18244=CARTESIAN_POINT('Ctrl Pts',(17.4053447135351,49.440078607106,-30.5808478194672));
#18245=CARTESIAN_POINT('Ctrl Pts',(17.8246308649064,48.7248106142456,-30.5281983117364));
#18246=CARTESIAN_POINT('Ctrl Pts',(18.2439170162777,48.0095426213853,-30.4755488040056));
#18247=CARTESIAN_POINT('Ctrl Pts',(19.050443121423,47.5212725530731,-30.4228992962748));
#18248=CARTESIAN_POINT('Ctrl Pts',(19.878582835266,47.4813502197473,-30.3702497885439));
#18249=CARTESIAN_POINT('Ctrl Pts',(20.7067225491089,47.4414278864215,-30.3176002808131));
#18250=CARTESIAN_POINT('Ctrl Pts',(21.5564758716496,47.8498532880821,-30.2649507730823));
#18251=CARTESIAN_POINT('Ctrl Pts',(22.0426200561537,48.521472979734,-30.2123012653514));
#18252=CARTESIAN_POINT('Ctrl Pts',(22.3495384543439,48.9454880076317,-30.1790619443983));
#18253=CARTESIAN_POINT('Ctrl Pts',(22.511529471131,49.4744070526688,-30.1458226234451));
#18254=CARTESIAN_POINT('Ctrl Pts',(22.5146148548194,50.0015907043193,-30.112583302492));
#18255=CARTESIAN_POINT('Ctrl Pts',(22.5197498940917,50.0018038620106,-30.387416697508));
#18256=CARTESIAN_POINT('Ctrl Pts',(22.5139589449867,49.2882726126943,-30.4326406678226));
#18257=CARTESIAN_POINT('Ctrl Pts',(22.1957352286107,48.5702211005946,-30.4778646381373));
#18258=CARTESIAN_POINT('Ctrl Pts',(21.6595471291725,48.1015158787921,-30.5230886084519));
#18259=CARTESIAN_POINT('Ctrl Pts',(21.0353197716417,47.5558517315029,-30.5757381161827));
#18260=CARTESIAN_POINT('Ctrl Pts',(20.1156745269951,47.3481389192203,-30.6283876239135));
#18261=CARTESIAN_POINT('Ctrl Pts',(19.3175185820202,47.5725408867429,-30.6810371316444));
#18262=CARTESIAN_POINT('Ctrl Pts',(18.5193626370453,47.7969428542654,-30.7336866393752));
#18263=CARTESIAN_POINT('Ctrl Pts',(17.8426959917422,48.4534596015932,-30.786336147106));
#18264=CARTESIAN_POINT('Ctrl Pts',(17.5942751798161,49.2444692448522,-30.8389856548368));
#18265=CARTESIAN_POINT('Ctrl Pts',(17.3458543678901,50.0354788881112,-30.8916351625677));
#18266=CARTESIAN_POINT('Ctrl Pts',(17.5256793893411,50.9609814273015,-30.9442846702985));
#18267=CARTESIAN_POINT('Ctrl Pts',(18.0522293052598,51.6014143602248,-30.9969341780293));
#18268=CARTESIAN_POINT('Ctrl Pts',(18.5787792211785,52.2418472931482,-31.0495836857601));
#18269=CARTESIAN_POINT('Ctrl Pts',(19.4520540315648,52.5972106198046,-31.102233193491));
#18270=CARTESIAN_POINT('Ctrl Pts',(20.2761678808566,52.5064057799978,-31.1548827012218));
#18271=CARTESIAN_POINT('Ctrl Pts',(21.1002817301483,52.415600940191,-31.2075322089526));
#18272=CARTESIAN_POINT('Ctrl Pts',(21.8752346183454,51.8786279339211,-31.2601817166834));
#18273=CARTESIAN_POINT('Ctrl Pts',(22.2497134381471,51.1389153079327,-31.3128312244142));
#18274=CARTESIAN_POINT('Ctrl Pts',(22.4265475064497,50.7896127943817,-31.3376930487788));
#18275=CARTESIAN_POINT('Ctrl Pts',(22.5140815132308,50.3951022088419,-31.3625548731434));
#18276=CARTESIAN_POINT('Ctrl Pts',(22.5135563364326,50.0003713189448,-31.387416697508));
#18277=CARTESIAN_POINT('Origin',(20.,50.,-32.));
#18278=CARTESIAN_POINT('',(22.518438676647,49.9978466804791,-32.387416697508));
#18279=CARTESIAN_POINT('',(22.5214653521749,50.000465985833,-32.112583302492));
#18280=CARTESIAN_POINT('',(22.5175,50.,-32.));
#18281=CARTESIAN_POINT('Ctrl Pts',(22.5214653521749,50.000465985833,-32.112583302492));
#18282=CARTESIAN_POINT('Ctrl Pts',(22.5215314384593,50.0261887418618,-32.1109500495483));
#18283=CARTESIAN_POINT('Ctrl Pts',(22.5211715019415,50.0519096037782,-32.1093167966047));
#18284=CARTESIAN_POINT('Ctrl Pts',(22.5203798163051,50.0776171696253,-32.1076835436611));
#18285=CARTESIAN_POINT('Ctrl Pts',(22.4948590546864,50.9063257245881,-32.0550340359302));
#18286=CARTESIAN_POINT('Ctrl Pts',(22.0206825923804,51.7212175581987,-32.0023845281994));
#18287=CARTESIAN_POINT('Ctrl Pts',(21.312811117861,52.1528738495971,-31.9497350204686));
#18288=CARTESIAN_POINT('Ctrl Pts',(20.6049396433416,52.5845301409955,-31.8970855127378));
#18289=CARTESIAN_POINT('Ctrl Pts',(19.6633731566088,52.6329508901818,-31.844436005007));
#18290=CARTESIAN_POINT('Ctrl Pts',(18.9149565061977,52.2761852868376,-31.7917864972761));
#18291=CARTESIAN_POINT('Ctrl Pts',(18.1665398557866,51.9194196834934,-31.7391369895453));
#18292=CARTESIAN_POINT('Ctrl Pts',(17.6112730416973,51.1574677276187,-31.6864874818145));
#18293=CARTESIAN_POINT('Ctrl Pts',(17.5008778302588,50.3357487515487,-31.6338379740837));
#18294=CARTESIAN_POINT('Ctrl Pts',(17.3904826188202,49.5140297754786,-31.5811884663529));
#18295=CARTESIAN_POINT('Ctrl Pts',(17.7249590100325,48.6325437792133,-31.528538958622));
#18296=CARTESIAN_POINT('Ctrl Pts',(18.3526772182592,48.0908990345672,-31.4758894508912));
#18297=CARTESIAN_POINT('Ctrl Pts',(18.980395426486,47.5492542899211,-31.4232399431604));
#18298=CARTESIAN_POINT('Ctrl Pts',(19.9013554517273,47.3474507968943,-31.3705904354295));
#18299=CARTESIAN_POINT('Ctrl Pts',(20.6980540714064,47.5769731002625,-31.3179409276987));
#18300=CARTESIAN_POINT('Ctrl Pts',(21.4947526910856,47.8064954036307,-31.2652914199679));
#18301=CARTESIAN_POINT('Ctrl Pts',(22.1671899052026,48.467343503394,-31.2126419122371));
#18302=CARTESIAN_POINT('Ctrl Pts',(22.4105265283643,49.2599319629178,-31.1599924045063));
#18303=CARTESIAN_POINT('Ctrl Pts',(22.4835653296022,49.4978316682992,-31.1441893705015));
#18304=CARTESIAN_POINT('Ctrl Pts',(22.5179450581875,49.7476002926395,-31.1283863364967));
#18305=CARTESIAN_POINT('Ctrl Pts',(22.5159430076381,49.9979064240735,-31.112583302492));
#18306=CARTESIAN_POINT('Ctrl Pts',(22.5135563364326,50.0003713189448,-31.387416697508));
#18307=CARTESIAN_POINT('Ctrl Pts',(22.5129693543042,49.5591866004592,-31.4152043808743));
#18308=CARTESIAN_POINT('Ctrl Pts',(22.4023771380614,49.1177266735126,-31.4429920642405));
#18309=CARTESIAN_POINT('Ctrl Pts',(22.1835122430109,48.7388049647084,-31.4707797476067));
#18310=CARTESIAN_POINT('Ctrl Pts',(21.7688274766669,48.0208594931794,-31.5234292553375));
#18311=CARTESIAN_POINT('Ctrl Pts',(20.9654531925725,47.5274207958285,-31.5760787630683));
#18312=CARTESIAN_POINT('Ctrl Pts',(20.1375869056597,47.4821818024699,-31.6287282707992));
#18313=CARTESIAN_POINT('Ctrl Pts',(19.309720618747,47.4369428091112,-31.68137777853));
#18314=CARTESIAN_POINT('Ctrl Pts',(18.457362329016,47.8399035197448,-31.7340272862608));
#18315=CARTESIAN_POINT('Ctrl Pts',(17.9669157054634,48.508387823953,-31.7866767939917));
#18316=CARTESIAN_POINT('Ctrl Pts',(17.4764690819109,49.1768721281611,-31.8393263017225));
#18317=CARTESIAN_POINT('Ctrl Pts',(17.3479341245368,50.1108800259438,-31.8919758094533));
#18318=CARTESIAN_POINT('Ctrl Pts',(17.6395802016597,50.8869932401243,-31.9446253171841));
#18319=CARTESIAN_POINT('Ctrl Pts',(17.9312262787826,51.6631064543048,-31.9972748249149));
#18320=CARTESIAN_POINT('Ctrl Pts',(18.6430533904026,52.2813249848831,-32.0499243326458));
#18321=CARTESIAN_POINT('Ctrl Pts',(19.4523655400881,52.4613888621549,-32.1025738403766));
#18322=CARTESIAN_POINT('Ctrl Pts',(20.2616776897736,52.6414527394267,-32.1552233481074));
#18323=CARTESIAN_POINT('Ctrl Pts',(21.1684748775248,52.3833619633919,-32.2078728558382));
#18324=CARTESIAN_POINT('Ctrl Pts',(21.7616743877694,51.8041180626279,-32.2605223635691));
#18325=CARTESIAN_POINT('Ctrl Pts',(22.2382452047924,51.3387590488808,-32.302820474882));
#18326=CARTESIAN_POINT('Ctrl Pts',(22.5124087275473,50.6661161816974,-32.345118586195));
#18327=CARTESIAN_POINT('Ctrl Pts',(22.518438676647,49.9978466804791,-32.387416697508));
#18328=CARTESIAN_POINT('Origin',(20.,50.,-32.));
#18329=CARTESIAN_POINT('',(22.519890696217,50.0017467019843,-33.387416697508));
#18330=CARTESIAN_POINT('',(22.5147220745132,50.001651275808,-33.112583302492));
#18331=CARTESIAN_POINT('',(22.5175,50.,-32.));
#18332=CARTESIAN_POINT('Ctrl Pts',(22.5147220745132,50.001651275808,-33.112583302492));
#18333=CARTESIAN_POINT('Ctrl Pts',(22.5165646035554,50.3040663516863,-33.0935137626));
#18334=CARTESIAN_POINT('Ctrl Pts',(22.4660534290505,50.6058866921801,-33.0744442227079));
#18335=CARTESIAN_POINT('Ctrl Pts',(22.3604198375119,50.8869932548441,-33.0553746828159));
#18336=CARTESIAN_POINT('Ctrl Pts',(22.0687737555491,51.6631064819043,-33.0027251750851));
#18337=CARTESIAN_POINT('Ctrl Pts',(21.3569466321163,52.2813250227421,-32.9500756673542));
#18338=CARTESIAN_POINT('Ctrl Pts',(20.5476344690001,52.4613889030021,-32.8974261596234));
#18339=CARTESIAN_POINT('Ctrl Pts',(19.7383223058839,52.6414527832621,-32.8447766518926));
#18340=CARTESIAN_POINT('Ctrl Pts',(18.8315251030843,52.3833620029443,-32.7921271441618));
#18341=CARTESIAN_POINT('Ctrl Pts',(18.2383255829953,51.8041180925676,-32.739477636431));
#18342=CARTESIAN_POINT('Ctrl Pts',(17.6451260629064,51.224874182191,-32.6868281287001));
#18343=CARTESIAN_POINT('Ctrl Pts',(17.3655242255282,50.3244771417555,-32.6341786209693));
#18344=CARTESIAN_POINT('Ctrl Pts',(17.5262733119833,49.5111082773736,-32.5815291132385));
#18345=CARTESIAN_POINT('Ctrl Pts',(17.6870223984385,48.6977394129917,-32.5288796055077));
#18346=CARTESIAN_POINT('Ctrl Pts',(18.2881224087269,47.9713987246632,-32.4762300977768));
#18347=CARTESIAN_POINT('Ctrl Pts',(19.0570737939997,47.6613617181153,-32.423580590046));
#18348=CARTESIAN_POINT('Ctrl Pts',(19.8260251792725,47.3513247115674,-32.3709310823152));
#18349=CARTESIAN_POINT('Ctrl Pts',(20.7628279395296,47.4575913867999,-32.3182815745844));
#18350=CARTESIAN_POINT('Ctrl Pts',(21.4427967891924,47.9319873625737,-32.2656320668535));
#18351=CARTESIAN_POINT('Ctrl Pts',(22.1016721629015,48.3916669875728,-32.2146158120664));
#18352=CARTESIAN_POINT('Ctrl Pts',(22.5194010823779,49.1969905165226,-32.1635995572792));
#18353=CARTESIAN_POINT('Ctrl Pts',(22.5214653521749,50.000465985833,-32.112583302492));
#18354=CARTESIAN_POINT('Ctrl Pts',(22.518438676647,49.9978466804791,-32.387416697508));
#18355=CARTESIAN_POINT('Ctrl Pts',(22.5199143546754,49.8343045669821,-32.3977680939259));
#18356=CARTESIAN_POINT('Ctrl Pts',(22.5053314531976,49.6710243753477,-32.4081194903437));
#18357=CARTESIAN_POINT('Ctrl Pts',(22.4737266469647,49.5111082854868,-32.4184708867615));
#18358=CARTESIAN_POINT('Ctrl Pts',(22.3129775631772,48.6977394346029,-32.4711203944923));
#18359=CARTESIAN_POINT('Ctrl Pts',(21.7118775628641,47.9713987583282,-32.5237699022232));
#18360=CARTESIAN_POINT('Ctrl Pts',(20.9429261903522,47.6613617569254,-32.576419409954));
#18361=CARTESIAN_POINT('Ctrl Pts',(20.1739748178403,47.3513247555226,-32.6290689176848));
#18362=CARTESIAN_POINT('Ctrl Pts',(19.2371720731297,47.4575914289917,-32.6817184254156));
#18363=CARTESIAN_POINT('Ctrl Pts',(18.5572032347511,47.9319873968928,-32.7343679331465));
#18364=CARTESIAN_POINT('Ctrl Pts',(17.8772343963725,48.4063833647939,-32.7870174408773));
#18365=CARTESIAN_POINT('Ctrl Pts',(17.4540994643259,49.2489086271271,-32.8396669486081));
#18366=CARTESIAN_POINT('Ctrl Pts',(17.4796202255211,50.0776171683373,-32.8923164563389));
#18367=CARTESIAN_POINT('Ctrl Pts',(17.5051409867163,50.9063257095475,-32.9449659640698));
#18368=CARTESIAN_POINT('Ctrl Pts',(17.9793174411532,51.7212175296348,-32.9976154718006));
#18369=CARTESIAN_POINT('Ctrl Pts',(18.6871889039254,52.1528738138698,-33.0502649795314));
#18370=CARTESIAN_POINT('Ctrl Pts',(19.3950603666975,52.5845300981048,-33.1029144872622));
#18371=CARTESIAN_POINT('Ctrl Pts',(20.3366268378049,52.6329508464875,-33.155563994993));
#18372=CARTESIAN_POINT('Ctrl Pts',(21.0850434757959,52.2761852490638,-33.2082135027239));
#18373=CARTESIAN_POINT('Ctrl Pts',(21.8334601137868,51.9194196516402,-33.2608630104547));
#18374=CARTESIAN_POINT('Ctrl Pts',(22.3887269186614,51.1574677084102,-33.3135125181855));
#18375=CARTESIAN_POINT('Ctrl Pts',(22.4991221282679,50.3357487459767,-33.3661620259163));
#18376=CARTESIAN_POINT('Ctrl Pts',(22.5139776892953,50.2251724244374,-33.3732469164469));
#18377=CARTESIAN_POINT('Ctrl Pts',(22.5207773824235,50.1135138238392,-33.3803318069775));
#18378=CARTESIAN_POINT('Ctrl Pts',(22.519890696217,50.0017467019843,-33.387416697508));
#18379=CARTESIAN_POINT('Origin',(20.,50.,-32.));
#18380=CARTESIAN_POINT('',(22.5135830750733,50.000456715329,-34.387416697508));
#18381=CARTESIAN_POINT('',(22.5158014821082,49.9979396994526,-34.112583302492));
#18382=CARTESIAN_POINT('',(22.5175,50.,-32.));
#18383=CARTESIAN_POINT('Ctrl Pts',(22.5158014821082,49.9979396994526,-34.112583302492));
#18384=CARTESIAN_POINT('Ctrl Pts',(22.5112690113793,50.5762422161602,-34.0760774756516));
#18385=CARTESIAN_POINT('Ctrl Pts',(22.3128670252218,51.1573545057524,-34.0395716488111));
#18386=CARTESIAN_POINT('Ctrl Pts',(21.9477707270638,51.6014143868006,-34.0030658219707));
#18387=CARTESIAN_POINT('Ctrl Pts',(21.421220802407,52.241847330352,-33.9504163142399));
#18388=CARTESIAN_POINT('Ctrl Pts',(20.5479459775285,52.5972106629057,-33.897766806509));
#18389=CARTESIAN_POINT('Ctrl Pts',(19.7238321145605,52.506405821592,-33.8451172987782));
#18390=CARTESIAN_POINT('Ctrl Pts',(18.8997182515924,52.4156009802783,-33.7924677910474));
#18391=CARTESIAN_POINT('Ctrl Pts',(18.1247653505348,51.8786279650973,-33.7398182833166));
#18392=CARTESIAN_POINT('Ctrl Pts',(17.7502865245185,51.1389153268333,-33.6871687755857));
#18393=CARTESIAN_POINT('Ctrl Pts',(17.3758076985023,50.3992026885692,-33.6345192678549));
#18394=CARTESIAN_POINT('Ctrl Pts',(17.4018029475274,49.456750427222,-33.5818697601241));
#18395=CARTESIAN_POINT('Ctrl Pts',(17.8164877207532,48.7388049437786,-33.5292202523933));
#18396=CARTESIAN_POINT('Ctrl Pts',(18.2311724939791,48.0208594603352,-33.4765707446625));
#18397=CARTESIAN_POINT('Ctrl Pts',(19.0345467914056,47.5274207547956,-33.4239212369316));
#18398=CARTESIAN_POINT('Ctrl Pts',(19.8624130920569,47.4821817606862,-33.3712717292008));
#18399=CARTESIAN_POINT('Ctrl Pts',(20.6902793927082,47.4369427665768,-33.31862222147));
#18400=CARTESIAN_POINT('Ctrl Pts',(21.5426376965843,47.8399034838976,-33.2659727137392));
#18401=CARTESIAN_POINT('Ctrl Pts',(22.0330843282759,48.5083877991994,-33.2133232060084));
#18402=CARTESIAN_POINT('Ctrl Pts',(22.345892231496,48.9347485151121,-33.1797432381696));
#18403=CARTESIAN_POINT('Ctrl Pts',(22.5114775250207,49.4691219867189,-33.1461632703308));
#18404=CARTESIAN_POINT('Ctrl Pts',(22.5147220745132,50.001651275808,-33.112583302492));
#18405=CARTESIAN_POINT('Ctrl Pts',(22.519890696217,50.0017467019843,-33.387416697508));
#18406=CARTESIAN_POINT('Ctrl Pts',(22.5141882061925,49.2829457408508,-33.4329813147083));
#18407=CARTESIAN_POINT('Ctrl Pts',(22.1905707471301,48.5596562513103,-33.4785459319085));
#18408=CARTESIAN_POINT('Ctrl Pts',(21.6473227544031,48.0908990662491,-33.5241105491088));
#18409=CARTESIAN_POINT('Ctrl Pts',(21.0196045565934,47.5492543305917,-33.5767600568396));
#18410=CARTESIAN_POINT('Ctrl Pts',(20.0986445466357,47.3474508409138,-33.6294095645704));
#18411=CARTESIAN_POINT('Ctrl Pts',(19.3019459401779,47.5769731404731,-33.6820590723013));
#18412=CARTESIAN_POINT('Ctrl Pts',(18.5052473337201,47.8064954400324,-33.7347085800321));
#18413=CARTESIAN_POINT('Ctrl Pts',(17.8328101307623,48.4673435288288,-33.7873580877629));
#18414=CARTESIAN_POINT('Ctrl Pts',(17.5894735116388,49.2599319751995,-33.8400075954937));
#18415=CARTESIAN_POINT('Ctrl Pts',(17.3461368925154,50.0525204215702,-33.8926571032246));
#18416=CARTESIAN_POINT('Ctrl Pts',(17.5319008572263,50.9768492255152,-33.9453066109554));
#18417=CARTESIAN_POINT('Ctrl Pts',(18.0625521372478,51.613887979861,-33.9979561186862));
#18418=CARTESIAN_POINT('Ctrl Pts',(18.5932034172692,52.2509267342067,-34.050605626417));
#18419=CARTESIAN_POINT('Ctrl Pts',(19.468742012601,52.6006754389532,-34.1032551341478));
#18420=CARTESIAN_POINT('Ctrl Pts',(20.292255815201,52.5045808373667,-34.1559046418787));
#18421=CARTESIAN_POINT('Ctrl Pts',(21.115769617801,52.4084862357801,-34.2085541496095));
#18422=CARTESIAN_POINT('Ctrl Pts',(21.8872586276691,51.8665483278603,-34.2612036573403));
#18423=CARTESIAN_POINT('Ctrl Pts',(22.2569800340703,51.1244464230148,-34.3138531650711));
#18424=CARTESIAN_POINT('Ctrl Pts',(22.4291754564946,50.7788171227519,-34.3383743425501));
#18425=CARTESIAN_POINT('Ctrl Pts',(22.5142205709798,50.3897688065706,-34.3628955200291));
#18426=CARTESIAN_POINT('Ctrl Pts',(22.5135830750733,50.000456715329,-34.387416697508));
#18427=CARTESIAN_POINT('Origin',(20.,50.,-32.));
#18428=CARTESIAN_POINT('',(22.5182787891679,49.9978231920092,-35.387416697508));
#18429=CARTESIAN_POINT('',(22.5215054096331,50.0003700141344,-35.112583302492));
#18430=CARTESIAN_POINT('',(22.5175,50.,-32.));
#18431=CARTESIAN_POINT('Ctrl Pts',(22.5215054096331,50.0003700141344,-35.112583302492));
#18432=CARTESIAN_POINT('Ctrl Pts',(22.5215475819598,50.0207269166612,-35.111290696434));
#18433=CARTESIAN_POINT('Ctrl Pts',(22.5213221499952,50.0410828615022,-35.109998090376));
#18434=CARTESIAN_POINT('Ctrl Pts',(22.5208262388437,50.0614322147998,-35.108705484318));
#18435=CARTESIAN_POINT('Ctrl Pts',(22.500627139634,50.890287554852,-35.0560559765872));
#18436=CARTESIAN_POINT('Ctrl Pts',(22.0316928715497,51.7082072759168,-35.0034064688563));
#18437=CARTESIAN_POINT('Ctrl Pts',(21.3266076540305,52.1443999104008,-34.9507569611255));
#18438=CARTESIAN_POINT('Ctrl Pts',(20.6215224365114,52.5805925448848,-34.8981074533947));
#18439=CARTESIAN_POINT('Ctrl Pts',(19.6802862695575,52.635058092788,-34.8454579456639));
#18440=CARTESIAN_POINT('Ctrl Pts',(18.9295942562556,52.2831054262161,-34.792808437933));
#18441=CARTESIAN_POINT('Ctrl Pts',(18.1789022429538,51.9311527596443,-34.7401589302022));
#18442=CARTESIAN_POINT('Ctrl Pts',(17.618754383304,51.1727818785975,-34.6875094224714));
#18443=CARTESIAN_POINT('Ctrl Pts',(17.5030851914148,50.3517886895942,-34.6348599147406));
#18444=CARTESIAN_POINT('Ctrl Pts',(17.3874159995256,49.5307955005909,-34.5822104070097));
#18445=CARTESIAN_POINT('Ctrl Pts',(17.7162254753971,48.6471800036312,-34.5295608992789));
#18446=CARTESIAN_POINT('Ctrl Pts',(18.340452843287,48.1015158472865,-34.4769113915481));
#18447=CARTESIAN_POINT('Ctrl Pts',(18.9646802111769,47.5558516909418,-34.4242618838173));
#18448=CARTESIAN_POINT('Ctrl Pts',(19.8843254710852,47.3481388752122,-34.3716123760865));
#18449=CARTESIAN_POINT('Ctrl Pts',(20.6824814293057,47.5725408464587,-34.3189628683556));
#18450=CARTESIAN_POINT('Ctrl Pts',(21.4806373875261,47.7969428177052,-34.2663133606248));
#18451=CARTESIAN_POINT('Ctrl Pts',(22.1573040440586,48.4534595759279,-34.213663852894));
#18452=CARTESIAN_POINT('Ctrl Pts',(22.4057248601073,49.2444692323139,-34.1610143451632));
#18453=CARTESIAN_POINT('Ctrl Pts',(22.4818970135361,49.4870129525554,-34.1448706642728));
#18454=CARTESIAN_POINT('Ctrl Pts',(22.5178058405196,49.7422015859551,-34.1287269833824));
#18455=CARTESIAN_POINT('Ctrl Pts',(22.5158014821082,49.9979396994526,-34.112583302492));
#18456=CARTESIAN_POINT('Ctrl Pts',(22.5135830750733,50.000456715329,-34.387416697508));
#18457=CARTESIAN_POINT('Ctrl Pts',(22.5128518012425,49.5538754252223,-34.4155450277599));
#18458=CARTESIAN_POINT('Ctrl Pts',(22.3993753556208,49.1069470475986,-34.4436733580117));
#18459=CARTESIAN_POINT('Ctrl Pts',(22.1753690989929,48.7248106354076,-34.4718016882636));
#18460=CARTESIAN_POINT('Ctrl Pts',(21.7560829545797,48.0095426544173,-34.5244511959944));
#18461=CARTESIAN_POINT('Ctrl Pts',(20.9495568628189,47.521272594208,-34.5771007037253));
#18462=CARTESIAN_POINT('Ctrl Pts',(20.121417162719,47.4813502615447,-34.6297502114561));
#18463=CARTESIAN_POINT('Ctrl Pts',(19.2932774626192,47.4414279288815,-34.6823997191869));
#18464=CARTESIAN_POINT('Ctrl Pts',(18.4435241541804,47.8498533237643,-34.7350492269177));
#18465=CARTESIAN_POINT('Ctrl Pts',(17.9573799777439,48.5214730042706,-34.7876987346485));
#18466=CARTESIAN_POINT('Ctrl Pts',(17.4712358013075,49.1930926847769,-34.8403482423793));
#18467=CARTESIAN_POINT('Ctrl Pts',(17.3487007568734,50.1279066509067,-34.8929977501102));
#18468=CARTESIAN_POINT('Ctrl Pts',(17.6453242434686,50.9021312066576,-34.945647257841));
#18469=CARTESIAN_POINT('Ctrl Pts',(17.9419477300637,51.6763557624084,-34.9982967655718));
#18470=CARTESIAN_POINT('Ctrl Pts',(18.6577297476881,52.2899909077803,-35.0509462733026));
#18471=CARTESIAN_POINT('Ctrl Pts',(19.4681814034145,52.4648544810502,-35.1035957810335));
#18472=CARTESIAN_POINT('Ctrl Pts',(20.2786330591408,52.6397180543201,-35.1562452887643));
#18473=CARTESIAN_POINT('Ctrl Pts',(21.1837543529692,52.375810055488,-35.2088947964951));
#18474=CARTESIAN_POINT('Ctrl Pts',(21.7732223103528,51.7927691626316,-35.261544304226));
#18475=CARTESIAN_POINT('Ctrl Pts',(22.2429813246144,51.3281320069191,-35.3035017686533));
#18476=CARTESIAN_POINT('Ctrl Pts',(22.5122745698353,50.6608192775936,-35.3454592330807));
#18477=CARTESIAN_POINT('Ctrl Pts',(22.5182787891679,49.9978231920092,-35.387416697508));
#18478=CARTESIAN_POINT('Origin',(20.,50.,-32.));
#18479=CARTESIAN_POINT('',(22.5200280234191,50.0016863229039,-36.387416697508));
#18480=CARTESIAN_POINT('',(22.5148335005971,50.0017093727271,-36.112583302492));
#18481=CARTESIAN_POINT('',(22.5175,50.,-32.));
#18482=CARTESIAN_POINT('Ctrl Pts',(22.5148335005971,50.0017093727271,-36.112583302492));
#18483=CARTESIAN_POINT('Ctrl Pts',(22.5167121752117,50.29868917153,-36.0938544094856));
#18484=CARTESIAN_POINT('Ctrl Pts',(22.4680382958723,50.5950732095141,-36.0751255164792));
#18485=CARTESIAN_POINT('Ctrl Pts',(22.3660665601341,50.8718187176302,-36.0563966234728));
#18486=CARTESIAN_POINT('Ctrl Pts',(22.0794099121816,51.6497886042672,-36.0037471157419));
#18487=CARTESIAN_POINT('Ctrl Pts',(21.3715670432168,52.2725650414812,-35.9510976080111));
#18488=CARTESIAN_POINT('Ctrl Pts',(20.5634277538184,52.4578218018643,-35.8984481002803));
#18489=CARTESIAN_POINT('Ctrl Pts',(19.7552884644201,52.6430785622474,-35.8457985925495));
#18490=CARTESIAN_POINT('Ctrl Pts',(18.8468527545881,52.3908156457995,-35.7931490848187));
#18491=CARTESIAN_POINT('Ctrl Pts',(18.2499461389797,51.8153926095982,-35.7404995770879));
#18492=CARTESIAN_POINT('Ctrl Pts',(17.6530395233712,51.239969573397,-35.687850069357));
#18493=CARTESIAN_POINT('Ctrl Pts',(17.3676620019863,50.3413864174424,-35.6352005616262));
#18494=CARTESIAN_POINT('Ctrl Pts',(17.5231851344541,49.5270021508903,-35.5825510538954));
#18495=CARTESIAN_POINT('Ctrl Pts',(17.6787082669219,48.7126178843383,-35.5299015461645));
#18496=CARTESIAN_POINT('Ctrl Pts',(18.2751320532423,47.9824325071888,-35.4772520384337));
#18497=CARTESIAN_POINT('Ctrl Pts',(19.0420768395959,47.6674644563856,-35.4246025307029));
#18498=CARTESIAN_POINT('Ctrl Pts',(19.8090216259494,47.3524964055824,-35.3719530229721));
#18499=CARTESIAN_POINT('Ctrl Pts',(20.7464874123362,47.4527456811256,-35.3193035152413));
#18500=CARTESIAN_POINT('Ctrl Pts',(21.4294883403622,47.9227657984169,-35.2666540075104));
#18501=CARTESIAN_POINT('Ctrl Pts',(22.0957208089051,48.3812463804461,-35.2152971058376));
#18502=CARTESIAN_POINT('Ctrl Pts',(22.5198298488346,49.1915640867918,-35.1639402041648));
#18503=CARTESIAN_POINT('Ctrl Pts',(22.5215054096331,50.0003700141344,-35.112583302492));
#18504=CARTESIAN_POINT('Ctrl Pts',(22.5182787891679,49.9978231920092,-35.387416697508));
#18505=CARTESIAN_POINT('Ctrl Pts',(22.5198088476208,49.8288715417166,-35.3981087408115));
#18506=CARTESIAN_POINT('Ctrl Pts',(22.5042412842967,49.6602002082423,-35.408800784115));
#18507=CARTESIAN_POINT('Ctrl Pts',(22.4705364786134,49.495234569071,-35.4194928274184));
#18508=CARTESIAN_POINT('Ctrl Pts',(22.3045680685516,48.6829146552474,-35.4721423351492));
#18509=CARTESIAN_POINT('Ctrl Pts',(21.6988166274892,47.9604486144809,-35.5247918428801));
#18510=CARTESIAN_POINT('Ctrl Pts',(20.9278903596849,47.6553554399738,-35.5774413506109));
#18511=CARTESIAN_POINT('Ctrl Pts',(20.1569640918805,47.3502622654666,-35.6300908583417));
#18512=CARTESIAN_POINT('Ctrl Pts',(19.2208629973343,47.4625419572188,-35.6827403660725));
#18513=CARTESIAN_POINT('Ctrl Pts',(18.5439542721414,47.941294224338,-35.7353898738034));
#18514=CARTESIAN_POINT('Ctrl Pts',(17.8670455469485,48.4200464914572,-35.7880393815342));
#18515=CARTESIAN_POINT('Ctrl Pts',(17.4493291911088,49.2652713339433,-35.840688889265));
#18516=CARTESIAN_POINT('Ctrl Pts',(17.4801705624149,50.0937989227362,-35.8933383969958));
#18517=CARTESIAN_POINT('Ctrl Pts',(17.5110119337209,50.9223265115291,-35.9459879047267));
#18518=CARTESIAN_POINT('Ctrl Pts',(17.9904110321727,51.7341568466287,-35.9986374124574));
#18519=CARTESIAN_POINT('Ctrl Pts',(18.7010395666056,52.1612589907602,-36.0512869201883));
#18520=CARTESIAN_POINT('Ctrl Pts',(19.4116681010385,52.5883611348917,-36.1039364279191));
#18521=CARTESIAN_POINT('Ctrl Pts',(20.3535260714527,52.630735088055,-36.15658593565));
#18522=CARTESIAN_POINT('Ctrl Pts',(21.0996364896456,52.2691712633729,-36.2092354433808));
#18523=CARTESIAN_POINT('Ctrl Pts',(21.8457469078385,51.9076074386908,-36.2618849511116));
#18524=CARTESIAN_POINT('Ctrl Pts',(22.3961097738102,51.1421058361633,-36.3145344588424));
#18525=CARTESIAN_POINT('Ctrl Pts',(22.5012264514832,50.3196949656275,-36.3671839665732));
#18526=CARTESIAN_POINT('Ctrl Pts',(22.5146915818506,50.2143466057627,-36.3739282102181));
#18527=CARTESIAN_POINT('Ctrl Pts',(22.5208507388777,50.1080644308405,-36.3806724538631));
#18528=CARTESIAN_POINT('Ctrl Pts',(22.5200280234191,50.0016863229039,-36.387416697508));
#18529=CARTESIAN_POINT('Origin',(20.,50.,-32.));
#18530=CARTESIAN_POINT('',(22.5136153256948,50.0005414263439,-37.387416697508));
#18531=CARTESIAN_POINT('',(22.5156628463169,49.9979761585217,-37.112583302492));
#18532=CARTESIAN_POINT('',(22.5175,50.,-32.));
#18533=CARTESIAN_POINT('Ctrl Pts',(22.5156628463169,49.9979761585217,-37.112583302492));
#18534=CARTESIAN_POINT('Ctrl Pts',(22.5112697173306,50.5709622635485,-37.0764181225372));
#18535=CARTESIAN_POINT('Ctrl Pts',(22.3168705700426,51.146645177931,-37.0402529425824));
#18536=CARTESIAN_POINT('Ctrl Pts',(21.958013252757,51.5888747404873,-37.0040877626276));
#18537=CARTESIAN_POINT('Ctrl Pts',(21.4355864011749,52.2326754571354,-36.9514382548968));
#18538=CARTESIAN_POINT('Ctrl Pts',(20.5646113672267,52.5936387616293,-36.898788747166));
#18539=CARTESIAN_POINT('Ctrl Pts',(19.739931435762,52.5081274263933,-36.8461392394351));
#18540=CARTESIAN_POINT('Ctrl Pts',(18.9152515042972,52.4226160911573,-36.7934897317043));
#18541=CARTESIAN_POINT('Ctrl Pts',(18.1368666753158,51.8906301161915,-36.7408402239735));
#18542=CARTESIAN_POINT('Ctrl Pts',(17.7576458753074,51.1533372547338,-36.6881907162427));
#18543=CARTESIAN_POINT('Ctrl Pts',(17.3784250752991,50.4160443932761,-36.6355412085118));
#18544=CARTESIAN_POINT('Ctrl Pts',(17.3983683042637,49.4734446453265,-36.582891700781));
#18545=CARTESIAN_POINT('Ctrl Pts',(17.8084346021093,48.7528512720282,-36.5302421930502));
#18546=CARTESIAN_POINT('Ctrl Pts',(18.2185008999548,48.0322578987299,-36.4775926853194));
#18547=CARTESIAN_POINT('Ctrl Pts',(19.0186902666813,47.5336709000828,-36.4249431775885));
#18548=CARTESIAN_POINT('Ctrl Pts',(19.8462490214711,47.4831171103322,-36.3722936698577));
#18549=CARTESIAN_POINT('Ctrl Pts',(20.6738077762609,47.4325633205815,-36.3196441621269));
#18550=CARTESIAN_POINT('Ctrl Pts',(21.5287359191141,47.8300427397272,-36.2669946543961));
#18551=CARTESIAN_POINT('Ctrl Pts',(22.0234647770705,48.4953641173301,-36.2143451466653));
#18552=CARTESIAN_POINT('Ctrl Pts',(22.3422048319556,48.9240121919327,-36.1804245319408));
#18553=CARTESIAN_POINT('Ctrl Pts',(22.511430961121,49.4638378961434,-36.1465039172164));
#18554=CARTESIAN_POINT('Ctrl Pts',(22.5148335005971,50.0017093727271,-36.112583302492));
#18555=CARTESIAN_POINT('Ctrl Pts',(22.5200280234191,50.0016863229039,-36.387416697508));
#18556=CARTESIAN_POINT('Ctrl Pts',(22.5144281411516,49.2776147449956,-36.4333219615939));
#18557=CARTESIAN_POINT('Ctrl Pts',(22.1853609537679,48.5490986296555,-36.4792272256798));
#18558=CARTESIAN_POINT('Ctrl Pts',(21.6350304610706,48.0803609647987,-36.5251324897657));
#18559=CARTESIAN_POINT('Ctrl Pts',(21.0038473036104,47.5427579730497,-36.5777819974966));
#18560=CARTESIAN_POINT('Ctrl Pts',(20.0816104993157,47.3468721280956,-36.6304315052273));
#18561=CARTESIAN_POINT('Ctrl Pts',(19.2864020789169,47.5815052956607,-36.6830810129581));
#18562=CARTESIAN_POINT('Ctrl Pts',(18.491193658518,47.8161384632257,-36.735730520689));
#18563=CARTESIAN_POINT('Ctrl Pts',(17.823013622015,48.4812906433099,-36.7883800284198));
#18564=CARTESIAN_POINT('Ctrl Pts',(17.5847712284946,49.2754252164592,-36.8410295361507));
#18565=CARTESIAN_POINT('Ctrl Pts',(17.3465288349741,50.0695597896084,-36.8936790438815));
#18566=CARTESIAN_POINT('Ctrl Pts',(17.5382240844361,50.9926767558226,-36.9463285516123));
#18567=CARTESIAN_POINT('Ctrl Pts',(18.0729548497615,51.6262950631108,-36.9989780593431));
#18568=CARTESIAN_POINT('Ctrl Pts',(18.607685615087,52.2599133703989,-37.0516275670739));
#18569=CARTESIAN_POINT('Ctrl Pts',(19.4854518962758,52.604033018761,-37.1042770748047));
#18570=CARTESIAN_POINT('Ctrl Pts',(20.308331699469,52.5026526245038,-37.1569265825356));
#18571=CARTESIAN_POINT('Ctrl Pts',(21.1312115026622,52.4012722302467,-37.2095760902664));
#18572=CARTESIAN_POINT('Ctrl Pts',(21.8992048278599,51.8543917933704,-37.2622255979972));
#18573=CARTESIAN_POINT('Ctrl Pts',(22.2641535764485,51.1099311920064,-37.314875105728));
#18574=CARTESIAN_POINT('Ctrl Pts',(22.4317649133932,50.7680200683765,-37.3390556363214));
#18575=CARTESIAN_POINT('Ctrl Pts',(22.5143611435832,50.3844329124877,-37.3632361669147));
#18576=CARTESIAN_POINT('Ctrl Pts',(22.5136153256948,50.0005414263439,-37.387416697508));
#18577=CARTESIAN_POINT('Origin',(20.,50.,-32.));
#18578=CARTESIAN_POINT('',(22.51811817366,49.9978011072146,-38.387416697508));
#18579=CARTESIAN_POINT('',(22.5215367446411,50.0002732851607,-38.112583302492));
#18580=CARTESIAN_POINT('',(22.5175,50.,-32.));
#18581=CARTESIAN_POINT('Ctrl Pts',(22.5215367446411,50.0002732851607,-38.112583302492));
#18582=CARTESIAN_POINT('Ctrl Pts',(22.5215600436793,50.0152649335192,-38.1116313433196));
#18583=CARTESIAN_POINT('Ctrl Pts',(22.5214377828025,50.0302561917135,-38.1106793841472));
#18584=CARTESIAN_POINT('Ctrl Pts',(22.5211687992195,50.0452448167457,-38.1097274249749));
#18585=CARTESIAN_POINT('Ctrl Pts',(22.5062922649704,50.8742128569845,-38.057077917244));
#18586=CARTESIAN_POINT('Ctrl Pts',(22.0426193843105,51.6951265643069,-38.0044284095132));
#18587=CARTESIAN_POINT('Ctrl Pts',(21.3403494591696,52.1358375133504,-37.9517789017824));
#18588=CARTESIAN_POINT('Ctrl Pts',(20.6380795340287,52.5765484623939,-37.8991293940516));
#18589=CARTESIAN_POINT('Ctrl Pts',(19.6972125644067,52.6370566531585,-37.8464798863208));
#18590=CARTESIAN_POINT('Ctrl Pts',(18.9442761565781,52.2899314565743,-37.7938303785899));
#18591=CARTESIAN_POINT('Ctrl Pts',(18.1913397487494,51.9428062599901,-37.7411808708591));
#18592=CARTESIAN_POINT('Ctrl Pts',(17.6263339027141,51.1880476760571,-37.6885313631283));
#18593=CARTESIAN_POINT('Ctrl Pts',(17.5053954905343,50.3678141121614,-37.6358818553975));
#18594=CARTESIAN_POINT('Ctrl Pts',(17.3844570783544,49.5475805482657,-37.5832323476667));
#18595=CARTESIAN_POINT('Ctrl Pts',(17.7075861000302,48.6618720044072,-37.5305828399358));
#18596=CARTESIAN_POINT('Ctrl Pts',(18.3282968953505,48.112210939538,-37.477933332205));
#18597=CARTESIAN_POINT('Ctrl Pts',(18.9490076906708,47.5625498746688,-37.4252838244742));
#18598=CARTESIAN_POINT('Ctrl Pts',(19.8673002596356,47.3489362887889,-37.3726343167434));
#18599=CARTESIAN_POINT('Ctrl Pts',(20.6668806464798,47.5682086730699,-37.3199848090125));
#18600=CARTESIAN_POINT('Ctrl Pts',(21.4664610333241,47.7874810573509,-37.2673353012817));
#18601=CARTESIAN_POINT('Ctrl Pts',(22.1473292380478,48.4396394117927,-37.2146857935509));
#18602=CARTESIAN_POINT('Ctrl Pts',(22.4008240058016,49.2290376534148,-37.1620362858201));
#18603=CARTESIAN_POINT('Ctrl Pts',(22.4801920952911,49.4761947479739,-37.145551958044));
#18604=CARTESIAN_POINT('Ctrl Pts',(22.517665263511,49.7368053091528,-37.129067630268));
#18605=CARTESIAN_POINT('Ctrl Pts',(22.5156628463169,49.9979761585217,-37.112583302492));
#18606=CARTESIAN_POINT('Ctrl Pts',(22.5136153256948,50.0005414263439,-37.387416697508));
#18607=CARTESIAN_POINT('Ctrl Pts',(22.5127372360958,49.5485663176867,-37.4158856746455));
#18608=CARTESIAN_POINT('Ctrl Pts',(22.3963340756929,49.0961693598541,-37.444354651783));
#18609=CARTESIAN_POINT('Ctrl Pts',(22.1671362634044,48.710868852972,-37.4728236289205));
#18610=CARTESIAN_POINT('Ctrl Pts',(21.7432660297921,47.9983078811531,-37.5254731366513));
#18611=CARTESIAN_POINT('Ctrl Pts',(20.9336213905881,47.5152267033671,-37.5781226443822));
#18612=CARTESIAN_POINT('Ctrl Pts',(20.1052424175224,47.4806226208699,-37.630772152113));
#18613=CARTESIAN_POINT('Ctrl Pts',(19.2768634444567,47.4460185383727,-37.6834216598438));
#18614=CARTESIAN_POINT('Ctrl Pts',(18.4297501375294,47.8598915511643,-37.7360711675746));
#18615=CARTESIAN_POINT('Ctrl Pts',(17.9479284590968,48.5346190298311,-37.7887206753054));
#18616=CARTESIAN_POINT('Ctrl Pts',(17.4661067806642,49.209346508498,-37.8413701830363));
#18617=CARTESIAN_POINT('Ctrl Pts',(17.3495767307262,50.1449284530401,-37.8940196907671));
#18618=CARTESIAN_POINT('Ctrl Pts',(17.6511653825088,50.9172322053898,-37.9466691984979));
#18619=CARTESIAN_POINT('Ctrl Pts',(17.9527540342914,51.6895359577395,-37.9993187062287));
#18620=CARTESIAN_POINT('Ctrl Pts',(18.6724613877946,52.2985615178968,-38.0519682139595));
#18621=CARTESIAN_POINT('Ctrl Pts',(19.4840191639997,52.4682180234673,-38.1046177216904));
#18622=CARTESIAN_POINT('Ctrl Pts',(20.2955769402048,52.6378745290377,-38.1572672294212));
#18623=CARTESIAN_POINT('Ctrl Pts',(21.1989851391119,52.3681619800214,-38.209916737152));
#18624=CARTESIAN_POINT('Ctrl Pts',(21.7846971822037,51.7813472460311,-38.2625662448829));
#18625=CARTESIAN_POINT('Ctrl Pts',(22.2476734241463,51.3174993817714,-38.3041830624246));
#18626=CARTESIAN_POINT('Ctrl Pts',(22.5121494139052,50.6555223852163,-38.3457998799663));
#18627=CARTESIAN_POINT('Ctrl Pts',(22.51811817366,49.9978011072146,-38.387416697508));
#18628=CARTESIAN_POINT('Origin',(20.,50.,-32.));
#18629=CARTESIAN_POINT('',(22.5201576955115,50.0015647648602,-39.387416697508));
#18630=CARTESIAN_POINT('',(22.5149457203491,50.0017607375679,-39.112583302492));
#18631=CARTESIAN_POINT('',(22.5175,50.,-32.));
#18632=CARTESIAN_POINT('',(18.086534003335,51.635987203375,-40.));
#18633=CARTESIAN_POINT('Ctrl Pts',(22.5201576955115,50.0015647648602,-39.387416697508));
#18634=CARTESIAN_POINT('Ctrl Pts',(22.5146850116671,49.2723762340521,-39.4336626084796));
#18635=CARTESIAN_POINT('Ctrl Pts',(22.1801325379537,48.5389628969671,-39.4799085194511));
#18636=CARTESIAN_POINT('Ctrl Pts',(21.6226859420216,48.0701217693743,-39.5261544304226));
#18637=CARTESIAN_POINT('Ctrl Pts',(20.9880506143681,47.5363609664587,-39.5788039381534));
#18638=CARTESIAN_POINT('Ctrl Pts',(20.0645199255084,47.34551492175,-39.6314534458842));
#18639=CARTESIAN_POINT('Ctrl Pts',(19.2708509938193,47.5857187771834,-39.6841029536151));
#18640=CARTESIAN_POINT('Ctrl Pts',(18.4771820621302,47.8259226326167,-39.7367524613459));
#18641=CARTESIAN_POINT('Ctrl Pts',(17.8133748876117,48.4971763881921,-39.7894019690767));
#18642=CARTESIAN_POINT('Ctrl Pts',(17.5804140263325,49.2914457293263,-39.8420514768075));
#18643=CARTESIAN_POINT('Ctrl Pts',(17.3474531650532,50.0857150704605,-39.8947009845383));
#18644=CARTESIAN_POINT('Ctrl Pts',(17.5453386170133,51.0029999971535,-39.9473504922692));
#18645=CARTESIAN_POINT('Ctrl Pts',(18.086534003335,51.635987203375,-40.));
#18646=CARTESIAN_POINT('',(21.9170726842248,51.6385409294649,-40.));
#18647=CARTESIAN_POINT('Origin',(20.,50.,-40.));
#18648=CARTESIAN_POINT('Ctrl Pts',(21.9170801928212,51.6385462459494,-40.));
#18649=CARTESIAN_POINT('Ctrl Pts',(21.3942483348109,52.247316763458,-39.9490537266974));
#18650=CARTESIAN_POINT('Ctrl Pts',(20.554552609146,52.5873620245221,-39.8981074533947));
#18651=CARTESIAN_POINT('Ctrl Pts',(19.7559044863995,52.5095731650181,-39.847161180092));
#18652=CARTESIAN_POINT('Ctrl Pts',(18.9305559812605,52.4291836704717,-39.7945116723612));
#18653=CARTESIAN_POINT('Ctrl Pts',(18.1490455625112,51.9025550055059,-39.7418621646304));
#18654=CARTESIAN_POINT('Ctrl Pts',(17.765166694843,51.1677991047107,-39.6892126568996));
#18655=CARTESIAN_POINT('Ctrl Pts',(17.3812878271748,50.4330432039155,-39.6365631491687));
#18656=CARTESIAN_POINT('Ctrl Pts',(17.3950405105878,49.490160067291,-39.5839136414379));
#18657=CARTESIAN_POINT('Ctrl Pts',(17.8004371569179,48.766905015811,-39.5312641337071));
#18658=CARTESIAN_POINT('Ctrl Pts',(18.2058338032481,48.0436499643311,-39.4786146259763));
#18659=CARTESIAN_POINT('Ctrl Pts',(19.0028744124954,47.5400229979957,-39.4259651182455));
#18660=CARTESIAN_POINT('Ctrl Pts',(19.8301087131647,47.484178338697,-39.3733156105146));
#18661=CARTESIAN_POINT('Ctrl Pts',(20.657343013834,47.4283336793982,-39.3206661027838));
#18662=CARTESIAN_POINT('Ctrl Pts',(21.5147710059253,47.8202713271361,-39.268016595053));
#18663=CARTESIAN_POINT('Ctrl Pts',(22.0137530473082,48.4823913654697,-39.2153670873221));
#18664=CARTESIAN_POINT('Ctrl Pts',(22.3384617672062,48.9132608802729,-39.1811058257121));
#18665=CARTESIAN_POINT('Ctrl Pts',(22.5113809799459,49.4585433263153,-39.146844564102));
#18666=CARTESIAN_POINT('Ctrl Pts',(22.5149457203491,50.0017607375679,-39.112583302492));
#18667=CARTESIAN_POINT('Origin',(20.,-50.,-32.));
#18668=CARTESIAN_POINT('',(22.5134613473905,-49.9997270421583,-25.387416697508));
#18669=CARTESIAN_POINT('',(22.5157642476295,-50.0033830516534,-25.112583302492));
#18670=CARTESIAN_POINT('',(22.5175,-50.,-32.));
#18671=CARTESIAN_POINT('',(21.9134659966651,-48.3640127966251,-25.));
#18672=CARTESIAN_POINT('Ctrl Pts',(22.5157642476295,-50.0033830516534,-25.112583302492));
#18673=CARTESIAN_POINT('Ctrl Pts',(22.5105545148632,-49.4108213760461,-25.0750555349946));
#18674=CARTESIAN_POINT('Ctrl Pts',(22.2992218280841,-48.8151964396956,-25.0375277674973));
#18675=CARTESIAN_POINT('Ctrl Pts',(21.9134659966651,-48.3640127966251,-25.));
#18676=CARTESIAN_POINT('',(22.5175,-50.,-25.));
#18677=CARTESIAN_POINT('Origin',(20.,-50.,-25.));
#18678=CARTESIAN_POINT('',(17.4825,-50.,-25.));
#18679=CARTESIAN_POINT('Ctrl Pts',(22.5175,-50.,-25.));
#18680=CARTESIAN_POINT('Ctrl Pts',(22.5175,-49.6777819917977,-25.));
#18681=CARTESIAN_POINT('Ctrl Pts',(22.4519182005811,-49.3379042845385,-24.965994767533));
#18682=CARTESIAN_POINT('Ctrl Pts',(22.1930921359231,-48.7191330360028,-24.8434341672334));
#18683=CARTESIAN_POINT('Ctrl Pts',(22.0001401774783,-48.439857534204,-24.75619390213));
#18684=CARTESIAN_POINT('Ctrl Pts',(21.5595215410958,-47.9992388978215,-24.5883213994305));
#18685=CARTESIAN_POINT('Ctrl Pts',(21.2804542351089,-47.8067418484832,-24.4956547875015));
#18686=CARTESIAN_POINT('Ctrl Pts',(20.6625974062016,-47.5482850278898,-24.3600905047278));
#18687=CARTESIAN_POINT('Ctrl Pts',(20.3231274362054,-47.4825,-24.3199761284063));
#18688=CARTESIAN_POINT('Ctrl Pts',(20.,-47.4825,-24.3199761284063));
#18689=CARTESIAN_POINT('Ctrl Pts',(19.6768725637946,-47.4825,-24.3199761284063));
#18690=CARTESIAN_POINT('Ctrl Pts',(19.3374025937983,-47.5482850278898,-24.3600905047278));
#18691=CARTESIAN_POINT('Ctrl Pts',(18.719545764891,-47.8067418484832,-24.4956547875015));
#18692=CARTESIAN_POINT('Ctrl Pts',(18.4404784589043,-47.9992388978215,-24.5883213994305));
#18693=CARTESIAN_POINT('Ctrl Pts',(17.9998598225217,-48.439857534204,-24.75619390213));
#18694=CARTESIAN_POINT('Ctrl Pts',(17.8069078640769,-48.7191330360028,-24.8434341672334));
#18695=CARTESIAN_POINT('Ctrl Pts',(17.5480817994189,-49.3379042845386,-24.965994767533));
#18696=CARTESIAN_POINT('Ctrl Pts',(17.4825,-49.6777819917977,-25.));
#18697=CARTESIAN_POINT('Ctrl Pts',(17.4825,-50.,-25.));
#18698=CARTESIAN_POINT('',(18.0829272567075,-48.3614591395872,-25.));
#18699=CARTESIAN_POINT('Origin',(20.,-50.,-25.));
#18700=CARTESIAN_POINT('Ctrl Pts',(18.082919744614,-48.3614538208575,-25.));
#18701=CARTESIAN_POINT('Ctrl Pts',(18.6057515849863,-47.7526833829372,-25.0509462733027));
#18702=CARTESIAN_POINT('Ctrl Pts',(19.4454473582538,-47.4126378852296,-25.1018925466053));
#18703=CARTESIAN_POINT('Ctrl Pts',(20.2440955154214,-47.4904266963984,-25.152838819908));
#18704=CARTESIAN_POINT('Ctrl Pts',(21.0694440561323,-47.5708161409938,-25.2054883276388));
#18705=CARTESIAN_POINT('Ctrl Pts',(21.8509544963761,-48.0974449571186,-25.2581378353696));
#18706=CARTESIAN_POINT('Ctrl Pts',(22.234833370557,-48.8322009067204,-25.3107873431004));
#18707=CARTESIAN_POINT('Ctrl Pts',(22.4210737335855,-49.188670678815,-25.3363304612363));
#18708=CARTESIAN_POINT('Ctrl Pts',(22.5137218121911,-49.5941282464848,-25.3618735793722));
#18709=CARTESIAN_POINT('Ctrl Pts',(22.5134613473905,-49.9997270421583,-25.387416697508));
#18710=CARTESIAN_POINT('Origin',(20.,-50.,-32.));
#18711=CARTESIAN_POINT('',(22.51875591101,-50.0020955263397,-26.387416697508));
#18712=CARTESIAN_POINT('',(22.5213592474396,-49.9993296992679,-26.112583302492));
#18713=CARTESIAN_POINT('',(22.5175,-50.,-32.));
#18714=CARTESIAN_POINT('Ctrl Pts',(22.5213592474396,-49.9993296992679,-26.112583302492));
#18715=CARTESIAN_POINT('Ctrl Pts',(22.5214870426669,-49.9628733533498,-26.1102687557771));
#18716=CARTESIAN_POINT('Ctrl Pts',(22.5207640617796,-49.9264222613598,-26.1079542090622));
#18717=CARTESIAN_POINT('Ctrl Pts',(22.5191744259947,-49.8900090854379,-26.1056396623473));
#18718=CARTESIAN_POINT('Ctrl Pts',(22.4830146280504,-49.0617104925164,-26.0529901546164));
#18719=CARTESIAN_POINT('Ctrl Pts',(21.9984162961223,-48.253031042163,-26.0003406468856));
#18720=CARTESIAN_POINT('Ctrl Pts',(21.2850581295563,-47.8304728873339,-25.9476911391548));
#18721=CARTESIAN_POINT('Ctrl Pts',(20.5716999629903,-47.4079147325048,-25.895041631424));
#18722=CARTESIAN_POINT('Ctrl Pts',(19.6295819617865,-47.3714778732001,-25.8423921236932));
#18723=CARTESIAN_POINT('Ctrl Pts',(18.8858121000221,-47.7378802757919,-25.7897426159623));
#18724=CARTESIAN_POINT('Ctrl Pts',(18.1420422382578,-48.1042826783837,-25.7370931082315));
#18725=CARTESIAN_POINT('Ctrl Pts',(17.5966205159329,-48.8735243428719,-25.6844436005007));
#18726=CARTESIAN_POINT('Ctrl Pts',(17.4967795653299,-49.6964831019948,-25.6317940927699));
#18727=CARTESIAN_POINT('Ctrl Pts',(17.3969386147268,-50.5194418611176,-25.5791445850391));
#18728=CARTESIAN_POINT('Ctrl Pts',(17.7426784358456,-51.3961177148752,-25.5264950773082));
#18729=CARTESIAN_POINT('Ctrl Pts',(18.3773138867814,-51.9298784728165,-25.4738455695774));
#18730=CARTESIAN_POINT('Ctrl Pts',(19.0119493377171,-52.4636392307578,-25.4211960618466));
#18731=CARTESIAN_POINT('Ctrl Pts',(19.9354804184698,-52.654484892883,-25.3685465541157));
#18732=CARTESIAN_POINT('Ctrl Pts',(20.7291491830128,-52.4142811943913,-25.3158970463849));
#18733=CARTESIAN_POINT('Ctrl Pts',(21.5228179475557,-52.1740774958997,-25.2632475386541));
#18734=CARTESIAN_POINT('Ctrl Pts',(22.1866243958889,-51.5028244367913,-25.2105980309233));
#18735=CARTESIAN_POINT('Ctrl Pts',(22.4195852547467,-50.708555063528,-25.1579485231925));
#18736=CARTESIAN_POINT('Ctrl Pts',(22.4864951603479,-50.4804288064068,-25.142826782959));
#18737=CARTESIAN_POINT('Ctrl Pts',(22.5178634992192,-50.2421546154428,-25.1277050427255));
#18738=CARTESIAN_POINT('Ctrl Pts',(22.5157642476295,-50.0033830516534,-25.112583302492));
#18739=CARTESIAN_POINT('Ctrl Pts',(22.5134613473905,-49.9997270421583,-25.387416697508));
#18740=CARTESIAN_POINT('Ctrl Pts',(22.5131849418113,-50.4301490022454,-25.414523087103));
#18741=CARTESIAN_POINT('Ctrl Pts',(22.4082797518455,-50.8607300059878,-25.4416294766979));
#18742=CARTESIAN_POINT('Ctrl Pts',(22.1995628957716,-51.2330949928824,-25.4687358662929));
#18743=CARTESIAN_POINT('Ctrl Pts',(21.7941662386876,-51.9563500463638,-25.5213853740237));
#18744=CARTESIAN_POINT('Ctrl Pts',(20.9971256164018,-52.4599770702478,-25.5740348817545));
#18745=CARTESIAN_POINT('Ctrl Pts',(20.1698912949398,-52.5158217407964,-25.6266843894854));
#18746=CARTESIAN_POINT('Ctrl Pts',(19.3426569734778,-52.5716664113451,-25.6793338972162));
#18747=CARTESIAN_POINT('Ctrl Pts',(18.4852289528396,-52.1797287285584,-25.731983404947));
#18748=CARTESIAN_POINT('Ctrl Pts',(17.9862468973199,-51.5176086672518,-25.7846329126778));
#18749=CARTESIAN_POINT('Ctrl Pts',(17.4872648418001,-50.8554886059452,-25.8372824204087));
#18750=CARTESIAN_POINT('Ctrl Pts',(17.3467287513987,-49.9231861661186,-25.8899319281395));
#18751=CARTESIAN_POINT('Ctrl Pts',(17.6283798121799,-49.1433861673454,-25.9425814358703));
#18752=CARTESIAN_POINT('Ctrl Pts',(17.9100308729611,-48.3635861685722,-25.9952309436011));
#18753=CARTESIAN_POINT('Ctrl Pts',(18.6138690849249,-47.7362886108523,-26.047880451332));
#18754=CARTESIAN_POINT('Ctrl Pts',(19.4208043833602,-47.5458493696428,-26.1005299590628));
#18755=CARTESIAN_POINT('Ctrl Pts',(20.2277396817955,-47.3554101284333,-26.1531794667936));
#18756=CARTESIAN_POINT('Ctrl Pts',(21.1377720667024,-47.6018292037341,-26.2058289745244));
#18757=CARTESIAN_POINT('Ctrl Pts',(21.7383600880492,-48.173406266917,-26.2584784822553));
#18758=CARTESIAN_POINT('Ctrl Pts',(22.2286384775488,-48.6400021230645,-26.3014578873395));
#18759=CARTESIAN_POINT('Ctrl Pts',(22.5127044815768,-49.3232818559675,-26.3444372924237));
#18760=CARTESIAN_POINT('Ctrl Pts',(22.51875591101,-50.0020955263397,-26.387416697508));
#18761=CARTESIAN_POINT('Origin',(20.,-50.,-32.));
#18762=CARTESIAN_POINT('',(22.5196060265899,-49.9981422852793,-27.387416697508));
#18763=CARTESIAN_POINT('',(22.5145120517532,-49.9984719976714,-27.112583302492));
#18764=CARTESIAN_POINT('',(22.5175,-50.,-32.));
#18765=CARTESIAN_POINT('Ctrl Pts',(22.5145120517532,-49.9984719976714,-27.112583302492));
#18766=CARTESIAN_POINT('Ctrl Pts',(22.5162682753667,-49.6851867289941,-27.0928324688287));
#18767=CARTESIAN_POINT('Ctrl Pts',(22.4619721349342,-49.372488283433,-27.0730816351654));
#18768=CARTESIAN_POINT('Ctrl Pts',(22.3488347498514,-49.0827677433124,-27.0533308015021));
#18769=CARTESIAN_POINT('Ctrl Pts',(22.0472460811345,-48.310463947083,-27.0006812937713));
#18770=CARTESIAN_POINT('Ctrl Pts',(21.3275386873248,-47.701438351122,-26.9480317860405));
#18771=CARTESIAN_POINT('Ctrl Pts',(20.515980865224,-47.5317818366054,-26.8953822783096));
#18772=CARTESIAN_POINT('Ctrl Pts',(19.7044230431231,-47.3621253220887,-26.8427327705788));
#18773=CARTESIAN_POINT('Ctrl Pts',(18.8010147927311,-47.6318378890163,-26.790083262848));
#18774=CARTESIAN_POINT('Ctrl Pts',(18.2153027169047,-48.2186526549655,-26.7374337551172));
#18775=CARTESIAN_POINT('Ctrl Pts',(17.6295906410783,-48.8054674209146,-26.6847842473863));
#18776=CARTESIAN_POINT('Ctrl Pts',(17.3615747398177,-49.7093843858853,-26.6321347396555));
#18777=CARTESIAN_POINT('Ctrl Pts',(17.5327555271831,-50.5206201517315,-26.5794852319247));
#18778=CARTESIAN_POINT('Ctrl Pts',(17.7039363145486,-51.3318559175777,-26.5268357241939));
#18779=CARTESIAN_POINT('Ctrl Pts',(18.3143137905401,-52.0504104842994,-26.474186216463));
#18780=CARTESIAN_POINT('Ctrl Pts',(19.0871834427573,-52.3505507840466,-26.4215367087322));
#18781=CARTESIAN_POINT('Ctrl Pts',(19.8600530949745,-52.6506910837937,-26.3688872010014));
#18782=CARTESIAN_POINT('Ctrl Pts',(20.7954149234172,-52.5324171165662,-26.3162376932706));
#18783=CARTESIAN_POINT('Ctrl Pts',(21.4692352056584,-52.0493212652077,-26.2635881855397));
#18784=CARTESIAN_POINT('Ctrl Pts',(22.1134333966795,-51.5874629897342,-26.2132532245238));
#18785=CARTESIAN_POINT('Ctrl Pts',(22.518580056272,-50.792153943755,-26.1629182635079));
#18786=CARTESIAN_POINT('Ctrl Pts',(22.5213592474396,-49.9993296992679,-26.112583302492));
#18787=CARTESIAN_POINT('Ctrl Pts',(22.51875591101,-50.0020955263397,-26.387416697508));
#18788=CARTESIAN_POINT('Ctrl Pts',(22.5201174455325,-50.1548244405144,-26.3970868001546));
#18789=CARTESIAN_POINT('Ctrl Pts',(22.5074052592067,-50.3073272725945,-26.4067569028011));
#18790=CARTESIAN_POINT('Ctrl Pts',(22.4798015470764,-50.4570851924628,-26.4164270054477));
#18791=CARTESIAN_POINT('Ctrl Pts',(22.3295113269701,-51.2724520037605,-26.4690765131785));
#18792=CARTESIAN_POINT('Ctrl Pts',(21.7377872289705,-52.006450575291,-26.5217260209094));
#18793=CARTESIAN_POINT('Ctrl Pts',(20.9728803659084,-52.3263363422347,-26.5743755286402));
#18794=CARTESIAN_POINT('Ctrl Pts',(20.2079735028462,-52.6462221091785,-26.627025036371));
#18795=CARTESIAN_POINT('Ctrl Pts',(19.2698838747213,-52.5519950715356,-26.6796745441018));
#18796=CARTESIAN_POINT('Ctrl Pts',(18.5838791489413,-52.0863703552799,-26.7323240518326));
#18797=CARTESIAN_POINT('Ctrl Pts',(17.8978744231613,-51.6207456390243,-26.7849735595635));
#18798=CARTESIAN_POINT('Ctrl Pts',(17.4639545997261,-50.7837232441561,-26.8376230672943));
#18799=CARTESIAN_POINT('Ctrl Pts',(17.4788311344027,-49.9547551821562,-26.8902725750251));
#18800=CARTESIAN_POINT('Ctrl Pts',(17.4937076690793,-49.1257871201564,-26.942922082756));
#18801=CARTESIAN_POINT('Ctrl Pts',(17.9573805618677,-48.304873391025,-26.9955715904868));
#18802=CARTESIAN_POINT('Ctrl Pts',(18.6596505054912,-47.8641624303278,-27.0482210982176));
#18803=CARTESIAN_POINT('Ctrl Pts',(19.3619204491148,-47.4234514696305,-27.1008706059484));
#18804=CARTESIAN_POINT('Ctrl Pts',(20.3027874435735,-47.3629432773675,-27.1535201136792));
#18805=CARTESIAN_POINT('Ctrl Pts',(21.0557238712505,-47.7100684831199,-27.2061696214101));
#18806=CARTESIAN_POINT('Ctrl Pts',(21.8086602989275,-48.0571936888723,-27.2588191291409));
#18807=CARTESIAN_POINT('Ctrl Pts',(22.3736661598227,-48.81195229264,-27.3114686368717));
#18808=CARTESIAN_POINT('Ctrl Pts',(22.4946045751828,-49.6321858781341,-27.3641181446025));
#18809=CARTESIAN_POINT('Ctrl Pts',(22.5124438687173,-49.7531762818444,-27.3718843289044));
#18810=CARTESIAN_POINT('Ctrl Pts',(22.5206209696132,-49.8755913157382,-27.3796505132062));
#18811=CARTESIAN_POINT('Ctrl Pts',(22.5196060265899,-49.9981422852793,-27.387416697508));
#18812=CARTESIAN_POINT('Origin',(20.,-50.,-32.));
#18813=CARTESIAN_POINT('',(22.5135352489342,-49.9997146182226,-28.387416697508));
#18814=CARTESIAN_POINT('',(22.5160873419658,-50.0021236034949,-28.112583302492));
#18815=CARTESIAN_POINT('',(22.5175,-50.,-32.));
#18816=CARTESIAN_POINT('Ctrl Pts',(22.5160873419658,-50.0021236034949,-28.112583302492));
#18817=CARTESIAN_POINT('Ctrl Pts',(22.5112879704401,-49.4131979553026,-28.0753961818803));
#18818=CARTESIAN_POINT('Ctrl Pts',(22.3047334737028,-48.821238787295,-28.0382090612686));
#18819=CARTESIAN_POINT('Ctrl Pts',(21.9270452588827,-48.3737048452096,-28.0010219406569));
#18820=CARTESIAN_POINT('Ctrl Pts',(21.3923144634106,-47.7400865021905,-27.9483724329261));
#18821=CARTESIAN_POINT('Ctrl Pts',(20.5145481327378,-47.3959668343932,-27.8957229251952));
#18822=CARTESIAN_POINT('Ctrl Pts',(19.6916682831495,-47.4973472343812,-27.8430734174644));
#18823=CARTESIAN_POINT('Ctrl Pts',(18.8687884335611,-47.5987276343691,-27.7904239097336));
#18824=CARTESIAN_POINT('Ctrl Pts',(18.1007950650571,-48.1456081021423,-27.7377744020028));
#18825=CARTESIAN_POINT('Ctrl Pts',(17.7358462958969,-48.89006874545,-27.685124894272));
#18826=CARTESIAN_POINT('Ctrl Pts',(17.3708975267368,-49.6345293887576,-27.6324753865411));
#18827=CARTESIAN_POINT('Ctrl Pts',(17.4089933569204,-50.5765702075996,-27.5798258788103));
#18828=CARTESIAN_POINT('Ctrl Pts',(17.8328636144219,-51.289131219645,-27.5271763710795));
#18829=CARTESIAN_POINT('Ctrl Pts',(18.2567338719235,-52.0016922316905,-27.4745268633487));
#18830=CARTESIAN_POINT('Ctrl Pts',(19.0663785567431,-52.4847734369395,-27.4218773556178));
#18831=CARTESIAN_POINT('Ctrl Pts',(19.8947575765285,-52.5193775212888,-27.369227847887));
#18832=CARTESIAN_POINT('Ctrl Pts',(20.723136596314,-52.5539816056381,-27.3165783401562));
#18833=CARTESIAN_POINT('Ctrl Pts',(21.5702499510653,-52.1401085690878,-27.2639288324254));
#18834=CARTESIAN_POINT('Ctrl Pts',(22.0520716566289,-51.4653810525637,-27.2112793246946));
#18835=CARTESIAN_POINT('Ctrl Pts',(22.3531437071225,-51.0437695008659,-27.178380650627));
#18836=CARTESIAN_POINT('Ctrl Pts',(22.511586735828,-50.5203066766564,-27.1454819765595));
#18837=CARTESIAN_POINT('Ctrl Pts',(22.5145120517532,-49.9984719976714,-27.112583302492));
#18838=CARTESIAN_POINT('Ctrl Pts',(22.5196060265899,-49.9981422852793,-27.387416697508));
#18839=CARTESIAN_POINT('Ctrl Pts',(22.5137403383433,-50.7064044882707,-27.432300020937));
#18840=CARTESIAN_POINT('Ctrl Pts',(22.2008546131046,-51.4192070272122,-27.477183344366));
#18841=CARTESIAN_POINT('Ctrl Pts',(21.6717031486973,-51.8877891102062,-27.522066667795));
#18842=CARTESIAN_POINT('Ctrl Pts',(21.0509923370266,-52.4374501895634,-27.5747161755258));
#18843=CARTESIAN_POINT('Ctrl Pts',(20.1326997438602,-52.6510637810572,-27.6273656832566));
#18844=CARTESIAN_POINT('Ctrl Pts',(19.333119335948,-52.4317913909958,-27.6800151909875));
#18845=CARTESIAN_POINT('Ctrl Pts',(18.5335389280356,-52.2125190009344,-27.7326646987183));
#18846=CARTESIAN_POINT('Ctrl Pts',(17.8526707053774,-51.5603606293177,-27.7853142064491));
#18847=CARTESIAN_POINT('Ctrl Pts',(17.5991759309459,-50.7709623668994,-27.8379637141799));
#18848=CARTESIAN_POINT('Ctrl Pts',(17.3456811565143,-49.9815641044811,-27.8906132219107));
#18849=CARTESIAN_POINT('Ctrl Pts',(17.5195598303094,-49.0549259512611,-27.9432627296416));
#18850=CARTESIAN_POINT('Ctrl Pts',(18.0419866956553,-48.4111252176501,-27.9959122373724));
#18851=CARTESIAN_POINT('Ctrl Pts',(18.5644135610011,-47.7673244840391,-28.0485617451032));
#18852=CARTESIAN_POINT('Ctrl Pts',(19.4353886178977,-47.4063611700371,-28.1012112528341));
#18853=CARTESIAN_POINT('Ctrl Pts',(20.2600685710903,-47.4918725075265,-28.1538607605649));
#18854=CARTESIAN_POINT('Ctrl Pts',(21.0847485242829,-47.5773838450159,-28.2065102682957));
#18855=CARTESIAN_POINT('Ctrl Pts',(21.8631333737715,-48.1093698339967,-28.2591597760265));
#18856=CARTESIAN_POINT('Ctrl Pts',(22.2423541837709,-48.8466627148794,-28.3118092837573));
#18857=CARTESIAN_POINT('Ctrl Pts',(22.4238810768686,-49.1995929403326,-28.3370117550075));
#18858=CARTESIAN_POINT('Ctrl Pts',(22.5139442132876,-49.5995668314161,-28.3622142262578));
#18859=CARTESIAN_POINT('Ctrl Pts',(22.5135352489342,-49.9997146182226,-28.387416697508));
#18860=CARTESIAN_POINT('Origin',(20.,-50.,-32.));
#18861=CARTESIAN_POINT('',(22.5185978370021,-50.0021261700316,-29.387416697508));
#18862=CARTESIAN_POINT('',(22.5214169330132,-49.9994390864176,-29.112583302492));
#18863=CARTESIAN_POINT('',(22.5175,-50.,-32.));
#18864=CARTESIAN_POINT('Ctrl Pts',(22.5214169330132,-49.9994390864176,-29.112583302492));
#18865=CARTESIAN_POINT('Ctrl Pts',(22.5215116550139,-49.9683497400867,-29.1106094026627));
#18866=CARTESIAN_POINT('Ctrl Pts',(22.5209858636051,-49.9372636712048,-29.1086355028335));
#18867=CARTESIAN_POINT('Ctrl Pts',(22.5198295796509,-49.9062010719754,-29.1066616030042));
#18868=CARTESIAN_POINT('Ctrl Pts',(22.488988206606,-49.077673436471,-29.0540120952734));
#18869=CARTESIAN_POINT('Ctrl Pts',(22.0095890811262,-48.2658430556014,-29.0013625875425));
#18870=CARTESIAN_POINT('Ctrl Pts',(21.2989605066287,-47.8387408873901,-28.9487130798117));
#18871=CARTESIAN_POINT('Ctrl Pts',(20.5883319321312,-47.4116387191788,-28.8960635720809));
#18872=CARTESIAN_POINT('Ctrl Pts',(19.6464739086159,-47.3692647636258,-28.8434140643501));
#18873=CARTESIAN_POINT('Ctrl Pts',(18.900363448358,-47.7308286086929,-28.7907645566192));
#18874=CARTESIAN_POINT('Ctrl Pts',(18.1542529881,-48.0923924537599,-28.7381150488884));
#18875=CARTESIAN_POINT('Ctrl Pts',(17.6038900910993,-48.8578940994471,-28.6854655411576));
#18876=CARTESIAN_POINT('Ctrl Pts',(17.4987734074998,-49.6803050163489,-28.6328160334268));
#18877=CARTESIAN_POINT('Ctrl Pts',(17.3936567239004,-50.5027159332509,-28.580166525696));
#18878=CARTESIAN_POINT('Ctrl Pts',(17.7337862537023,-51.3820361213676,-28.5275170179651));
#18879=CARTESIAN_POINT('Ctrl Pts',(18.3649694467479,-51.9196391434274,-28.4748675102343));
#18880=CARTESIAN_POINT('Ctrl Pts',(18.9961526397934,-52.4572421654872,-28.4222180025035));
#18881=CARTESIAN_POINT('Ctrl Pts',(19.9183894960826,-52.6531280214901,-28.3695684947727));
#18882=CARTESIAN_POINT('Ctrl Pts',(20.7135979613149,-52.4184948406945,-28.3169189870418));
#18883=CARTESIAN_POINT('Ctrl Pts',(21.5088064265471,-52.1838616598988,-28.264269479311));
#18884=CARTESIAN_POINT('Ctrl Pts',(22.1769865007224,-51.5187094423045,-28.2116199715802));
#18885=CARTESIAN_POINT('Ctrl Pts',(22.4152289076743,-50.7245748243869,-28.1589704638494));
#18886=CARTESIAN_POINT('Ctrl Pts',(22.4851972033575,-50.4913491511343,-28.1435080767302));
#18887=CARTESIAN_POINT('Ctrl Pts',(22.5180829183707,-50.246998608791,-28.1280456896111));
#18888=CARTESIAN_POINT('Ctrl Pts',(22.5160873419658,-50.0021236034949,-28.112583302492));
#18889=CARTESIAN_POINT('Ctrl Pts',(22.5135352489342,-49.9997146182226,-28.387416697508));
#18890=CARTESIAN_POINT('Ctrl Pts',(22.5130898616776,-50.4355000931096,-28.4148637339886));
#18891=CARTESIAN_POINT('Ctrl Pts',(22.4053396278516,-50.8714918178098,-28.4423107704692));
#18892=CARTESIAN_POINT('Ctrl Pts',(22.1915654556312,-51.2471487608302,-28.4697578069498));
#18893=CARTESIAN_POINT('Ctrl Pts',(21.7814991469819,-51.9677421531138,-28.5224073146806));
#18894=CARTESIAN_POINT('Ctrl Pts',(20.9813097591729,-52.4663291648967,-28.5750568224115));
#18895=CARTESIAN_POINT('Ctrl Pts',(20.1537509825797,-52.5168829559793,-28.6277063301423));
#18896=CARTESIAN_POINT('Ctrl Pts',(19.3261922059864,-52.5674367470618,-28.6803558378731));
#18897=CARTESIAN_POINT('Ctrl Pts',(18.4712640406088,-52.1699573174439,-28.7330053456039));
#18898=CARTESIAN_POINT('Ctrl Pts',(17.976535169618,-51.504635922312,-28.7856548533348));
#18899=CARTESIAN_POINT('Ctrl Pts',(17.4818062986271,-50.8393145271801,-28.8383043610656));
#18900=CARTESIAN_POINT('Ctrl Pts',(17.347276722023,-49.9061511665343,-28.8909538687964));
#18901=CARTESIAN_POINT('Ctrl Pts',(17.633933377528,-49.1281812594003,-28.9436033765272));
#18902=CARTESIAN_POINT('Ctrl Pts',(17.9205900330329,-48.3502113522664,-28.996252884258));
#18903=CARTESIAN_POINT('Ctrl Pts',(18.628432920647,-47.7274348986443,-29.0489023919888));
#18904=CARTESIAN_POINT('Ctrl Pts',(19.4365722313371,-47.5421781333803,-29.1015518997197));
#18905=CARTESIAN_POINT('Ctrl Pts',(20.2447115420273,-47.3569213681163,-29.1542014074505));
#18906=CARTESIAN_POINT('Ctrl Pts',(21.1531472757935,-47.6091842912105,-29.2068509151813));
#18907=CARTESIAN_POINT('Ctrl Pts',(21.7500539071284,-48.1846073425723,-29.2595004229122));
#18908=CARTESIAN_POINT('Ctrl Pts',(22.233465027528,-48.6506197595234,-29.3021391811108));
#18909=CARTESIAN_POINT('Ctrl Pts',(22.512552285434,-49.3285845273022,-29.3447779393094));
#18910=CARTESIAN_POINT('Ctrl Pts',(22.5185978370021,-50.0021261700316,-29.387416697508));
#18911=CARTESIAN_POINT('Origin',(20.,-50.,-32.));
#18912=CARTESIAN_POINT('',(22.5197500022945,-49.9981961379119,-30.387416697508));
#18913=CARTESIAN_POINT('',(22.5146149548606,-49.9984092956174,-30.112583302492));
#18914=CARTESIAN_POINT('',(22.5175,-50.,-32.));
#18915=CARTESIAN_POINT('Ctrl Pts',(22.5146149548606,-49.9984092956174,-30.112583302492));
#18916=CARTESIAN_POINT('Ctrl Pts',(22.5164166726556,-49.6905590369979,-30.0931731157143));
#18917=CARTESIAN_POINT('Ctrl Pts',(22.4640314720864,-49.3833005485878,-30.0737629289366));
#18918=CARTESIAN_POINT('Ctrl Pts',(22.354675889286,-49.0978687424812,-30.054352742159));
#18919=CARTESIAN_POINT('Ctrl Pts',(22.0580523859675,-48.3236441430802,-30.0017032344282));
#18920=CARTESIAN_POINT('Ctrl Pts',(21.3422703279879,-47.7100089631121,-29.9490537266973));
#18921=CARTESIAN_POINT('Ctrl Pts',(20.531818626569,-47.5351453799835,-29.8964042189665));
#18922=CARTESIAN_POINT('Ctrl Pts',(19.7213669251501,-47.3602817968549,-29.8437547112357));
#18923=CARTESIAN_POINT('Ctrl Pts',(18.8162455802918,-47.6241898105659,-29.7911052035049));
#18924=CARTESIAN_POINT('Ctrl Pts',(18.2267775896746,-48.2072307362936,-29.738455695774));
#18925=CARTESIAN_POINT('Ctrl Pts',(17.6373095990573,-48.7902716620213,-29.6858061880432));
#18926=CARTESIAN_POINT('Ctrl Pts',(17.363494962681,-49.6924454997657,-29.6331566803124));
#18927=CARTESIAN_POINT('Ctrl Pts',(17.5294633821,-50.5047654593872,-29.5805071725816));
#18928=CARTESIAN_POINT('Ctrl Pts',(17.6954318015189,-51.3170854190086,-29.5278576648508));
#18929=CARTESIAN_POINT('Ctrl Pts',(18.301183276733,-52.0395515005071,-29.4752081571199));
#18930=CARTESIAN_POINT('Ctrl Pts',(19.0721095880014,-52.3446446922152,-29.4225586493891));
#18931=CARTESIAN_POINT('Ctrl Pts',(19.8430358992699,-52.6497378839233,-29.3699091416583));
#18932=CARTESIAN_POINT('Ctrl Pts',(20.7791370465926,-52.5374581858409,-29.3172596339275));
#18933=CARTESIAN_POINT('Ctrl Pts',(21.4560458099491,-52.0587058917301,-29.2646101261966));
#18934=CARTESIAN_POINT('Ctrl Pts',(22.1075763665567,-51.597902655689,-29.2139345182951));
#18935=CARTESIAN_POINT('Ctrl Pts',(22.5189851505611,-50.797590796662,-29.1632589103935));
#18936=CARTESIAN_POINT('Ctrl Pts',(22.5214169330132,-49.9994390864176,-29.112583302492));
#18937=CARTESIAN_POINT('Ctrl Pts',(22.5185978370021,-50.0021261700316,-29.387416697508));
#18938=CARTESIAN_POINT('Ctrl Pts',(22.5200172147018,-50.160260622575,-29.3974274470402));
#18939=CARTESIAN_POINT('Ctrl Pts',(22.5063860176688,-50.3181512641088,-29.4074381965724));
#18940=CARTESIAN_POINT('Ctrl Pts',(22.4768149308017,-50.4729978615716,-29.4174489461046));
#18941=CARTESIAN_POINT('Ctrl Pts',(22.3212917942364,-51.28738214958,-29.4700984538354));
#18942=CARTESIAN_POINT('Ctrl Pts',(21.7248679922022,-52.0175675459674,-29.5227479615663));
#18943=CARTESIAN_POINT('Ctrl Pts',(20.9579231856422,-52.3325356050689,-29.5753974692971));
#18944=CARTESIAN_POINT('Ctrl Pts',(20.1909783790822,-52.6475036641704,-29.6280469770279));
#18945=CARTESIAN_POINT('Ctrl Pts',(19.2535125679963,-52.547254385986,-29.6806964847587));
#18946=CARTESIAN_POINT('Ctrl Pts',(18.5705116219756,-52.0772342563112,-29.7333459924895));
#18947=CARTESIAN_POINT('Ctrl Pts',(17.8875106759548,-51.6072141266365,-29.7859955002204));
#18948=CARTESIAN_POINT('Ctrl Pts',(17.4589745949992,-50.7674231454713,-29.8386450079512));
#18949=CARTESIAN_POINT('Ctrl Pts',(17.479173694741,-49.9385677835816,-29.891294515682));
#18950=CARTESIAN_POINT('Ctrl Pts',(17.4993727944828,-49.1097124216919,-29.9439440234129));
#18951=CARTESIAN_POINT('Ctrl Pts',(17.9683070749221,-48.2917926790776,-29.9965935311437));
#18952=CARTESIAN_POINT('Ctrl Pts',(18.6733923110178,-47.8556000331014,-30.0492430388745));
#18953=CARTESIAN_POINT('Ctrl Pts',(19.3784775471136,-47.4194073871252,-30.1018925466053));
#18954=CARTESIAN_POINT('Ctrl Pts',(20.319713738866,-47.3649418377871,-30.1545420543362));
#18955=CARTESIAN_POINT('Ctrl Pts',(21.070405771946,-47.7168945136317,-30.207191562067));
#18956=CARTESIAN_POINT('Ctrl Pts',(21.8210978050261,-48.0688471894763,-30.2598410697978));
#18957=CARTESIAN_POINT('Ctrl Pts',(22.3812456794339,-48.8272180905037,-30.3124905775286));
#18958=CARTESIAN_POINT('Ctrl Pts',(22.4969148743706,-49.6482113011374,-30.3651400852594));
#18959=CARTESIAN_POINT('Ctrl Pts',(22.5132285299378,-49.764001857721,-30.3725656226756));
#18960=CARTESIAN_POINT('Ctrl Pts',(22.5207008456371,-49.8810380648793,-30.3799911600918));
#18961=CARTESIAN_POINT('Ctrl Pts',(22.5197500022945,-49.9981961379119,-30.387416697508));
#18962=CARTESIAN_POINT('Origin',(20.,-50.,-32.));
#18963=CARTESIAN_POINT('',(22.5135564443693,-49.9996286810393,-31.387416697508));
#18964=CARTESIAN_POINT('',(22.5159431077322,-50.0020935760098,-31.112583302492));
#18965=CARTESIAN_POINT('',(22.5175,-50.,-32.));
#18966=CARTESIAN_POINT('Ctrl Pts',(22.5159431077322,-50.0020935760098,-31.112583302492));
#18967=CARTESIAN_POINT('Ctrl Pts',(22.5112751113286,-49.4184778817386,-31.0757368287659));
#18968=CARTESIAN_POINT('Ctrl Pts',(22.3088214262113,-48.8319400870852,-31.0388903550399));
#18969=CARTESIAN_POINT('Ctrl Pts',(21.9374479719839,-48.3861119291495,-31.0020438813138));
#18970=CARTESIAN_POINT('Ctrl Pts',(21.4067966620449,-47.7490731388881,-30.949394373583));
#18971=CARTESIAN_POINT('Ctrl Pts',(20.5312580173509,-47.399324414423,-30.8967448658522));
#18972=CARTESIAN_POINT('Ctrl Pts',(19.707744168322,-47.4954190214273,-30.8440953581213));
#18973=CARTESIAN_POINT('Ctrl Pts',(18.884230319293,-47.5915136284316,-30.7914458503905));
#18974=CARTESIAN_POINT('Ctrl Pts',(18.112741265929,-48.1334515669052,-30.7387963426597));
#18975=CARTESIAN_POINT('Ctrl Pts',(17.7430198386832,-48.8755535135898,-30.6861468349289));
#18976=CARTESIAN_POINT('Ctrl Pts',(17.3732984114373,-49.6176554602744,-30.633497327198));
#18977=CARTESIAN_POINT('Ctrl Pts',(17.4053446103095,-50.5599214151699,-30.5808478194672));
#18978=CARTESIAN_POINT('Ctrl Pts',(17.8246307783617,-51.2751894364864,-30.5281983117364));
#18979=CARTESIAN_POINT('Ctrl Pts',(18.2439169464138,-51.9904574578029,-30.4755488040056));
#18980=CARTESIAN_POINT('Ctrl Pts',(19.0504430836459,-52.4787275455404,-30.4228992962747));
#18981=CARTESIAN_POINT('Ctrl Pts',(19.8785828304355,-52.5186498804545,-30.3702497885439));
#18982=CARTESIAN_POINT('Ctrl Pts',(20.7067225772251,-52.5585722153686,-30.3176002808131));
#18983=CARTESIAN_POINT('Ctrl Pts',(21.5564759335723,-52.1501467974592,-30.2649507730823));
#18984=CARTESIAN_POINT('Ctrl Pts',(22.0426201374171,-51.4785270790876,-30.2123012653515));
#18985=CARTESIAN_POINT('Ctrl Pts',(22.3495385478177,-51.054512034321,-30.1790619443983));
#18986=CARTESIAN_POINT('Ctrl Pts',(22.5115295710495,-50.5255929682414,-30.1458226234451));
#18987=CARTESIAN_POINT('Ctrl Pts',(22.5146149548606,-49.9984092956174,-30.112583302492));
#18988=CARTESIAN_POINT('Ctrl Pts',(22.5197500022945,-49.9981961379119,-30.387416697508));
#18989=CARTESIAN_POINT('Ctrl Pts',(22.5139590529408,-50.7117274178686,-30.4326406678226));
#18990=CARTESIAN_POINT('Ctrl Pts',(22.1957353228996,-51.4297789608027,-30.4778646381373));
#18991=CARTESIAN_POINT('Ctrl Pts',(21.6595472004365,-51.8984842027323,-30.5230886084519));
#18992=CARTESIAN_POINT('Ctrl Pts',(21.0353198161003,-52.4441483734534,-30.5757381161827));
#18993=CARTESIAN_POINT('Ctrl Pts',(20.1156745319623,-52.6518611946555,-30.6283876239135));
#18994=CARTESIAN_POINT('Ctrl Pts',(19.3175185527131,-52.4274592174967,-30.6810371316444));
#18995=CARTESIAN_POINT('Ctrl Pts',(18.519362573464,-52.2030572403379,-30.7336866393752));
#18996=CARTESIAN_POINT('Ctrl Pts',(17.8426958991036,-51.5465404648181,-30.786336147106));
#18997=CARTESIAN_POINT('Ctrl Pts',(17.5942750765099,-50.7555307875917,-30.8389856548368));
#18998=CARTESIAN_POINT('Ctrl Pts',(17.3458542539162,-49.9645211103653,-30.8916351625677));
#18999=CARTESIAN_POINT('Ctrl Pts',(17.5256792830892,-49.0390185314322,-30.9442846702985));
#19000=CARTESIAN_POINT('Ctrl Pts',(18.0522292216189,-48.3985855710075,-30.9969341780293));
#19001=CARTESIAN_POINT('Ctrl Pts',(18.5787791601487,-47.7581526105828,-31.0495836857601));
#19002=CARTESIAN_POINT('Ctrl Pts',(19.452054008035,-47.4027892686665,-31.102233193491));
#19003=CARTESIAN_POINT('Ctrl Pts',(20.2761678927157,-47.4935941123726,-31.1548827012218));
#19004=CARTESIAN_POINT('Ctrl Pts',(21.1002817773964,-47.5843989560786,-31.2075322089526));
#19005=CARTESIAN_POINT('Ctrl Pts',(21.8752346988714,-48.1213719854071,-31.2601817166834));
#19006=CARTESIAN_POINT('Ctrl Pts',(22.2497135347539,-48.8610846431602,-31.3128312244142));
#19007=CARTESIAN_POINT('Ctrl Pts',(22.4265476106501,-49.2103871717109,-31.3376930487788));
#19008=CARTESIAN_POINT('Ctrl Pts',(22.5140816211901,-49.6048977741917,-31.3625548731434));
#19009=CARTESIAN_POINT('Ctrl Pts',(22.5135564443693,-49.9996286810393,-31.387416697508));
#19010=CARTESIAN_POINT('Origin',(20.,-50.,-32.));
#19011=CARTESIAN_POINT('',(22.5184387847934,-50.0021533196134,-32.387416697508));
#19012=CARTESIAN_POINT('',(22.5214654524887,-49.9995340141484,-32.112583302492));
#19013=CARTESIAN_POINT('',(22.5175,-50.,-32.));
#19014=CARTESIAN_POINT('Ctrl Pts',(22.5214654524887,-49.9995340141484,-32.112583302492));
#19015=CARTESIAN_POINT('Ctrl Pts',(22.5215315387758,-49.9738112570963,-32.1109500495483));
#19016=CARTESIAN_POINT('Ctrl Pts',(22.5211716022436,-49.9480903941566,-32.1093167966047));
#19017=CARTESIAN_POINT('Ctrl Pts',(22.5203799165757,-49.9223828272867,-32.107683543661));
#19018=CARTESIAN_POINT('Ctrl Pts',(22.4948591539416,-49.0936742393547,-32.0550340359302));
#19019=CARTESIAN_POINT('Ctrl Pts',(22.0206826727711,-48.2787823733245,-32.0023845281994));
#19020=CARTESIAN_POINT('Ctrl Pts',(21.3128111700898,-47.8471260647531,-31.9497350204686));
#19021=CARTESIAN_POINT('Ctrl Pts',(20.6049396674085,-47.4154697561817,-31.8970855127378));
#19022=CARTESIAN_POINT('Ctrl Pts',(19.6633731432164,-47.3670490050691,-31.8444360050069));
#19023=CARTESIAN_POINT('Ctrl Pts',(18.9149564630304,-47.7238146226069,-31.7917864972761));
#19024=CARTESIAN_POINT('Ctrl Pts',(18.1665397828444,-48.0805802401446,-31.7391369895453));
#19025=CARTESIAN_POINT('Ctrl Pts',(17.6112729466644,-48.8425322263327,-31.6864874818145));
#19026=CARTESIAN_POINT('Ctrl Pts',(17.5008777308339,-49.6642512350939,-31.6338379740837));
#19027=CARTESIAN_POINT('Ctrl Pts',(17.3904825150034,-50.4859702438552,-31.5811884663529));
#19028=CARTESIAN_POINT('Ctrl Pts',(17.7249589195224,-51.3674562751895,-31.528538958622));
#19029=CARTESIAN_POINT('Ctrl Pts',(18.3526771527223,-51.9091010413843,-31.4758894508912));
#19030=CARTESIAN_POINT('Ctrl Pts',(18.9803953859221,-52.4507458075792,-31.4232399431604));
#19031=CARTESIAN_POINT('Ctrl Pts',(19.9013554478028,-52.6525493086346,-31.3705904354296));
#19032=CARTESIAN_POINT('Ctrl Pts',(20.6980540991777,-52.423026996135,-31.3179409276987));
#19033=CARTESIAN_POINT('Ctrl Pts',(21.4947527505527,-52.1935046836355,-31.2652914199679));
#19034=CARTESIAN_POINT('Ctrl Pts',(22.1671899914219,-51.5326565575811,-31.2126419122371));
#19035=CARTESIAN_POINT('Ctrl Pts',(22.4105266242645,-50.740068066525,-31.1599924045063));
#19036=CARTESIAN_POINT('Ctrl Pts',(22.4835654284082,-50.502168351679,-31.1441893705015));
#19037=CARTESIAN_POINT('Ctrl Pts',(22.5179451583612,-50.2523997174019,-31.1283863364967));
#19038=CARTESIAN_POINT('Ctrl Pts',(22.5159431077322,-50.0020935760098,-31.112583302492));
#19039=CARTESIAN_POINT('Ctrl Pts',(22.5135564443693,-49.9996286810393,-31.387416697508));
#19040=CARTESIAN_POINT('Ctrl Pts',(22.5129694622158,-50.4408134184701,-31.4152043808743));
#19041=CARTESIAN_POINT('Ctrl Pts',(22.402377241224,-50.8822733643739,-31.4429920642405));
#19042=CARTESIAN_POINT('Ctrl Pts',(22.183512336775,-51.2611950894497,-31.4707797476067));
#19043=CARTESIAN_POINT('Ctrl Pts',(21.7688275526236,-51.9791405918085,-31.5234292553376));
#19044=CARTESIAN_POINT('Ctrl Pts',(20.9654532340308,-52.4725793103486,-31.5760787630683));
#19045=CARTESIAN_POINT('Ctrl Pts',(20.137586911568,-52.5178183056499,-31.6287282707992));
#19046=CARTESIAN_POINT('Ctrl Pts',(19.3097205891052,-52.5630573009512,-31.68137777853));
#19047=CARTESIAN_POINT('Ctrl Pts',(18.4573622627723,-52.1600965730137,-31.7340272862608));
#19048=CARTESIAN_POINT('Ctrl Pts',(17.966915618159,-51.4916122400996,-31.7866767939916));
#19049=CARTESIAN_POINT('Ctrl Pts',(17.4764689735458,-50.8231279071855,-31.8393263017225));
#19050=CARTESIAN_POINT('Ctrl Pts',(17.3479340106522,-49.8891199692948,-31.8919758094533));
#19051=CARTESIAN_POINT('Ctrl Pts',(17.6395801002989,-49.1130067217866,-31.9446253171841));
#19052=CARTESIAN_POINT('Ctrl Pts',(17.9312261899457,-48.3368934742784,-31.9972748249149));
#19053=CARTESIAN_POINT('Ctrl Pts',(18.6430533321328,-47.7186749171526,-32.0499243326458));
#19054=CARTESIAN_POINT('Ctrl Pts',(19.4523655165717,-47.5386110321486,-32.1025738403766));
#19055=CARTESIAN_POINT('Ctrl Pts',(20.2616777010105,-47.3585471471445,-32.1552233481074));
#19056=CARTESIAN_POINT('Ctrl Pts',(21.1684749277012,-47.6166379342622,-32.2078728558382));
#19057=CARTESIAN_POINT('Ctrl Pts',(21.7616744634189,-48.1958818598999,-32.2605223635691));
#19058=CARTESIAN_POINT('Ctrl Pts',(22.2382453009068,-48.6612408936304,-32.302820474882));
#19059=CARTESIAN_POINT('Ctrl Pts',(22.5124088354348,-49.3338837896983,-32.345118586195));
#19060=CARTESIAN_POINT('Ctrl Pts',(22.5184387847934,-50.0021533196134,-32.387416697508));
#19061=CARTESIAN_POINT('Origin',(20.,-50.,-32.));
#19062=CARTESIAN_POINT('',(22.5198908044257,-49.9982532979407,-33.387416697508));
#19063=CARTESIAN_POINT('',(22.5147221745587,-49.9983487241263,-33.112583302492));
#19064=CARTESIAN_POINT('',(22.5175,-50.,-32.));
#19065=CARTESIAN_POINT('Ctrl Pts',(22.5147221745587,-49.9983487241263,-33.112583302492));
#19066=CARTESIAN_POINT('Ctrl Pts',(22.5165647036742,-49.6959336362168,-33.0935137625999));
#19067=CARTESIAN_POINT('Ctrl Pts',(22.4660535271598,-49.3941132837153,-33.0744442227079));
#19068=CARTESIAN_POINT('Ctrl Pts',(22.3604199314187,-49.1130067098679,-33.0553746828159));
#19069=CARTESIAN_POINT('Ctrl Pts',(22.068773837853,-48.3368934519308,-33.0027251750851));
#19070=CARTESIAN_POINT('Ctrl Pts',(21.3569466861009,-47.7186748864979,-32.9500756673543));
#19071=CARTESIAN_POINT('Ctrl Pts',(20.5476344907871,-47.5386109990743,-32.8974261596234));
#19072=CARTESIAN_POINT('Ctrl Pts',(19.7383222954733,-47.3585471116506,-32.8447766518926));
#19073=CARTESIAN_POINT('Ctrl Pts',(18.8315250565977,-47.6166379022362,-32.7921271441618));
#19074=CARTESIAN_POINT('Ctrl Pts',(18.238325512909,-48.1958818356575,-32.7394776364309));
#19075=CARTESIAN_POINT('Ctrl Pts',(17.6451259692203,-48.7751257690787,-32.6868281287001));
#19076=CARTESIAN_POINT('Ctrl Pts',(17.3655241207184,-49.6755228453355,-32.6341786209693));
#19077=CARTESIAN_POINT('Ctrl Pts',(17.5262732135688,-50.4888917420764,-32.5815291132385));
#19078=CARTESIAN_POINT('Ctrl Pts',(17.6870223064191,-51.3022606388174,-32.5288796055077));
#19079=CARTESIAN_POINT('Ctrl Pts',(18.2881223406218,-52.0286013560425,-32.4762300977768));
#19080=CARTESIAN_POINT('Ctrl Pts',(19.0570737564864,-52.3386383749249,-32.423580590046));
#19081=CARTESIAN_POINT('Ctrl Pts',(19.8260251723511,-52.6486753938073,-32.3709310823152));
#19082=CARTESIAN_POINT('Ctrl Pts',(20.7628279698778,-52.542408714347,-32.3182815745844));
#19083=CARTESIAN_POINT('Ctrl Pts',(21.4427968465925,-52.0680127196999,-32.2656320668536));
#19084=CARTESIAN_POINT('Ctrl Pts',(22.1016722465143,-51.608333076413,-32.2146158120664));
#19085=CARTESIAN_POINT('Ctrl Pts',(22.5194011826095,-50.8030095154242,-32.1635995572792));
#19086=CARTESIAN_POINT('Ctrl Pts',(22.5214654524887,-49.9995340141484,-32.112583302492));
#19087=CARTESIAN_POINT('Ctrl Pts',(22.5184387847934,-50.0021533196134,-32.387416697508));
#19088=CARTESIAN_POINT('Ctrl Pts',(22.5199144628852,-50.1656954401332,-32.3977680939259));
#19089=CARTESIAN_POINT('Ctrl Pts',(22.5053315607811,-50.3289756387791,-32.4081194903437));
#19090=CARTESIAN_POINT('Ctrl Pts',(22.4737267531911,-50.4888917355071,-32.4184708867615));
#19091=CARTESIAN_POINT('Ctrl Pts',(22.3129776625007,-51.3022606213186,-32.4711203944923));
#19092=CARTESIAN_POINT('Ctrl Pts',(21.7118776363753,-52.0286013287837,-32.5237699022232));
#19093=CARTESIAN_POINT('Ctrl Pts',(20.9429262308432,-52.3386383435,-32.576419409954));
#19094=CARTESIAN_POINT('Ctrl Pts',(20.1739748253111,-52.6486753582164,-32.6290689176848));
#19095=CARTESIAN_POINT('Ctrl Pts',(19.2371720403724,-52.542408680184,-32.6817184254156));
#19096=CARTESIAN_POINT('Ctrl Pts',(18.5572031727947,-52.0680126919115,-32.7343679331465));
#19097=CARTESIAN_POINT('Ctrl Pts',(17.877234305217,-51.5936167036389,-32.7870174408773));
#19098=CARTESIAN_POINT('Ctrl Pts',(17.4540993550003,-50.7510914051262,-32.8396669486081));
#19099=CARTESIAN_POINT('Ctrl Pts',(17.4796201172914,-49.9223828283297,-32.8923164563389));
#19100=CARTESIAN_POINT('Ctrl Pts',(17.5051408795824,-49.0936742515332,-32.9449659640697));
#19101=CARTESIAN_POINT('Ctrl Pts',(17.9793173543814,-48.2787823964529,-32.9976154718006));
#19102=CARTESIAN_POINT('Ctrl Pts',(18.6871888475508,-47.8471260936818,-33.0502649795314));
#19103=CARTESIAN_POINT('Ctrl Pts',(19.3950603407203,-47.4154697909107,-33.1029144872622));
#19104=CARTESIAN_POINT('Ctrl Pts',(20.3366268522603,-47.3670490404488,-33.155563994993));
#19105=CARTESIAN_POINT('Ctrl Pts',(21.0850435223897,-47.7238146531926,-33.2082135027239));
#19106=CARTESIAN_POINT('Ctrl Pts',(21.833460192519,-48.0805802659364,-33.2608630104547));
#19107=CARTESIAN_POINT('Ctrl Pts',(22.3887270212377,-48.842532241886,-33.3135125181855));
#19108=CARTESIAN_POINT('Ctrl Pts',(22.4991222355848,-49.6642512396056,-33.3661620259163));
#19109=CARTESIAN_POINT('Ctrl Pts',(22.5139777972501,-49.7748275658933,-33.3732469164469));
#19110=CARTESIAN_POINT('Ctrl Pts',(22.5207774906703,-49.8864861712863,-33.3803318069775));
#19111=CARTESIAN_POINT('Ctrl Pts',(22.5198908044257,-49.9982532979407,-33.387416697508));
#19112=CARTESIAN_POINT('Origin',(20.,-50.,-32.));
#19113=CARTESIAN_POINT('',(22.5135831830112,-49.9995432846514,-34.387416697508));
#19114=CARTESIAN_POINT('',(22.5158015821966,-50.0020603006293,-34.112583302492));
#19115=CARTESIAN_POINT('',(22.5175,-50.,-32.));
#19116=CARTESIAN_POINT('Ctrl Pts',(22.5158015821966,-50.0020603006293,-34.112583302492));
#19117=CARTESIAN_POINT('Ctrl Pts',(22.5112691112874,-49.4237577609146,-34.0760774756515));
#19118=CARTESIAN_POINT('Ctrl Pts',(22.3128671172368,-48.8426454482035,-34.0395716488111));
#19119=CARTESIAN_POINT('Ctrl Pts',(21.9477708045538,-48.3985855494889,-34.0030658219707));
#19120=CARTESIAN_POINT('Ctrl Pts',(21.4212208589487,-47.7581525804585,-33.9504163142399));
#19121=CARTESIAN_POINT('Ctrl Pts',(20.5479459993279,-47.4027892337671,-33.897766806509));
#19122=CARTESIAN_POINT('Ctrl Pts',(19.7238321035734,-47.4935940786933,-33.8451172987782));
#19123=CARTESIAN_POINT('Ctrl Pts',(18.8997182078189,-47.5843989236195,-33.7924677910474));
#19124=CARTESIAN_POINT('Ctrl Pts',(18.1247652759306,-48.1213719601635,-33.7398182833166));
#19125=CARTESIAN_POINT('Ctrl Pts',(17.7502864350161,-48.8610846278562,-33.6871687755858));
#19126=CARTESIAN_POINT('Ctrl Pts',(17.3758075941016,-49.600797295549,-33.6345192678549));
#19127=CARTESIAN_POINT('Ctrl Pts',(17.4018028441609,-50.5432495943906,-33.5818697601241));
#19128=CARTESIAN_POINT('Ctrl Pts',(17.8164876338846,-51.2611951063967,-33.5292202523933));
#19129=CARTESIAN_POINT('Ctrl Pts',(18.2311724236082,-51.9791406184027,-33.4765707446625));
#19130=CARTESIAN_POINT('Ctrl Pts',(19.0345467529961,-52.4725793435733,-33.4239212369316));
#19131=CARTESIAN_POINT('Ctrl Pts',(19.8624130865832,-52.5178183394824,-33.3712717292008));
#19132=CARTESIAN_POINT('Ctrl Pts',(20.6902794201703,-52.5630573353916,-33.31862222147));
#19133=CARTESIAN_POINT('Ctrl Pts',(21.5426377579565,-52.1600966020395,-33.2659727137392));
#19134=CARTESIAN_POINT('Ctrl Pts',(22.03308440916,-51.4916122601428,-33.2133232060084));
#19135=CARTESIAN_POINT('Ctrl Pts',(22.3458923248248,-51.0652515272677,-33.1797432381696));
#19136=CARTESIAN_POINT('Ctrl Pts',(22.5114776249371,-50.5308780344015,-33.1461632703308));
#19137=CARTESIAN_POINT('Ctrl Pts',(22.5147221745587,-49.9983487241263,-33.112583302492));
#19138=CARTESIAN_POINT('Ctrl Pts',(22.5198908044257,-49.9982532979407,-33.387416697508));
#19139=CARTESIAN_POINT('Ctrl Pts',(22.5141883141564,-50.7170542899409,-33.4329813147083));
#19140=CARTESIAN_POINT('Ctrl Pts',(22.1905708411972,-51.4403438105407,-33.4785459319085));
#19141=CARTESIAN_POINT('Ctrl Pts',(21.6473228251422,-51.9091010157313,-33.5241105491088));
#19142=CARTESIAN_POINT('Ctrl Pts',(21.0196046003771,-52.4507457746479,-33.5767600568396));
#19143=CARTESIAN_POINT('Ctrl Pts',(20.0986445508716,-52.6525492729915,-33.6294095645704));
#19144=CARTESIAN_POINT('Ctrl Pts',(19.3019459102021,-52.4230269635761,-33.6820590723013));
#19145=CARTESIAN_POINT('Ctrl Pts',(18.5052472695326,-52.1935046541608,-33.7347085800321));
#19146=CARTESIAN_POINT('Ctrl Pts',(17.8328100376991,-51.5326565369863,-33.7873580877629));
#19147=CARTESIAN_POINT('Ctrl Pts',(17.5894734081264,-50.7400680565804,-33.8400075954937));
#19148=CARTESIAN_POINT('Ctrl Pts',(17.3461367785536,-49.9474795761745,-33.8926571032246));
#19149=CARTESIAN_POINT('Ctrl Pts',(17.5319007512416,-49.0231507325371,-33.9453066109554));
#19150=CARTESIAN_POINT('Ctrl Pts',(18.0625520540502,-48.3861119508357,-33.9979561186862));
#19151=CARTESIAN_POINT('Ctrl Pts',(18.5932033568587,-47.7490731691343,-34.050605626417));
#19152=CARTESIAN_POINT('Ctrl Pts',(19.4687419897878,-47.399324449369,-34.1032551341478));
#19153=CARTESIAN_POINT('Ctrl Pts',(20.292255827751,-47.495419055082,-34.1559046418787));
#19154=CARTESIAN_POINT('Ctrl Pts',(21.1157696657142,-47.5915136607951,-34.2085541496095));
#19155=CARTESIAN_POINT('Ctrl Pts',(21.8872587087114,-48.1334515919866,-34.2612036573403));
#19156=CARTESIAN_POINT('Ctrl Pts',(22.2569801309892,-48.8755535286994,-34.3138531650711));
#19157=CARTESIAN_POINT('Ctrl Pts',(22.4291755608078,-49.2211828438043,-34.3383743425501));
#19158=CARTESIAN_POINT('Ctrl Pts',(22.5142206789451,-49.610231176692,-34.3628955200291));
#19159=CARTESIAN_POINT('Ctrl Pts',(22.5135831830112,-49.9995432846514,-34.387416697508));
#19160=CARTESIAN_POINT('Origin',(20.,-50.,-32.));
#19161=CARTESIAN_POINT('',(22.5182788973074,-50.0021768080843,-35.387416697508));
#19162=CARTESIAN_POINT('',(22.5215055099484,-49.9996299858508,-35.112583302492));
#19163=CARTESIAN_POINT('',(22.5175,-50.,-32.));
#19164=CARTESIAN_POINT('Ctrl Pts',(22.5215055099484,-49.9996299858508,-35.112583302492));
#19165=CARTESIAN_POINT('Ctrl Pts',(22.5215476822769,-49.9792730825142,-35.111290696434));
#19166=CARTESIAN_POINT('Ctrl Pts',(22.5213222503032,-49.9589171368633,-35.109998090376));
#19167=CARTESIAN_POINT('Ctrl Pts',(22.520826339132,-49.9385677827562,-35.108705484318));
#19168=CARTESIAN_POINT('Ctrl Pts',(22.5006272391188,-49.1097124097289,-35.0560559765872));
#19169=CARTESIAN_POINT('Ctrl Pts',(22.0316929523784,-48.291792656124,-35.0034064688563));
#19170=CARTESIAN_POINT('Ctrl Pts',(21.3266077068082,-47.8556000042866,-34.9507569611255));
#19171=CARTESIAN_POINT('Ctrl Pts',(20.621522461238,-47.4194073524491,-34.8981074533947));
#19172=CARTESIAN_POINT('Ctrl Pts',(19.680286256838,-47.3649418023791,-34.8454579456639));
#19173=CARTESIAN_POINT('Ctrl Pts',(18.9295942136707,-47.716894482953,-34.792808437933));
#19174=CARTESIAN_POINT('Ctrl Pts',(18.1789021705034,-48.0688471635269,-34.7401589302022));
#19175=CARTESIAN_POINT('Ctrl Pts',(17.6187542885687,-48.8272180747446,-34.6875094224714));
#19176=CARTESIAN_POINT('Ctrl Pts',(17.5030850920777,-49.6482112964103,-34.6348599147406));
#19177=CARTESIAN_POINT('Ctrl Pts',(17.3874158955868,-50.4692045180759,-34.5822104070097));
#19178=CARTESIAN_POINT('Ctrl Pts',(17.7162253845396,-51.3528200501893,-34.5295608992789));
#19179=CARTESIAN_POINT('Ctrl Pts',(18.3404527772637,-51.8984842282426,-34.4769113915481));
#19180=CARTESIAN_POINT('Ctrl Pts',(18.9646801699878,-52.444148406296,-34.4242618838173));
#19181=CARTESIAN_POINT('Ctrl Pts',(19.8843254664833,-52.6518612302893,-34.3716123760864));
#19182=CARTESIAN_POINT('Ctrl Pts',(20.6824814564575,-52.4274592501151,-34.3189628683556));
#19183=CARTESIAN_POINT('Ctrl Pts',(21.4806374464317,-52.203057269941,-34.2663133606248));
#19184=CARTESIAN_POINT('Ctrl Pts',(22.1573041298847,-51.5465404855995,-34.213663852894));
#19185=CARTESIAN_POINT('Ctrl Pts',(22.4057249558165,-50.755530797744,-34.1610143451632));
#19186=CARTESIAN_POINT('Ctrl Pts',(22.4818971122757,-50.5129870678532,-34.1448706642728));
#19187=CARTESIAN_POINT('Ctrl Pts',(22.5178059406877,-50.2577984243011,-34.1287269833824));
#19188=CARTESIAN_POINT('Ctrl Pts',(22.5158015821966,-50.0020603006293,-34.112583302492));
#19189=CARTESIAN_POINT('Ctrl Pts',(22.5135831830112,-49.9995432846514,-34.387416697508));
#19190=CARTESIAN_POINT('Ctrl Pts',(22.512851909149,-50.4461245939351,-34.4155450277599));
#19191=CARTESIAN_POINT('Ctrl Pts',(22.3993754586544,-50.8930529907507,-34.4436733580118));
#19192=CARTESIAN_POINT('Ctrl Pts',(22.1753691924073,-51.2751894193514,-34.4718016882636));
#19193=CARTESIAN_POINT('Ctrl Pts',(21.7560830299892,-51.9904574310566,-34.5244511959944));
#19194=CARTESIAN_POINT('Ctrl Pts',(20.9495569035946,-52.4787275122331,-34.5771007037253));
#19195=CARTESIAN_POINT('Ctrl Pts',(20.1214171679329,-52.5186498466107,-34.6297502114561));
#19196=CARTESIAN_POINT('Ctrl Pts',(19.2932774322712,-52.5585721809883,-34.6823997191869));
#19197=CARTESIAN_POINT('Ctrl Pts',(18.4435240873424,-52.150146768567,-34.7350492269177));
#19198=CARTESIAN_POINT('Ctrl Pts',(17.95737989003,-51.4785270592201,-34.7876987346485));
#19199=CARTESIAN_POINT('Ctrl Pts',(17.4712356927177,-50.8069073498732,-34.8403482423793));
#19200=CARTESIAN_POINT('Ctrl Pts',(17.3487006430217,-49.8720933436008,-34.8929977501102));
#19201=CARTESIAN_POINT('Ctrl Pts',(17.6453241423544,-49.0978687546033,-34.945647257841));
#19202=CARTESIAN_POINT('Ctrl Pts',(17.9419476416872,-48.3236441656058,-34.9982967655718));
#19203=CARTESIAN_POINT('Ctrl Pts',(18.6577296900485,-47.7100089938833,-35.0509462733026));
#19204=CARTESIAN_POINT('Ctrl Pts',(19.4681813805772,-47.5351454131044,-35.1035957810335));
#19205=CARTESIAN_POINT('Ctrl Pts',(20.2786330711059,-47.3602818323255,-35.1562452887643));
#19206=CARTESIAN_POINT('Ctrl Pts',(21.1837544038018,-47.6241898424903,-35.2088947964951));
#19207=CARTESIAN_POINT('Ctrl Pts',(21.7732223864982,-48.2072307603836,-35.2615443042259));
#19208=CARTESIAN_POINT('Ctrl Pts',(22.2429814209321,-48.6718679360485,-35.3035017686533));
#19209=CARTESIAN_POINT('Ctrl Pts',(22.512274677717,-49.3391806940296,-35.3454592330807));
#19210=CARTESIAN_POINT('Ctrl Pts',(22.5182788973074,-50.0021768080843,-35.387416697508));
#19211=CARTESIAN_POINT('Origin',(20.,-50.,-32.));
#19212=CARTESIAN_POINT('',(22.5200281316337,-49.9983136770239,-36.387416697508));
#19213=CARTESIAN_POINT('',(22.514833600647,-49.998290627205,-36.112583302492));
#19214=CARTESIAN_POINT('',(22.5175,-50.,-32.));
#19215=CARTESIAN_POINT('Ctrl Pts',(22.514833600647,-49.998290627205,-36.112583302492));
#19216=CARTESIAN_POINT('Ctrl Pts',(22.5167122753364,-49.701310816587,-36.0938544094856));
#19217=CARTESIAN_POINT('Ctrl Pts',(22.4680383940606,-49.4049267668115,-36.0751255164792));
#19218=CARTESIAN_POINT('Ctrl Pts',(22.3660666542655,-49.1281812476854,-36.0563966234728));
#19219=CARTESIAN_POINT('Ctrl Pts',(22.0794099949087,-48.3502113300977,-36.003747115742));
#19220=CARTESIAN_POINT('Ctrl Pts',(21.3715670977831,-47.7274348681072,-35.9510976080111));
#19221=CARTESIAN_POINT('Ctrl Pts',(20.5634277762338,-47.5421781003539,-35.8984481002803));
#19222=CARTESIAN_POINT('Ctrl Pts',(19.7552884546845,-47.3569213326006,-35.8457985925495));
#19223=CARTESIAN_POINT('Ctrl Pts',(18.8468527087114,-47.6091842590845,-35.7931490848187));
#19224=CARTESIAN_POINT('Ctrl Pts',(18.2499460693557,-48.1846073181783,-35.7404995770878));
#19225=CARTESIAN_POINT('Ctrl Pts',(17.6530394299999,-48.7600303772722,-35.687850069357));
#19226=CARTESIAN_POINT('Ctrl Pts',(17.3676618972616,-49.658613568976,-35.6352005616262));
#19227=CARTESIAN_POINT('Ctrl Pts',(17.5231850359167,-50.4729978679274,-35.5825510538954));
#19228=CARTESIAN_POINT('Ctrl Pts',(17.6787081745718,-51.2873821668789,-35.5299015461646));
#19229=CARTESIAN_POINT('Ctrl Pts',(18.2751319846203,-52.017567573078,-35.4772520384337));
#19230=CARTESIAN_POINT('Ctrl Pts',(19.0420768014859,-52.3325356364118,-35.4246025307029));
#19231=CARTESIAN_POINT('Ctrl Pts',(19.8090216183516,-52.6475036997456,-35.3719530229721));
#19232=CARTESIAN_POINT('Ctrl Pts',(20.7464874420344,-52.5472544202141,-35.3193035152413));
#19233=CARTESIAN_POINT('Ctrl Pts',(21.4294883972328,-52.0772342842236,-35.2666540075104));
#19234=CARTESIAN_POINT('Ctrl Pts',(22.095720892281,-51.6187536839543,-35.2152971058376));
#19235=CARTESIAN_POINT('Ctrl Pts',(22.5198299490833,-50.8084359453709,-35.1639402041648));
#19236=CARTESIAN_POINT('Ctrl Pts',(22.5215055099484,-49.9996299858508,-35.112583302492));
#19237=CARTESIAN_POINT('Ctrl Pts',(22.5182788973074,-50.0021768080843,-35.387416697508));
#19238=CARTESIAN_POINT('Ctrl Pts',(22.519808955826,-50.171128465632,-35.3981087408115));
#19239=CARTESIAN_POINT('Ctrl Pts',(22.5042413918334,-50.3397998063493,-35.408800784115));
#19240=CARTESIAN_POINT('Ctrl Pts',(22.4705365847028,-50.5047654526046,-35.4194928274184));
#19241=CARTESIAN_POINT('Ctrl Pts',(22.304568167514,-51.3170854013106,-35.4721423351492));
#19242=CARTESIAN_POINT('Ctrl Pts',(21.6988167004395,-52.0395514731012,-35.5247918428801));
#19243=CARTESIAN_POINT('Ctrl Pts',(20.9278903995302,-52.3446446607096,-35.5774413506109));
#19244=CARTESIAN_POINT('Ctrl Pts',(20.1569640986209,-52.6497378483181,-35.6300908583417));
#19245=CARTESIAN_POINT('Ctrl Pts',(19.2208629638768,-52.5374581517444,-35.6827403660725));
#19246=CARTESIAN_POINT('Ctrl Pts',(18.5439542096161,-52.0587058640667,-35.7353898738034));
#19247=CARTESIAN_POINT('Ctrl Pts',(17.8670454553555,-51.579953576389,-35.7880393815342));
#19248=CARTESIAN_POINT('Ctrl Pts',(17.4493290815783,-50.7347286976071,-35.840688889265));
#19249=CARTESIAN_POINT('Ctrl Pts',(17.4801704542087,-49.9062010732358,-35.8933383969958));
#19250=CARTESIAN_POINT('Ctrl Pts',(17.5110118268392,-49.0776734488645,-35.9459879047266));
#19251=CARTESIAN_POINT('Ctrl Pts',(17.9904109458772,-48.2658430789037,-35.9986374124575));
#19252=CARTESIAN_POINT('Ctrl Pts',(18.7010395108258,-47.8387409164315,-36.0512869201883));
#19253=CARTESIAN_POINT('Ctrl Pts',(19.4116680757745,-47.4116387539593,-36.1039364279191));
#19254=CARTESIAN_POINT('Ctrl Pts',(20.3535260866337,-47.3692647989758,-36.1565859356499));
#19255=CARTESIAN_POINT('Ctrl Pts',(21.099636536866,-47.7308286391844,-36.2092354433808));
#19256=CARTESIAN_POINT('Ctrl Pts',(21.8457469870983,-48.092392479393,-36.2618849511116));
#19257=CARTESIAN_POINT('Ctrl Pts',(22.3961098767036,-48.8578941147936,-36.3145344588424));
#19258=CARTESIAN_POINT('Ctrl Pts',(22.5012265588905,-49.6803050206447,-36.3671839665732));
#19259=CARTESIAN_POINT('Ctrl Pts',(22.5146916898361,-49.7856533850333,-36.3739282102182));
#19260=CARTESIAN_POINT('Ctrl Pts',(22.5208508471277,-49.8919355645194,-36.3806724538631));
#19261=CARTESIAN_POINT('Ctrl Pts',(22.5200281316337,-49.9983136770239,-36.387416697508));
#19262=CARTESIAN_POINT('Origin',(20.,-50.,-32.));
#19263=CARTESIAN_POINT('',(22.5136154336298,-49.9994585736035,-37.387416697508));
#19264=CARTESIAN_POINT('',(22.5156629463979,-50.0020238415623,-37.112583302492));
#19265=CARTESIAN_POINT('',(22.5175,-50.,-32.));
#19266=CARTESIAN_POINT('Ctrl Pts',(22.5156629463979,-50.0020238415623,-37.112583302492));
#19267=CARTESIAN_POINT('Ctrl Pts',(22.5112698172375,-49.4290377137389,-37.0764181225372));
#19268=CARTESIAN_POINT('Ctrl Pts',(22.3168706622171,-48.8533547764504,-37.0402529425824));
#19269=CARTESIAN_POINT('Ctrl Pts',(21.9580133306554,-48.4111251962995,-37.0040877626276));
#19270=CARTESIAN_POINT('Ctrl Pts',(21.4355864582898,-47.7673244540371,-36.9514382548968));
#19271=CARTESIAN_POINT('Ctrl Pts',(20.5646113896891,-47.4063611351857,-36.898788747166));
#19272=CARTESIAN_POINT('Ctrl Pts',(19.7399314254149,-47.4918724738244,-36.8461392394351));
#19273=CARTESIAN_POINT('Ctrl Pts',(18.9152514611408,-47.5773838124631,-36.7934897317043));
#19274=CARTESIAN_POINT('Ctrl Pts',(18.1368666011931,-48.1093698085918,-36.7408402239735));
#19275=CARTESIAN_POINT('Ctrl Pts',(17.7576457860981,-48.8466626993815,-36.6881907162427));
#19276=CARTESIAN_POINT('Ctrl Pts',(17.378424971003,-49.5839555901713,-36.6355412085118));
#19277=CARTESIAN_POINT('Ctrl Pts',(17.3983682007606,-50.5265553756219,-36.582891700781));
#19278=CARTESIAN_POINT('Ctrl Pts',(17.8084345149201,-51.2471487775885,-36.5302421930502));
#19279=CARTESIAN_POINT('Ctrl Pts',(18.2185008290795,-51.967742179555,-36.4775926853194));
#19280=CARTESIAN_POINT('Ctrl Pts',(19.0186902276409,-52.4663291980374,-36.4249431775885));
#19281=CARTESIAN_POINT('Ctrl Pts',(19.8462490153544,-52.5168829897992,-36.3722936698577));
#19282=CARTESIAN_POINT('Ctrl Pts',(20.6738078030678,-52.567436781561,-36.3196441621269));
#19283=CARTESIAN_POINT('Ctrl Pts',(21.5287359799332,-52.1699573466022,-36.2669946543961));
#19284=CARTESIAN_POINT('Ctrl Pts',(22.0234648575718,-51.5046359425303,-36.2143451466652));
#19285=CARTESIAN_POINT('Ctrl Pts',(22.3422049251376,-51.0759878508744,-36.1804245319408));
#19286=CARTESIAN_POINT('Ctrl Pts',(22.5114310610355,-50.5361621251873,-36.1465039172164));
#19287=CARTESIAN_POINT('Ctrl Pts',(22.514833600647,-49.998290627205,-36.112583302492));
#19288=CARTESIAN_POINT('Ctrl Pts',(22.5200281316337,-49.9983136770239,-36.387416697508));
#19289=CARTESIAN_POINT('Ctrl Pts',(22.5144282491257,-50.7223852860246,-36.4333219615939));
#19290=CARTESIAN_POINT('Ctrl Pts',(22.1853610476112,-51.450901432647,-36.4792272256798));
#19291=CARTESIAN_POINT('Ctrl Pts',(21.6350305312817,-51.919639117633,-36.5251324897657));
#19292=CARTESIAN_POINT('Ctrl Pts',(21.0038473467175,-52.4572421324687,-36.5777819974965));
#19293=CARTESIAN_POINT('Ctrl Pts',(20.0816105028205,-52.6531279858382,-36.6304315052274));
#19294=CARTESIAN_POINT('Ctrl Pts',(19.2864020482738,-52.4184948081959,-36.6830810129582));
#19295=CARTESIAN_POINT('Ctrl Pts',(18.491193593727,-52.1838616305535,-36.735730520689));
#19296=CARTESIAN_POINT('Ctrl Pts',(17.8230135285305,-51.5187094218993,-36.7883800284198));
#19297=CARTESIAN_POINT('Ctrl Pts',(17.5847711247798,-50.7245748146517,-36.8410295361506));
#19298=CARTESIAN_POINT('Ctrl Pts',(17.3465287210292,-49.9304402074041,-36.8936790438814));
#19299=CARTESIAN_POINT('Ctrl Pts',(17.5382239787243,-49.0073232015632,-36.9463285516123));
#19300=CARTESIAN_POINT('Ctrl Pts',(18.0729547670113,-48.3737048670602,-36.9989780593431));
#19301=CARTESIAN_POINT('Ctrl Pts',(18.6076855552984,-47.7400865325572,-37.0516275670739));
#19302=CARTESIAN_POINT('Ctrl Pts',(19.4854518741773,-47.395966869392,-37.1042770748048));
#19303=CARTESIAN_POINT('Ctrl Pts',(20.308331712708,-47.4973472680142,-37.1569265825356));
#19304=CARTESIAN_POINT('Ctrl Pts',(21.1312115512386,-47.5987276666363,-37.2095760902664));
#19305=CARTESIAN_POINT('Ctrl Pts',(21.899204909421,-48.1456081270457,-37.2622255979972));
#19306=CARTESIAN_POINT('Ctrl Pts',(22.2641536736782,-48.8900687603565,-37.314875105728));
#19307=CARTESIAN_POINT('Ctrl Pts',(22.431765017819,-49.2319798986588,-37.3390556363213));
#19308=CARTESIAN_POINT('Ctrl Pts',(22.5143612515527,-49.6155670709948,-37.3632361669147));
#19309=CARTESIAN_POINT('Ctrl Pts',(22.5136154336298,-49.9994585736035,-37.387416697508));
#19310=CARTESIAN_POINT('Origin',(20.,-50.,-32.));
#19311=CARTESIAN_POINT('',(22.5181182812424,-50.0021988905331,-38.387416697508));
#19312=CARTESIAN_POINT('',(22.5215368448905,-49.9997267149633,-38.112583302492));
#19313=CARTESIAN_POINT('',(22.5175,-50.,-32.));
#19314=CARTESIAN_POINT('Ctrl Pts',(22.5215368448905,-49.9997267149633,-38.112583302492));
#19315=CARTESIAN_POINT('Ctrl Pts',(22.5215601439286,-49.9847350660108,-38.1116313433196));
#19316=CARTESIAN_POINT('Ctrl Pts',(22.5214378830458,-49.9697438072224,-38.1106793841472));
#19317=CARTESIAN_POINT('Ctrl Pts',(22.5211688994512,-49.9547551815961,-38.1097274249749));
#19318=CARTESIAN_POINT('Ctrl Pts',(22.5062923645566,-49.1257871084977,-38.057077917244));
#19319=CARTESIAN_POINT('Ctrl Pts',(22.0426194655824,-48.3048733682434,-38.0044284095132));
#19320=CARTESIAN_POINT('Ctrl Pts',(21.3403495125323,-47.8641624016026,-37.9517789017824));
#19321=CARTESIAN_POINT('Ctrl Pts',(20.6380795594823,-47.4234514349619,-37.8991293940516));
#19322=CARTESIAN_POINT('Ctrl Pts',(19.6972125523564,-47.3629432419346,-37.8464798863208));
#19323=CARTESIAN_POINT('Ctrl Pts',(18.9442761145565,-47.7100684523628,-37.7938303785899));
#19324=CARTESIAN_POINT('Ctrl Pts',(18.1913396767565,-48.0571936627911,-37.7411808708591));
#19325=CARTESIAN_POINT('Ctrl Pts',(17.6263338082825,-48.8119522766749,-37.6885313631283));
#19326=CARTESIAN_POINT('Ctrl Pts',(17.5053953913003,-49.6321858731847,-37.6358818553975));
#19327=CARTESIAN_POINT('Ctrl Pts',(17.3844569743181,-50.4524194696944,-37.5832323476667));
#19328=CARTESIAN_POINT('Ctrl Pts',(17.7075860088279,-51.3381280488302,-37.5305828399359));
#19329=CARTESIAN_POINT('Ctrl Pts',(18.3282968288376,-51.8877891355766,-37.477933332205));
#19330=CARTESIAN_POINT('Ctrl Pts',(18.9490076488472,-52.437450222323,-37.4252838244742));
#19331=CARTESIAN_POINT('Ctrl Pts',(19.8673002543568,-52.65106381668,-37.3726343167433));
#19332=CARTESIAN_POINT('Ctrl Pts',(20.6668806730142,-52.4317914236705,-37.3199848090125));
#19333=CARTESIAN_POINT('Ctrl Pts',(21.4664610916715,-52.212519030661,-37.2673353012817));
#19334=CARTESIAN_POINT('Ctrl Pts',(22.1473293234767,-51.5603606502849,-37.2146857935509));
#19335=CARTESIAN_POINT('Ctrl Pts',(22.4008241013141,-50.7709623772601,-37.1620362858201));
#19336=CARTESIAN_POINT('Ctrl Pts',(22.4801921939607,-50.523805272869,-37.145551958044));
#19337=CARTESIAN_POINT('Ctrl Pts',(22.5176653636715,-50.263194701322,-37.129067630268));
#19338=CARTESIAN_POINT('Ctrl Pts',(22.5156629463979,-50.0020238415623,-37.112583302492));
#19339=CARTESIAN_POINT('Ctrl Pts',(22.5136154336298,-49.9994585736035,-37.387416697508));
#19340=CARTESIAN_POINT('Ctrl Pts',(22.5127373439902,-50.4514337016458,-37.4158856746455));
#19341=CARTESIAN_POINT('Ctrl Pts',(22.3963341785868,-50.9038306788881,-37.444354651783));
#19342=CARTESIAN_POINT('Ctrl Pts',(22.1671363564595,-51.2891312023377,-37.4728236289205));
#19343=CARTESIAN_POINT('Ctrl Pts',(21.7432661046516,-52.0016922047957,-37.5254731366513));
#19344=CARTESIAN_POINT('Ctrl Pts',(20.9336214307039,-52.4847734034993,-37.5781226443822));
#19345=CARTESIAN_POINT('Ctrl Pts',(20.1052424220535,-52.5193774874071,-37.630772152113));
#19346=CARTESIAN_POINT('Ctrl Pts',(19.2768634134032,-52.5539815713149,-37.6834216598438));
#19347=CARTESIAN_POINT('Ctrl Pts',(18.42975007005,-52.140108540427,-37.7360711675746));
#19348=CARTESIAN_POINT('Ctrl Pts',(17.9479283709528,-51.4653810329258,-37.7887206753054));
#19349=CARTESIAN_POINT('Ctrl Pts',(17.4661066718556,-50.7906535254245,-37.8413701830363));
#19350=CARTESIAN_POINT('Ctrl Pts',(17.3495766170143,-49.85507154131,-37.8940196907671));
#19351=CARTESIAN_POINT('Ctrl Pts',(17.6511652816951,-49.0827677555387,-37.9466691984979));
#19352=CARTESIAN_POINT('Ctrl Pts',(17.9527539463759,-48.3104639697674,-37.9993187062287));
#19353=CARTESIAN_POINT('Ctrl Pts',(18.6724613305789,-47.7014383823393,-38.0519682139595));
#19354=CARTESIAN_POINT('Ctrl Pts',(19.4840191417411,-47.531781869955,-38.1046177216904));
#19355=CARTESIAN_POINT('Ctrl Pts',(20.2955769529033,-47.3621253575708,-38.1572672294212));
#19356=CARTESIAN_POINT('Ctrl Pts',(21.1989851910248,-47.6318379202303,-38.209916737152));
#19357=CARTESIAN_POINT('Ctrl Pts',(21.7846972590492,-48.2186526785622,-38.2625662448828));
#19358=CARTESIAN_POINT('Ctrl Pts',(22.2476735206997,-48.6825005620628,-38.3041830624246));
#19359=CARTESIAN_POINT('Ctrl Pts',(22.5121495212431,-49.3444775845434,-38.3457998799663));
#19360=CARTESIAN_POINT('Ctrl Pts',(22.5181182812424,-50.0021988905331,-38.387416697508));
#19361=CARTESIAN_POINT('Origin',(20.,-50.,-32.));
#19362=CARTESIAN_POINT('',(22.5201577888434,-49.9984351914864,-39.387416697508));
#19363=CARTESIAN_POINT('',(22.514945820706,-49.9982392595312,-39.112583302492));
#19364=CARTESIAN_POINT('',(22.5175,-50.,-32.));
#19365=CARTESIAN_POINT('',(18.086534003335,-48.364012796625,-40.));
#19366=CARTESIAN_POINT('Ctrl Pts',(22.5201577888434,-49.9984351914864,-39.387416697508));
#19367=CARTESIAN_POINT('Ctrl Pts',(22.5146851491745,-50.7276238121977,-39.4336626084795));
#19368=CARTESIAN_POINT('Ctrl Pts',(22.1801327508562,-51.4610373176228,-39.4799085194511));
#19369=CARTESIAN_POINT('Ctrl Pts',(21.6226860724328,-51.9298784151162,-39.5261544304226));
#19370=CARTESIAN_POINT('Ctrl Pts',(20.9880506508656,-52.4636391837647,-39.5788039381534));
#19371=CARTESIAN_POINT('Ctrl Pts',(20.064519663454,-52.6544849370069,-39.6314534458842));
#19372=CARTESIAN_POINT('Ctrl Pts',(19.2708508590834,-52.4142812011169,-39.6841029536151));
#19373=CARTESIAN_POINT('Ctrl Pts',(18.4771820547128,-52.1740774652269,-39.7367524613459));
#19374=CARTESIAN_POINT('Ctrl Pts',(17.813375433383,-51.5028242402046,-39.7894019690767));
#19375=CARTESIAN_POINT('Ctrl Pts',(17.5804145739582,-50.7085548746096,-39.8420514768075));
#19376=CARTESIAN_POINT('Ctrl Pts',(17.3474537145333,-49.9142855090145,-39.8947009845384));
#19377=CARTESIAN_POINT('Ctrl Pts',(17.5453386170133,-48.9970000028465,-39.9473504922692));
#19378=CARTESIAN_POINT('Ctrl Pts',(18.086534003335,-48.364012796625,-40.));
#19379=CARTESIAN_POINT('',(21.9170727734079,-48.3614591747396,-40.));
#19380=CARTESIAN_POINT('Origin',(20.,-50.,-40.));
#19381=CARTESIAN_POINT('Ctrl Pts',(21.917080287283,-48.3614538548662,-40.));
#19382=CARTESIAN_POINT('Ctrl Pts',(21.3942484559038,-47.752683457533,-39.9490537266974));
#19383=CARTESIAN_POINT('Ctrl Pts',(20.5545526583696,-47.4126378392115,-39.8981074533947));
#19384=CARTESIAN_POINT('Ctrl Pts',(19.7559044836509,-47.4904266257446,-39.847161180092));
#19385=CARTESIAN_POINT('Ctrl Pts',(18.9305559248023,-47.5708160448806,-39.7945116723612));
#19386=CARTESIAN_POINT('Ctrl Pts',(18.1490454735931,-48.0974449380489,-39.7418621646304));
#19387=CARTESIAN_POINT('Ctrl Pts',(17.7651665960889,-48.8322009125333,-39.6892126568995));
#19388=CARTESIAN_POINT('Ctrl Pts',(17.3812877185847,-49.5669568870177,-39.6365631491687));
#19389=CARTESIAN_POINT('Ctrl Pts',(17.3950404147854,-50.5098399428182,-39.5839136414379));
#19390=CARTESIAN_POINT('Ctrl Pts',(17.8004370773545,-51.2330949973265,-39.5312641337071));
#19391=CARTESIAN_POINT('Ctrl Pts',(18.2058337399236,-51.9563500518348,-39.4786146259763));
#19392=CARTESIAN_POINT('Ctrl Pts',(19.0028743688612,-52.4599771050508,-39.4259651182454));
#19393=CARTESIAN_POINT('Ctrl Pts',(19.8301087009278,-52.5158217813334,-39.3733156105146));
#19394=CARTESIAN_POINT('Ctrl Pts',(20.6573430329945,-52.5716664576159,-39.3206661027838));
#19395=CARTESIAN_POINT('Ctrl Pts',(21.5147710681904,-52.1797287569649,-39.268016595053));
#19396=CARTESIAN_POINT('Ctrl Pts',(22.01375313092,-51.5176086839439,-39.2153670873222));
#19397=CARTESIAN_POINT('Ctrl Pts',(22.3384618647093,-51.0867391465682,-39.1811058257121));
#19398=CARTESIAN_POINT('Ctrl Pts',(22.5113810821265,-50.5414566856712,-39.1468445641021));
#19399=CARTESIAN_POINT('Ctrl Pts',(22.514945820706,-49.9982392595312,-39.112583302492));
#19400=CARTESIAN_POINT('Origin',(20.,-50.,-42.2084234471774));
#19401=CARTESIAN_POINT('',(23.0782115777579,-49.9991816606551,-25.7915765528225));
#19402=CARTESIAN_POINT('',(23.0685693947188,-49.9996667583212,-25.7084234471775));
#19403=CARTESIAN_POINT('',(23.0735,-49.9999999999998,-42.2084234471774));
#19404=CARTESIAN_POINT('',(19.2062007174672,-52.9692229537457,-25.));
#19405=CARTESIAN_POINT('Ctrl Pts',(23.0685693947188,-49.9996667583212,-25.7084234471775));
#19406=CARTESIAN_POINT('Ctrl Pts',(23.0688873842183,-49.5044898373669,-25.6828803290416));
#19407=CARTESIAN_POINT('Ctrl Pts',(22.7226355830855,-47.989181422973,-25.6046877031749));
#19408=CARTESIAN_POINT('Ctrl Pts',(20.3515249129824,-46.3913842077397,-25.4738455695774));
#19409=CARTESIAN_POINT('Ctrl Pts',(17.1680748931287,-47.7313322718094,-25.315897046385));
#19410=CARTESIAN_POINT('Ctrl Pts',(16.5570912657335,-51.1345436021507,-25.1579485231925));
#19411=CARTESIAN_POINT('Ctrl Pts',(18.2239621276955,-52.7066289013681,-25.0526495077308));
#19412=CARTESIAN_POINT('Ctrl Pts',(19.2062007174672,-52.9692229537457,-25.));
#19413=CARTESIAN_POINT('',(20.7937992825328,-52.9692229537457,-25.));
#19414=CARTESIAN_POINT('Origin',(20.,-50.,-25.));
#19415=CARTESIAN_POINT('Ctrl Pts',(23.0782115777579,-49.9991816606551,-25.7915765528225));
#19416=CARTESIAN_POINT('Ctrl Pts',(23.0783675970752,-49.9546737841192,-25.7892620061076));
#19417=CARTESIAN_POINT('Ctrl Pts',(23.0574070137277,-48.8978876848609,-25.7342979516619));
#19418=CARTESIAN_POINT('Ctrl Pts',(21.8481507499307,-46.8799263624337,-25.6266843894854));
#19419=CARTESIAN_POINT('Ctrl Pts',(18.3975850974581,-46.7464741037567,-25.4687358662929));
#19420=CARTESIAN_POINT('Ctrl Pts',(16.3999441875489,-49.5638694433452,-25.3107873431005));
#19421=CARTESIAN_POINT('Ctrl Pts',(17.6525826922257,-52.7401247181454,-25.1545420543361));
#19422=CARTESIAN_POINT('Ctrl Pts',(19.8486501161164,-53.2252254607868,-25.0509462733027));
#19423=CARTESIAN_POINT('Ctrl Pts',(20.7956660331737,-52.9742969611506,-25.));
#19424=CARTESIAN_POINT('Origin',(20.,-50.,-42.2084234471774));
#19425=CARTESIAN_POINT('',(23.0698521513658,-49.9981345322115,-26.7915765528225));
#19426=CARTESIAN_POINT('',(23.0750332840076,-50.0025583317598,-26.7084234471774));
#19427=CARTESIAN_POINT('',(23.0735,-49.9999999999998,-42.2084234471774));
#19428=CARTESIAN_POINT('Ctrl Pts',(23.0750332840076,-50.0025583317598,-26.7084234471774));
#19429=CARTESIAN_POINT('Ctrl Pts',(23.0676453720462,-49.1738259322011,-26.6654440420932));
#19430=CARTESIAN_POINT('Ctrl Pts',(22.2960105484609,-47.3177698442431,-26.5698151292781));
#19431=CARTESIAN_POINT('Ctrl Pts',(19.1670202093295,-46.4705001000209,-26.4215367087323));
#19432=CARTESIAN_POINT('Ctrl Pts',(16.5891690739128,-48.7680163387323,-26.2635881855397));
#19433=CARTESIAN_POINT('Ctrl Pts',(17.1038912274563,-52.1826318884526,-26.1056396623473));
#19434=CARTESIAN_POINT('Ctrl Pts',(20.2442745697777,-53.6181279774832,-25.9476911391548));
#19435=CARTESIAN_POINT('Ctrl Pts',(22.6913964149601,-52.0718621316644,-25.8152857340982));
#19436=CARTESIAN_POINT('Ctrl Pts',(23.0682319438559,-50.5251491393848,-25.7355298367724));
#19437=CARTESIAN_POINT('Ctrl Pts',(23.0685693947188,-49.9996667583212,-25.7084234471775));
#19438=CARTESIAN_POINT('Ctrl Pts',(23.0698521513658,-49.9981345322115,-26.7915765528225));
#19439=CARTESIAN_POINT('Ctrl Pts',(23.0719962440276,-49.6156589519614,-26.7718257191592));
#19440=CARTESIAN_POINT('Ctrl Pts',(22.8290065354064,-48.2162500148277,-26.6994253777651));
#19441=CARTESIAN_POINT('Ctrl Pts',(20.7420732792926,-46.4502604182672,-26.5743755286402));
#19442=CARTESIAN_POINT('Ctrl Pts',(17.4332844917096,-47.4380994344961,-26.4164270054477));
#19443=CARTESIAN_POINT('Ctrl Pts',(16.4516596187905,-50.7487514207967,-26.2584784822553));
#19444=CARTESIAN_POINT('Ctrl Pts',(18.6872050080179,-53.3805021188932,-26.1005299590628));
#19445=CARTESIAN_POINT('Ctrl Pts',(22.0628244523097,-52.9536641922363,-25.9448959825852));
#19446=CARTESIAN_POINT('Ctrl Pts',(23.0748185910436,-50.9671043281552,-25.8419115138385));
#19447=CARTESIAN_POINT('Ctrl Pts',(23.0782115777579,-49.9991816606551,-25.7915765528225));
#19448=CARTESIAN_POINT('Origin',(20.,-50.,-42.2084234471774));
#19449=CARTESIAN_POINT('',(23.0717753507574,-50.0025926098673,-27.7915765528225));
#19450=CARTESIAN_POINT('',(23.0760711510323,-49.9977320015118,-27.7084234471775));
#19451=CARTESIAN_POINT('',(23.0735,-49.9999999999998,-42.2084234471774));
#19452=CARTESIAN_POINT('Ctrl Pts',(23.0760711510323,-49.9977320015118,-27.7084234471775));
#19453=CARTESIAN_POINT('Ctrl Pts',(23.0773102483044,-49.8481151574663,-27.7006572628756));
#19454=CARTESIAN_POINT('Ctrl Pts',(22.9996488588235,-48.6854877487299,-27.640241570843));
#19455=CARTESIAN_POINT('Ctrl Pts',(21.5183205224596,-46.7066670244563,-27.5271763710795));
#19456=CARTESIAN_POINT('Ctrl Pts',(18.0723367598354,-46.9282820340933,-27.369227847887));
#19457=CARTESIAN_POINT('Ctrl Pts',(16.3741060118888,-49.934929517492,-27.2112793246946));
#19458=CARTESIAN_POINT('Ctrl Pts',(17.963364296689,-53.000575988945,-27.053330801502));
#19459=CARTESIAN_POINT('Ctrl Pts',(21.3991757827366,-53.3456883625643,-26.8953822783096));
#19460=CARTESIAN_POINT('Ctrl Pts',(22.9766776415497,-51.388891073304,-26.7804131602014));
#19461=CARTESIAN_POINT('Ctrl Pts',(23.0766955189053,-50.1890180408823,-26.718093549824));
#19462=CARTESIAN_POINT('Ctrl Pts',(23.0750332840076,-50.0025583317598,-26.7084234471774));
#19463=CARTESIAN_POINT('Ctrl Pts',(23.0717753507574,-50.0025926098673,-27.7915765528225));
#19464=CARTESIAN_POINT('Ctrl Pts',(23.0659160187279,-49.2836003637029,-27.7543894322108));
#19465=CARTESIAN_POINT('Ctrl Pts',(22.4567168752833,-47.537712359323,-27.6645528038683));
#19466=CARTESIAN_POINT('Ctrl Pts',(19.556563602243,-46.4007357563187,-27.522066667795));
#19467=CARTESIAN_POINT('Ctrl Pts',(16.7437402241732,-48.4037194119704,-27.3641181446025));
#19468=CARTESIAN_POINT('Ctrl Pts',(16.883268566659,-51.8540023792524,-27.2061696214101));
#19469=CARTESIAN_POINT('Ctrl Pts',(19.8486424758461,-53.6233172761733,-27.0482210982176));
#19470=CARTESIAN_POINT('Ctrl Pts',(22.5632792878361,-52.2970308067085,-26.9100234086884));
#19471=CARTESIAN_POINT('Ctrl Pts',(23.0662807676534,-50.6352184987896,-26.8244752268901));
#19472=CARTESIAN_POINT('Ctrl Pts',(23.0698521513658,-49.9981345322115,-26.7915765528225));
#19473=CARTESIAN_POINT('Origin',(20.,-50.,-42.2084234471774));
#19474=CARTESIAN_POINT('',(23.0782820034225,-49.9993152063967,-28.7915765528225));
#19475=CARTESIAN_POINT('',(23.0686596177156,-49.9996515905093,-28.7084234471774));
#19476=CARTESIAN_POINT('',(23.0735,-49.9999999999998,-42.2084234471774));
#19477=CARTESIAN_POINT('Ctrl Pts',(23.0686596177156,-49.9996515905092,-28.7084234471774));
#19478=CARTESIAN_POINT('Ctrl Pts',(23.0691589034913,-49.5111295556534,-28.6832209759272));
#19479=CARTESIAN_POINT('Ctrl Pts',(22.7295044338491,-48.0027108479738,-28.6053689969462));
#19480=CARTESIAN_POINT('Ctrl Pts',(20.3740253245205,-46.3928620895824,-28.4748675102343));
#19481=CARTESIAN_POINT('Ctrl Pts',(17.1840251210985,-47.7149126304983,-28.3169189870418));
#19482=CARTESIAN_POINT('Ctrl Pts',(16.5471836864498,-51.1087823789649,-28.1589704638494));
#19483=CARTESIAN_POINT('Ctrl Pts',(19.0409058103903,-53.4973528915733,-28.0010219406569));
#19484=CARTESIAN_POINT('Ctrl Pts',(22.2388388670651,-52.7534484207361,-27.8508396017662));
#19485=CARTESIAN_POINT('Ctrl Pts',(23.0689100019457,-50.8624167605561,-27.7533067706064));
#19486=CARTESIAN_POINT('Ctrl Pts',(23.0760711510323,-49.9977320015118,-27.7084234471775));
#19487=CARTESIAN_POINT('Ctrl Pts',(23.0782820034225,-49.9993152063967,-28.7915765528225));
#19488=CARTESIAN_POINT('Ctrl Pts',(23.078397645158,-49.9613596528921,-28.7896026529933));
#19489=CARTESIAN_POINT('Ctrl Pts',(23.060634048498,-48.9111325473444,-28.7349792454332));
#19490=CARTESIAN_POINT('Ctrl Pts',(21.8681385615409,-46.8917211343748,-28.6277063301423));
#19491=CARTESIAN_POINT('Ctrl Pts',(18.4185250934885,-46.7365238921992,-28.4697578069498));
#19492=CARTESIAN_POINT('Ctrl Pts',(16.4027868246521,-49.5402211808024,-28.3118092837573));
#19493=CARTESIAN_POINT('Ctrl Pts',(17.648532337875,-52.7607859452632,-28.1538607605649));
#19494=CARTESIAN_POINT('Ctrl Pts',(21.0262820631638,-53.4782300506355,-27.9959122373724));
#19495=CARTESIAN_POINT('Ctrl Pts',(22.8973566155764,-51.6156342685664,-27.8751508347916));
#19496=CARTESIAN_POINT('Ctrl Pts',(23.0742116582373,-50.3015492449329,-27.8070389399417));
#19497=CARTESIAN_POINT('Ctrl Pts',(23.0717753507574,-50.0025926098673,-27.7915765528225));
#19498=CARTESIAN_POINT('Origin',(20.,-50.,-42.2084234471774));
#19499=CARTESIAN_POINT('',(23.0699777810384,-49.9980579821568,-29.7915765528225));
#19500=CARTESIAN_POINT('',(23.0748402987193,-50.0025957432343,-29.7084234471774));
#19501=CARTESIAN_POINT('',(23.0735,-49.9999999999998,-42.2084234471774));
#19502=CARTESIAN_POINT('Ctrl Pts',(23.0748402987193,-50.0025957432343,-29.7084234471774));
#19503=CARTESIAN_POINT('Ctrl Pts',(23.0674595627731,-49.1802997198265,-29.6657846889788));
#19504=CARTESIAN_POINT('Ctrl Pts',(22.3060144165507,-47.3305807981947,-29.5704964230494));
#19505=CARTESIAN_POINT('Ctrl Pts',(19.1896896511183,-46.4652106179844,-29.4225586493891));
#19506=CARTESIAN_POINT('Ctrl Pts',(16.5971711425799,-48.7461680323328,-29.2646101261967));
#19507=CARTESIAN_POINT('Ctrl Pts',(17.0898940665435,-52.1639367579875,-29.1066616030041));
#19508=CARTESIAN_POINT('Ctrl Pts',(20.2211215338182,-53.6197298387387,-28.9487130798117));
#19509=CARTESIAN_POINT('Ctrl Pts',(22.6842316286424,-52.0849997853531,-28.8159670278695));
#19510=CARTESIAN_POINT('Ctrl Pts',(23.0681158648922,-50.5316820401877,-28.735870483658));
#19511=CARTESIAN_POINT('Ctrl Pts',(23.0686596177156,-49.9996515905092,-28.7084234471774));
#19512=CARTESIAN_POINT('Ctrl Pts',(23.0699777810384,-49.9980579821568,-29.7915765528226));
#19513=CARTESIAN_POINT('Ctrl Pts',(23.0721774154546,-49.6222177557946,-29.7721663660449));
#19514=CARTESIAN_POINT('Ctrl Pts',(22.8347477112605,-48.2296051243342,-29.7001066715364));
#19515=CARTESIAN_POINT('Ctrl Pts',(20.7648507240798,-46.4550962552107,-29.5753974692971));
#19516=CARTESIAN_POINT('Ctrl Pts',(17.4497876216902,-47.4216757350208,-29.4174489461046));
#19517=CARTESIAN_POINT('Ctrl Pts',(16.4469245215085,-50.7259434096673,-29.2595004229122));
#19518=CARTESIAN_POINT('Ctrl Pts',(18.6655268957734,-53.3720202734039,-29.1015518997197));
#19519=CARTESIAN_POINT('Ctrl Pts',(22.0512087542155,-52.9659281134316,-28.9455772763565));
#19520=CARTESIAN_POINT('Ctrl Pts',(23.0753131520357,-50.9737419318929,-28.8422521607241));
#19521=CARTESIAN_POINT('Ctrl Pts',(23.0782820034225,-49.9993152063967,-28.7915765528225));
#19522=CARTESIAN_POINT('Origin',(20.,-50.,-42.2084234471774));
#19523=CARTESIAN_POINT('',(23.0715992618133,-50.0025559506913,-30.7915765528225));
#19524=CARTESIAN_POINT('',(23.0762469243503,-49.9977977477149,-30.7084234471774));
#19525=CARTESIAN_POINT('',(23.0735,-49.9999999999998,-42.2084234471774));
#19526=CARTESIAN_POINT('Ctrl Pts',(23.0762469243503,-49.9977977477149,-30.7084234471774));
#19527=CARTESIAN_POINT('Ctrl Pts',(23.0774077652693,-49.8547648430612,-30.7009979097613));
#19528=CARTESIAN_POINT('Ctrl Pts',(23.0036028704742,-48.6987851837245,-30.6409228646142));
#19529=CARTESIAN_POINT('Ctrl Pts',(21.5394357941431,-46.7164841598999,-30.5281983117364));
#19530=CARTESIAN_POINT('Ctrl Pts',(18.0920998235166,-46.9159676147846,-30.3702497885439));
#19531=CARTESIAN_POINT('Ctrl Pts',(16.3745989167479,-49.9116494367408,-30.2123012653515));
#19532=CARTESIAN_POINT('Ctrl Pts',(17.9441389105717,-52.98743602734,-30.054352742159));
#19533=CARTESIAN_POINT('Ctrl Pts',(21.3776656279966,-53.354605230716,-29.8964042189665));
#19534=CARTESIAN_POINT('Ctrl Pts',(22.9724077934703,-51.4022058860543,-29.7810944539727));
#19535=CARTESIAN_POINT('Ctrl Pts',(23.0765731516926,-50.1956548256145,-29.7184341967096));
#19536=CARTESIAN_POINT('Ctrl Pts',(23.0748402987193,-50.0025957432343,-29.7084234471774));
#19537=CARTESIAN_POINT('Ctrl Pts',(23.0715992618133,-50.0025559506913,-30.7915765528225));
#19538=CARTESIAN_POINT('Ctrl Pts',(23.0659003196299,-49.2900463831274,-30.7547300790965));
#19539=CARTESIAN_POINT('Ctrl Pts',(22.465560668895,-47.5507750303684,-30.6652340976396));
#19540=CARTESIAN_POINT('Ctrl Pts',(19.5796836114642,-46.3979626149297,-30.5230886084519));
#19541=CARTESIAN_POINT('Ctrl Pts',(16.7540570706331,-48.3828439502611,-30.3651400852594));
#19542=CARTESIAN_POINT('Ctrl Pts',(16.8714282629673,-51.8339514923121,-30.207191562067));
#19543=CARTESIAN_POINT('Ctrl Pts',(19.8253802980609,-53.6222709933982,-30.0492430388745));
#19544=CARTESIAN_POINT('Ctrl Pts',(22.5551894171279,-52.3102156517629,-29.9107047024597));
#19545=CARTESIAN_POINT('Ctrl Pts',(23.0662109778037,-50.6416722891319,-29.8248158737757));
#19546=CARTESIAN_POINT('Ctrl Pts',(23.0699777810384,-49.9980579821568,-29.7915765528226));
#19547=CARTESIAN_POINT('Origin',(20.,-50.,-42.2084234471774));
#19548=CARTESIAN_POINT('',(23.0783412386193,-49.9994310992988,-31.7915765528225));
#19549=CARTESIAN_POINT('',(23.0686854942479,-49.9995466737535,-31.7084234471775));
#19550=CARTESIAN_POINT('',(23.0735,-49.9999999999998,-42.2084234471774));
#19551=CARTESIAN_POINT('Ctrl Pts',(23.0686854942479,-49.9995466737535,-31.7084234471775));
#19552=CARTESIAN_POINT('Ctrl Pts',(23.0693266584817,-49.5176378585812,-31.6835616228129));
#19553=CARTESIAN_POINT('Ctrl Pts',(22.7361513781682,-48.0160365980268,-31.6060502907174));
#19554=CARTESIAN_POINT('Ctrl Pts',(20.3971790421746,-46.3953380678715,-31.4758894508912));
#19555=CARTESIAN_POINT('Ctrl Pts',(17.1987557115146,-47.6968783634582,-31.3179409276987));
#19556=CARTESIAN_POINT('Ctrl Pts',(16.5401353812306,-51.0865890006191,-31.1599924045063));
#19557=CARTESIAN_POINT('Ctrl Pts',(19.018469073759,-53.4911224380292,-31.0020438813138));
#19558=CARTESIAN_POINT('Ctrl Pts',(22.228377153031,-52.7661265353208,-30.8515208955375));
#19559=CARTESIAN_POINT('Ctrl Pts',(23.0691770205416,-50.8689152805637,-30.7536474174921));
#19560=CARTESIAN_POINT('Ctrl Pts',(23.0762469243503,-49.9977977477149,-30.7084234471774));
#19561=CARTESIAN_POINT('Ctrl Pts',(23.0783412386193,-49.9994310992988,-31.7915765528225));
#19562=CARTESIAN_POINT('Ctrl Pts',(23.0784219203286,-49.9680273678988,-31.7899432998789));
#19563=CARTESIAN_POINT('Ctrl Pts',(23.0638170352735,-48.9243704639443,-31.7356605392044));
#19564=CARTESIAN_POINT('Ctrl Pts',(21.888058303827,-46.9037805259858,-31.6287282707992));
#19565=CARTESIAN_POINT('Ctrl Pts',(18.4395124701376,-46.7264365197756,-31.4707797476067));
#19566=CARTESIAN_POINT('Ctrl Pts',(16.4058132196916,-49.5171329601522,-31.3128312244143));
#19567=CARTESIAN_POINT('Ctrl Pts',(17.6308538107017,-52.7456302598216,-31.1548827012217));
#19568=CARTESIAN_POINT('Ctrl Pts',(21.0039271972243,-53.4847481074805,-30.9969341780293));
#19569=CARTESIAN_POINT('Ctrl Pts',(22.8922345046466,-51.6289848188323,-30.8758321285629));
#19570=CARTESIAN_POINT('Ctrl Pts',(23.0740434733756,-50.308143210103,-30.8073795868273));
#19571=CARTESIAN_POINT('Ctrl Pts',(23.0715992618133,-50.0025559506913,-30.7915765528225));
#19572=CARTESIAN_POINT('Origin',(20.,-50.,-42.2084234471774));
#19573=CARTESIAN_POINT('',(23.070108680638,-49.9979840332082,-32.7915765528225));
#19574=CARTESIAN_POINT('',(23.0746461191906,-50.0026288889103,-32.7084234471774));
#19575=CARTESIAN_POINT('',(23.0735,-49.9999999999998,-42.2084234471774));
#19576=CARTESIAN_POINT('Ctrl Pts',(23.0746461191906,-50.0026288889103,-32.7084234471774));
#19577=CARTESIAN_POINT('Ctrl Pts',(23.0672844312647,-49.1867693456356,-32.6661253358645));
#19578=CARTESIAN_POINT('Ctrl Pts',(22.3159443950164,-47.3434040754006,-32.5711777168206));
#19579=CARTESIAN_POINT('Ctrl Pts',(19.2124032325014,-46.4600804856177,-32.4235805900461));
#19580=CARTESIAN_POINT('Ctrl Pts',(16.6052921443043,-48.7243443211601,-32.2656320668535));
#19581=CARTESIAN_POINT('Ctrl Pts',(17.0760594234942,-52.145206363393,-32.1076835436611));
#19582=CARTESIAN_POINT('Ctrl Pts',(20.1978746957691,-53.6210750394396,-31.9497350204685));
#19583=CARTESIAN_POINT('Ctrl Pts',(22.6771343927214,-52.0982945627933,-31.8166483216408));
#19584=CARTESIAN_POINT('Ctrl Pts',(23.067968874725,-50.5381688348235,-31.7362111305437));
#19585=CARTESIAN_POINT('Ctrl Pts',(23.0686854942479,-49.9995466737535,-31.7084234471775));
#19586=CARTESIAN_POINT('Ctrl Pts',(23.070108680638,-49.9979840332082,-32.7915765528225));
#19587=CARTESIAN_POINT('Ctrl Pts',(23.072358139719,-49.6287793568666,-32.7725070129305));
#19588=CARTESIAN_POINT('Ctrl Pts',(22.8404342309996,-48.2429602032945,-32.7007879653077));
#19589=CARTESIAN_POINT('Ctrl Pts',(20.7875967780819,-46.4600804380509,-32.576419409954));
#19590=CARTESIAN_POINT('Ctrl Pts',(17.4663956098388,-47.4053539771154,-32.4184708867615));
#19591=CARTESIAN_POINT('Ctrl Pts',(16.4423364860605,-50.7031141525378,-32.2605223635691));
#19592=CARTESIAN_POINT('Ctrl Pts',(18.6439026689266,-53.3633821101044,-32.1025738403766));
#19593=CARTESIAN_POINT('Ctrl Pts',(22.0395220840648,-52.978198375694,-31.9462585701278));
#19594=CARTESIAN_POINT('Ctrl Pts',(23.0758210664351,-50.9803573964871,-31.8425928076097));
#19595=CARTESIAN_POINT('Ctrl Pts',(23.0783412386193,-49.9994310992988,-31.7915765528225));
#19596=CARTESIAN_POINT('Origin',(20.,-50.,-42.2084234471774));
#19597=CARTESIAN_POINT('',(23.071426479794,-50.0025153263093,-33.7915765528226));
#19598=CARTESIAN_POINT('',(23.0764188231986,-49.997867531766,-33.7084234471775));
#19599=CARTESIAN_POINT('',(23.0735,-49.9999999999998,-42.2084234471774));
#19600=CARTESIAN_POINT('Ctrl Pts',(23.0764188231986,-49.997867531766,-33.7084234471775));
#19601=CARTESIAN_POINT('Ctrl Pts',(23.0775013376664,-49.8614161856796,-33.7013385566469));
#19602=CARTESIAN_POINT('Ctrl Pts',(23.0075099798091,-48.7120794545905,-33.6416041583855));
#19603=CARTESIAN_POINT('Ctrl Pts',(21.5604875088938,-46.7264365637634,-33.5292202523933));
#19604=CARTESIAN_POINT('Ctrl Pts',(18.1119417215434,-46.9037805675905,-33.3712717292008));
#19605=CARTESIAN_POINT('Ctrl Pts',(16.3752409525729,-49.8883725635259,-33.2133232060083));
#19606=CARTESIAN_POINT('Ctrl Pts',(17.9249989698413,-52.9741737611174,-33.0553746828159));
#19607=CARTESIAN_POINT('Ctrl Pts',(21.3560973128511,-53.3633820649098,-32.8974261596234));
#19608=CARTESIAN_POINT('Ctrl Pts',(22.9680910641118,-51.4155254173783,-32.7817757477439));
#19609=CARTESIAN_POINT('Ctrl Pts',(23.076447706724,-50.2022899444883,-32.7187748435953));
#19610=CARTESIAN_POINT('Ctrl Pts',(23.0746461191906,-50.0026288889103,-32.7084234471774));
#19611=CARTESIAN_POINT('Ctrl Pts',(23.0714264797939,-50.0025153263093,-33.7915765528226));
#19612=CARTESIAN_POINT('Ctrl Pts',(23.0658929944555,-49.2964923448543,-33.7550707259821));
#19613=CARTESIAN_POINT('Ctrl Pts',(22.4743382857738,-47.5638498555385,-33.6659153914109));
#19614=CARTESIAN_POINT('Ctrl Pts',(19.6028209524885,-46.3953380194348,-33.5241105491088));
#19615=CARTESIAN_POINT('Ctrl Pts',(16.7645077415746,-48.362035093299,-33.3661620259164));
#19616=CARTESIAN_POINT('Ctrl Pts',(16.8597169583261,-51.8138251316183,-33.2082135027239));
#19617=CARTESIAN_POINT('Ctrl Pts',(19.8021253015719,-53.621075088097,-33.0502649795314));
#19618=CARTESIAN_POINT('Ctrl Pts',(22.5470356567185,-52.3233918947014,-32.9113859962309));
#19619=CARTESIAN_POINT('Ctrl Pts',(23.0661475591835,-50.6481245834092,-32.8251565206613));
#19620=CARTESIAN_POINT('Ctrl Pts',(23.070108680638,-49.9979840332082,-32.7915765528225));
#19621=CARTESIAN_POINT('Origin',(20.,-50.,-42.2084234471774));
#19622=CARTESIAN_POINT('',(23.0783901429301,-49.9995482667377,-34.7915765528226));
#19623=CARTESIAN_POINT('',(23.0687181382264,-49.9994424172299,-34.7084234471775));
#19624=CARTESIAN_POINT('',(23.0735,-49.9999999999998,-42.2084234471774));
#19625=CARTESIAN_POINT('Ctrl Pts',(23.0687181382264,-49.9994424172299,-34.7084234471775));
#19626=CARTESIAN_POINT('Ctrl Pts',(23.0694964277012,-49.5241491644738,-34.6839022696985));
#19627=CARTESIAN_POINT('Ctrl Pts',(22.7427399824597,-48.0293655359017,-34.6067315844887));
#19628=CARTESIAN_POINT('Ctrl Pts',(20.420316382888,-46.3979626633313,-34.4769113915481));
#19629=CARTESIAN_POINT('Ctrl Pts',(17.213601799006,-47.6789390568155,-34.3189628683557));
#19630=CARTESIAN_POINT('Ctrl Pts',(16.5332297194947,-51.0643508156075,-34.1610143451632));
#19631=CARTESIAN_POINT('Ctrl Pts',(18.9960728162657,-53.4847480606549,-34.0030658219707));
#19632=CARTESIAN_POINT('Ctrl Pts',(22.217844613828,-52.7787838660493,-33.8522021893088));
#19633=CARTESIAN_POINT('Ctrl Pts',(23.0694569150187,-50.875418613757,-33.7539880643777));
#19634=CARTESIAN_POINT('Ctrl Pts',(23.0764188231986,-49.997867531766,-33.7084234471775));
#19635=CARTESIAN_POINT('Ctrl Pts',(23.0783901429301,-49.9995482667377,-34.7915765528226));
#19636=CARTESIAN_POINT('Ctrl Pts',(23.0784416291869,-49.9746954594268,-34.7902839467646));
#19637=CARTESIAN_POINT('Ctrl Pts',(23.06695636405,-48.9376046282268,-34.7363418329757));
#19638=CARTESIAN_POINT('Ctrl Pts',(21.9079002021205,-46.9159675733437,-34.6297502114561));
#19639=CARTESIAN_POINT('Ctrl Pts',(18.4605641851711,-46.7164841157783,-34.4718016882636));
#19640=CARTESIAN_POINT('Ctrl Pts',(16.4089878017039,-49.4940646468145,-34.3138531650711));
#19641=CARTESIAN_POINT('Ctrl Pts',(17.6132729627324,-52.7303613752562,-34.1559046418787));
#19642=CARTESIAN_POINT('Ctrl Pts',(20.98153093943,-53.4911224849404,-33.9979561186862));
#19643=CARTESIAN_POINT('Ctrl Pts',(22.887060184286,-51.6423364239543,-33.8765134223342));
#19644=CARTESIAN_POINT('Ctrl Pts',(23.0738735089191,-50.3147342431337,-33.8077202337129));
#19645=CARTESIAN_POINT('Ctrl Pts',(23.0714264797939,-50.0025153263093,-33.7915765528226));
#19646=CARTESIAN_POINT('Origin',(20.,-50.,-42.2084234471774));
#19647=CARTESIAN_POINT('',(23.070244715626,-49.9979131053482,-35.7915765528225));
#19648=CARTESIAN_POINT('',(23.0744509199104,-50.0026575649045,-35.7084234471775));
#19649=CARTESIAN_POINT('',(23.0735,-49.9999999999998,-42.2084234471774));
#19650=CARTESIAN_POINT('Ctrl Pts',(23.0744509199104,-50.0026575649045,-35.7084234471775));
#19651=CARTESIAN_POINT('Ctrl Pts',(23.0671206442753,-49.1932360925919,-35.6664659827501));
#19652=CARTESIAN_POINT('Ctrl Pts',(22.325805068483,-47.3562448982243,-35.5718590105919));
#19653=CARTESIAN_POINT('Ctrl Pts',(19.2351492861978,-46.4550963028444,-35.4246025307029));
#19654=CARTESIAN_POINT('Ctrl Pts',(16.613553108674,-48.7025732048773,-35.2666540075104));
#19655=CARTESIAN_POINT('Ctrl Pts',(17.0623453333896,-52.1263875225874,-35.108705484318));
#19656=CARTESIAN_POINT('Ctrl Pts',(20.1746196995926,-53.6222709447248,-34.9507569611255));
#19657=CARTESIAN_POINT('Ctrl Pts',(22.6699768333288,-52.111584321713,-34.817329615412));
#19658=CARTESIAN_POINT('Ctrl Pts',(23.0678253595906,-50.5446530047506,-34.7365517774293));
#19659=CARTESIAN_POINT('Ctrl Pts',(23.0687181382264,-49.9994424172299,-34.7084234471775));
#19660=CARTESIAN_POINT('Ctrl Pts',(23.070244715626,-49.9979131053482,-35.7915765528225));
#19661=CARTESIAN_POINT('Ctrl Pts',(23.0725383031763,-49.6353441091479,-35.7728476598162));
#19662=CARTESIAN_POINT('Ctrl Pts',(22.8460663522941,-48.2563155171469,-35.7014692590789));
#19663=CARTESIAN_POINT('Ctrl Pts',(20.81031035977,-46.4652105704865,-35.5774413506109));
#19664=CARTESIAN_POINT('Ctrl Pts',(17.4831080575873,-47.3891391955688,-35.4194928274184));
#19665=CARTESIAN_POINT('Ctrl Pts',(16.4378951318222,-50.6802559062359,-35.261544304226));
#19666=CARTESIAN_POINT('Ctrl Pts',(18.6223343534913,-53.3546052757928,-35.1035957810335));
#19667=CARTESIAN_POINT('Ctrl Pts',(22.0277621047601,-52.9904408764762,-34.946939863899));
#19668=CARTESIAN_POINT('Ctrl Pts',(23.0763445277092,-50.9869822753117,-34.8429334544954));
#19669=CARTESIAN_POINT('Ctrl Pts',(23.0783901429301,-49.9995482667377,-34.7915765528226));
#19670=CARTESIAN_POINT('Origin',(20.,-50.,-42.2084234471774));
#19671=CARTESIAN_POINT('',(23.0712572257215,-50.0024708151107,-36.7915765528225));
#19672=CARTESIAN_POINT('',(23.0765864796728,-49.9979412458126,-36.7084234471775));
#19673=CARTESIAN_POINT('',(23.0735,-49.9999999999998,-42.2084234471774));
#19674=CARTESIAN_POINT('Ctrl Pts',(23.0765864796728,-49.9979412458126,-36.7084234471775));
#19675=CARTESIAN_POINT('Ctrl Pts',(23.0775908951925,-49.868069099325,-36.7016792035325));
#19676=CARTESIAN_POINT('Ctrl Pts',(23.0113703825189,-48.7253704994309,-36.6422854521568));
#19677=CARTESIAN_POINT('Ctrl Pts',(21.581474885261,-46.7365239360518,-36.5302421930502));
#19678=CARTESIAN_POINT('Ctrl Pts',(18.1318614635619,-46.8917211761413,-36.3722936698578));
#19679=CARTESIAN_POINT('Ctrl Pts',(16.3760324359193,-49.8651002928142,-36.2143451466652));
#19680=CARTESIAN_POINT('Ctrl Pts',(17.905944580671,-52.960788870692,-36.0563966234728));
#19681=CARTESIAN_POINT('Ctrl Pts',(21.3344730862948,-53.3720202280932,-35.8984481002803));
#19682=CARTESIAN_POINT('Ctrl Pts',(22.963725640928,-51.4288475622717,-35.7824570415152));
#19683=CARTESIAN_POINT('Ctrl Pts',(23.0763188980065,-50.2089228755193,-35.7191154904809));
#19684=CARTESIAN_POINT('Ctrl Pts',(23.0744509199104,-50.0026575649045,-35.7084234471775));
#19685=CARTESIAN_POINT('Ctrl Pts',(23.0712572257215,-50.0024708151107,-36.7915765528225));
#19686=CARTESIAN_POINT('Ctrl Pts',(23.0658938563175,-49.302938396495,-36.7554113728678));
#19687=CARTESIAN_POINT('Ctrl Pts',(22.4830499320534,-47.5769365408491,-36.6665966851821));
#19688=CARTESIAN_POINT('Ctrl Pts',(19.625974670453,-46.3928620411136,-36.5251324897657));
#19689=CARTESIAN_POINT('Ctrl Pts',(16.775091810017,-48.3412937699339,-36.3671839665732));
#19690=CARTESIAN_POINT('Ctrl Pts',(16.8481351267915,-51.7936239871129,-36.2092354433808));
#19691=CARTESIAN_POINT('Ctrl Pts',(19.7788784632106,-53.6197298873777,-36.0512869201883));
#19692=CARTESIAN_POINT('Ctrl Pts',(22.538817759059,-52.3365588076076,-35.9120672900022));
#19693=CARTESIAN_POINT('Ctrl Pts',(23.0660907114569,-50.6545756868969,-35.825497167547));
#19694=CARTESIAN_POINT('Ctrl Pts',(23.070244715626,-49.9979131053482,-35.7915765528225));
#19695=CARTESIAN_POINT('Origin',(20.,-50.,-42.2084234471774));
#19696=CARTESIAN_POINT('',(23.0784283983202,-49.9996663588637,-37.7915765528226));
#19697=CARTESIAN_POINT('',(23.0687575115238,-49.9993389974064,-37.7084234471775));
#19698=CARTESIAN_POINT('',(23.0735,-49.9999999999998,-42.2084234471774));
#19699=CARTESIAN_POINT('Ctrl Pts',(23.0687575115238,-49.9993389974064,-37.7084234471775));
#19700=CARTESIAN_POINT('Ctrl Pts',(23.0696680463346,-49.5306635124935,-37.6842429165841));
#19701=CARTESIAN_POINT('Ctrl Pts',(22.749270481726,-48.0426974119101,-37.60741287826));
#19702=CARTESIAN_POINT('Ctrl Pts',(20.4434363918007,-46.4007358047025,-37.477933332205));
#19703=CARTESIAN_POINT('Ctrl Pts',(17.228562769865,-47.6610954290179,-37.3199848090125));
#19704=CARTESIAN_POINT('Ctrl Pts',(16.5264669908866,-51.0420687566668,-37.1620362858201));
#19705=CARTESIAN_POINT('Ctrl Pts',(18.9737179506262,-53.4782300038948,-37.0040877626276));
#19706=CARTESIAN_POINT('Ctrl Pts',(22.2072411043633,-52.7914200520352,-36.85288348308));
#19707=CARTESIAN_POINT('Ctrl Pts',(23.069749840591,-50.8819269817663,-36.7543287112634));
#19708=CARTESIAN_POINT('Ctrl Pts',(23.0765864796728,-49.9979412458126,-36.7084234471775));
#19709=CARTESIAN_POINT('Ctrl Pts',(23.0784283983202,-49.9996663588637,-37.7915765528226));
#19710=CARTESIAN_POINT('Ctrl Pts',(23.0784568430445,-49.981363743946,-37.7906245936502));
#19711=CARTESIAN_POINT('Ctrl Pts',(23.0700523868523,-48.9508348052474,-37.737023126747));
#19712=CARTESIAN_POINT('Ctrl Pts',(21.9276632661251,-46.9282819927009,-37.630772152113));
#19713=CARTESIAN_POINT('Ctrl Pts',(18.4816794571067,-46.7066669802649,-37.4728236289205));
#19714=CARTESIAN_POINT('Ctrl Pts',(16.4123103964255,-49.471017248116,-37.314875105728));
#19715=CARTESIAN_POINT('Ctrl Pts',(17.5957905404958,-52.7149798911831,-37.1569265825356));
#19716=CARTESIAN_POINT('Ctrl Pts',(20.9590942025022,-53.497352938559,-36.9989780593431));
#19717=CARTESIAN_POINT('Ctrl Pts',(22.8818334298203,-51.6556889545473,-36.8771947161054));
#19718=CARTESIAN_POINT('Ctrl Pts',(23.0737018849034,-50.3213223096376,-36.8080608805986));
#19719=CARTESIAN_POINT('Ctrl Pts',(23.0712572257215,-50.0024708151107,-36.7915765528225));
#19720=CARTESIAN_POINT('Origin',(20.,-50.,-42.2084234471774));
#19721=CARTESIAN_POINT('',(23.0703817199364,-49.9978503929169,-38.7915765528226));
#19722=CARTESIAN_POINT('',(23.0742548311415,-50.0026845243509,-38.7084234471775));
#19723=CARTESIAN_POINT('',(23.0735,-49.9999999999998,-42.2084234471774));
#19724=CARTESIAN_POINT('Ctrl Pts',(23.0742548311415,-50.0026845243509,-38.7084234471775));
#19725=CARTESIAN_POINT('Ctrl Pts',(23.0669678464909,-49.1997028226788,-38.6668066296357));
#19726=CARTESIAN_POINT('Ctrl Pts',(22.3355968763498,-47.3690990017349,-38.5725403043632));
#19727=CARTESIAN_POINT('Ctrl Pts',(19.257926730837,-46.4502604667964,-38.4256244713598));
#19728=CARTESIAN_POINT('Ctrl Pts',(16.6219537671653,-48.6808544802542,-38.2676759481673));
#19729=CARTESIAN_POINT('Ctrl Pts',(17.0487523255225,-52.107481564476,-38.1097274249749));
#19730=CARTESIAN_POINT('Ctrl Pts',(20.1513575221015,-53.6233172273567,-37.9517789017824));
#19731=CARTESIAN_POINT('Ctrl Pts',(22.6627587165777,-52.1248689098524,-37.8180109091833));
#19732=CARTESIAN_POINT('Ctrl Pts',(23.0676854922557,-50.5511346502516,-37.736892424315));
#19733=CARTESIAN_POINT('Ctrl Pts',(23.0687575115238,-49.9993389974064,-37.7084234471775));
#19734=CARTESIAN_POINT('Ctrl Pts',(23.0703817199364,-49.9978503929169,-38.7915765528226));
#19735=CARTESIAN_POINT('Ctrl Pts',(23.072717480822,-49.6419123660289,-38.7731883067018));
#19736=CARTESIAN_POINT('Ctrl Pts',(22.8516587059108,-48.2696526564415,-38.7021505528502));
#19737=CARTESIAN_POINT('Ctrl Pts',(20.8329798036235,-46.4705000476597,-38.5784632912678));
#19738=CARTESIAN_POINT('Ctrl Pts',(17.4999296646635,-47.373025224819,-38.4205147680753));
#19739=CARTESIAN_POINT('Ctrl Pts',(16.4335979353407,-50.6573730457065,-38.2625662448828));
#19740=CARTESIAN_POINT('Ctrl Pts',(18.600824198122,-53.3456884082951,-38.1046177216904));
#19741=CARTESIAN_POINT('Ctrl Pts',(22.0159280202989,-53.0026560286412,-37.9476211576702));
#19742=CARTESIAN_POINT('Ctrl Pts',(23.0768836655619,-50.9936168883794,-37.843274101381));
#19743=CARTESIAN_POINT('Ctrl Pts',(23.0784283983202,-49.9996663588637,-37.7915765528226));
#19744=CARTESIAN_POINT('Origin',(20.,-50.,-42.2084234471774));
#19745=CARTESIAN_POINT('',(23.0703065393339,-50.0033432771247,-39.7915765528225));
#19746=CARTESIAN_POINT('',(23.0767447721987,-49.9980895972328,-39.7084234471774));
#19747=CARTESIAN_POINT('',(23.0735,-49.9999999999998,-42.2084234471774));
#19748=CARTESIAN_POINT('',(20.7937992825328,-52.9692229537457,-40.));
#19749=CARTESIAN_POINT('Ctrl Pts',(20.7937992825328,-52.9692229537457,-40.));
#19750=CARTESIAN_POINT('Ctrl Pts',(21.7760378723045,-52.7066289013681,-39.9473504922692));
#19751=CARTESIAN_POINT('Ctrl Pts',(22.8758105836868,-51.6693936165595,-39.8778760098767));
#19752=CARTESIAN_POINT('Ctrl Pts',(23.0726592954589,-50.3288663223125,-39.8084015274842));
#19753=CARTESIAN_POINT('Ctrl Pts',(23.0703065393339,-50.0033432771247,-39.7915765528225));
#19754=CARTESIAN_POINT('',(19.2043379022879,-52.9742864271603,-40.));
#19755=CARTESIAN_POINT('Origin',(20.,-50.,-40.));
#19756=CARTESIAN_POINT('Ctrl Pts',(19.2043340224364,-52.9742969733088,-40.));
#19757=CARTESIAN_POINT('Ctrl Pts',(20.1513499766094,-53.2252255075611,-39.9490537266973));
#19758=CARTESIAN_POINT('Ctrl Pts',(22.2116710273535,-52.7701102416077,-39.8518615424232));
#19759=CARTESIAN_POINT('Ctrl Pts',(23.0700634780488,-50.8883224575133,-39.754669358149));
#19760=CARTESIAN_POINT('Ctrl Pts',(23.0767447721987,-49.9980895972329,-39.7084234471774));
#19761=CARTESIAN_POINT('Origin',(20.,50.,-42.2084234471774));
#19762=CARTESIAN_POINT('',(23.0782114598495,50.0008183538095,-25.7915765528225));
#19763=CARTESIAN_POINT('',(23.0685692638887,50.000333297858,-25.7084234471774));
#19764=CARTESIAN_POINT('',(23.0735,50.0000000000002,-42.2084234471774));
#19765=CARTESIAN_POINT('',(19.2062007174672,47.0307770462543,-25.));
#19766=CARTESIAN_POINT('Ctrl Pts',(23.0685692638887,50.000333297858,-25.7084234471774));
#19767=CARTESIAN_POINT('Ctrl Pts',(23.068887248526,50.495510231703,-25.6828803290416));
#19768=CARTESIAN_POINT('Ctrl Pts',(22.7226354451561,52.0108186486332,-25.6046877031749));
#19769=CARTESIAN_POINT('Ctrl Pts',(20.3515248813337,53.6086151161717,-25.4738455695774));
#19770=CARTESIAN_POINT('Ctrl Pts',(17.1680751579223,52.2686685512262,-25.3158970463849));
#19771=CARTESIAN_POINT('Ctrl Pts',(16.5570909615237,48.8654544718428,-25.1579485231925));
#19772=CARTESIAN_POINT('Ctrl Pts',(18.2239621276955,47.2933710986319,-25.0526495077308));
#19773=CARTESIAN_POINT('Ctrl Pts',(19.2062007174672,47.0307770462543,-25.));
#19774=CARTESIAN_POINT('',(20.7937992825328,47.0307770462543,-25.));
#19775=CARTESIAN_POINT('Origin',(20.,50.,-25.));
#19776=CARTESIAN_POINT('Ctrl Pts',(23.0782114598495,50.0008183538095,-25.7915765528225));
#19777=CARTESIAN_POINT('Ctrl Pts',(23.0783674790197,50.0453262282883,-25.7892620061076));
#19778=CARTESIAN_POINT('Ctrl Pts',(23.057406892625,51.1021122772341,-25.7342979516619));
#19779=CARTESIAN_POINT('Ctrl Pts',(21.8481506426783,53.1200734299207,-25.6266843894854));
#19780=CARTESIAN_POINT('Ctrl Pts',(18.3975852298821,53.2535259099818,-25.4687358662929));
#19781=CARTESIAN_POINT('Ctrl Pts',(16.3999441908908,50.4361302999107,-25.3107873431005));
#19782=CARTESIAN_POINT('Ctrl Pts',(17.6525830669794,47.2598757730875,-25.1545420543361));
#19783=CARTESIAN_POINT('Ctrl Pts',(19.8486498414593,46.7747744006132,-25.0509462733027));
#19784=CARTESIAN_POINT('Ctrl Pts',(20.7956658684167,47.0257030027424,-25.));
#19785=CARTESIAN_POINT('Origin',(20.,50.,-42.2084234471774));
#19786=CARTESIAN_POINT('',(23.0698520292984,50.0018654680674,-26.7915765528225));
#19787=CARTESIAN_POINT('',(23.0750331521824,49.9974416679533,-26.7084234471775));
#19788=CARTESIAN_POINT('',(23.0735,50.0000000000002,-42.2084234471774));
#19789=CARTESIAN_POINT('Ctrl Pts',(23.0750331521824,49.9974416679533,-26.7084234471775));
#19790=CARTESIAN_POINT('Ctrl Pts',(23.0676452399249,50.8261740335002,-26.6654440420932));
#19791=CARTESIAN_POINT('Ctrl Pts',(22.2960104470904,52.682230047647,-26.5698151292781));
#19792=CARTESIAN_POINT('Ctrl Pts',(19.1670202507297,53.5294997326245,-26.4215367087322));
#19793=CARTESIAN_POINT('Ctrl Pts',(16.5891692111351,51.2319836373097,-26.2635881855398));
#19794=CARTESIAN_POINT('Ctrl Pts',(17.1038913663152,47.8173681526091,-26.1056396623473));
#19795=CARTESIAN_POINT('Ctrl Pts',(20.2442745382167,46.3818722728576,-25.9476911391548));
#19796=CARTESIAN_POINT('Ctrl Pts',(22.6913963181601,47.9281378306177,-25.8152857340982));
#19797=CARTESIAN_POINT('Ctrl Pts',(23.0682318181854,49.4748509031148,-25.7355298367724));
#19798=CARTESIAN_POINT('Ctrl Pts',(23.0685692638887,50.000333297858,-25.7084234471774));
#19799=CARTESIAN_POINT('Ctrl Pts',(23.0698520292984,50.0018654680674,-26.7915765528225));
#19800=CARTESIAN_POINT('Ctrl Pts',(23.0719961218878,50.3843410331866,-26.7718257191592));
#19801=CARTESIAN_POINT('Ctrl Pts',(22.8290064229413,51.7837499147479,-26.6994253777651));
#19802=CARTESIAN_POINT('Ctrl Pts',(20.7420732493018,53.5497394380497,-26.5743755286402));
#19803=CARTESIAN_POINT('Ctrl Pts',(17.4332845947801,52.5619004681089,-26.4164270054477));
#19804=CARTESIAN_POINT('Ctrl Pts',(16.4516597580046,49.2512486007173,-26.2584784822552));
#19805=CARTESIAN_POINT('Ctrl Pts',(18.6872050642303,46.6194980305971,-26.1005299590628));
#19806=CARTESIAN_POINT('Ctrl Pts',(22.0628243622956,47.0463358989535,-25.9448959825852));
#19807=CARTESIAN_POINT('Ctrl Pts',(23.0748184763337,49.0328957310464,-25.8419115138385));
#19808=CARTESIAN_POINT('Ctrl Pts',(23.0782114598495,50.0008183538095,-25.7915765528225));
#19809=CARTESIAN_POINT('Origin',(20.,50.,-42.2084234471774));
#19810=CARTESIAN_POINT('',(23.0717752285503,49.997407390237,-27.7915765528225));
#19811=CARTESIAN_POINT('',(23.0760710189578,50.0022679983574,-27.7084234471775));
#19812=CARTESIAN_POINT('',(23.0735,50.0000000000002,-42.2084234471774));
#19813=CARTESIAN_POINT('Ctrl Pts',(23.0760710189578,50.0022679983574,-27.7084234471775));
#19814=CARTESIAN_POINT('Ctrl Pts',(23.0773101161764,50.1518848359786,-27.7006572628756));
#19815=CARTESIAN_POINT('Ctrl Pts',(22.9996487300235,51.314512194804,-27.640241570843));
#19816=CARTESIAN_POINT('Ctrl Pts',(21.518320457159,53.29333283432,-27.5271763710795));
#19817=CARTESIAN_POINT('Ctrl Pts',(18.0723368427983,53.0717178336273,-27.369227847887));
#19818=CARTESIAN_POINT('Ctrl Pts',(16.3741061672535,50.0650704804189,-27.2112793246946));
#19819=CARTESIAN_POINT('Ctrl Pts',(17.9633643847556,46.9994241385813,-27.0533308015021));
#19820=CARTESIAN_POINT('Ctrl Pts',(21.3991757215647,46.654311783583,-26.8953822783096));
#19821=CARTESIAN_POINT('Ctrl Pts',(22.9766775148259,48.6111089836517,-26.7804131602014));
#19822=CARTESIAN_POINT('Ctrl Pts',(23.0766953871467,49.8109819664833,-26.718093549824));
#19823=CARTESIAN_POINT('Ctrl Pts',(23.0750331521824,49.9974416679533,-26.7084234471775));
#19824=CARTESIAN_POINT('Ctrl Pts',(23.0717752285503,49.997407390237,-27.7915765528225));
#19825=CARTESIAN_POINT('Ctrl Pts',(23.0659158967544,50.7163996078025,-27.7543894322109));
#19826=CARTESIAN_POINT('Ctrl Pts',(22.4567167775476,52.4622875427393,-27.6645528038683));
#19827=CARTESIAN_POINT('Ctrl Pts',(19.5565636198783,53.5992641004309,-27.522066667795));
#19828=CARTESIAN_POINT('Ctrl Pts',(16.743740353733,51.5962805246318,-27.3641181446025));
#19829=CARTESIAN_POINT('Ctrl Pts',(16.8832686906281,48.1459976943029,-27.2061696214101));
#19830=CARTESIAN_POINT('Ctrl Pts',(19.8486424819224,46.3766828683592,-27.0482210982176));
#19831=CARTESIAN_POINT('Ctrl Pts',(22.5632791857677,47.7029692840987,-26.9100234086884));
#19832=CARTESIAN_POINT('Ctrl Pts',(23.0662806457067,49.3647815266923,-26.8244752268901));
#19833=CARTESIAN_POINT('Ctrl Pts',(23.0698520292984,50.0018654680674,-26.7915765528225));
#19834=CARTESIAN_POINT('Origin',(20.,50.,-42.2084234471774));
#19835=CARTESIAN_POINT('',(23.0782818809563,50.0006847935759,-28.7915765528225));
#19836=CARTESIAN_POINT('',(23.068659485942,50.0003484094753,-28.7084234471774));
#19837=CARTESIAN_POINT('',(23.0735,50.0000000000002,-42.2084234471774));
#19838=CARTESIAN_POINT('Ctrl Pts',(23.068659485942,50.0003484094753,-28.7084234471774));
#19839=CARTESIAN_POINT('Ctrl Pts',(23.0691587716964,50.4888704233529,-28.6832209759272));
#19840=CARTESIAN_POINT('Ctrl Pts',(22.7295043166397,51.9972890662579,-28.6053689969462));
#19841=CARTESIAN_POINT('Ctrl Pts',(20.3740253084567,53.6071377555246,-28.4748675102343));
#19842=CARTESIAN_POINT('Ctrl Pts',(17.1840252420261,52.2850872713679,-28.3169189870418));
#19843=CARTESIAN_POINT('Ctrl Pts',(16.5471838347117,48.8912176686634,-28.1589704638494));
#19844=CARTESIAN_POINT('Ctrl Pts',(19.0409058515914,46.5026472585805,-28.0010219406569));
#19845=CARTESIAN_POINT('Ctrl Pts',(22.238838770898,47.246551697553,-27.8508396017662));
#19846=CARTESIAN_POINT('Ctrl Pts',(23.0689098701799,49.1375832764411,-27.7533067706064));
#19847=CARTESIAN_POINT('Ctrl Pts',(23.0760710189578,50.0022679983574,-27.7084234471775));
#19848=CARTESIAN_POINT('Ctrl Pts',(23.0782818809564,50.0006847935759,-28.7915765528225));
#19849=CARTESIAN_POINT('Ctrl Pts',(23.0783975226873,50.0386403455705,-28.7896026529933));
#19850=CARTESIAN_POINT('Ctrl Pts',(23.060633926734,51.0888674093361,-28.7349792454332));
#19851=CARTESIAN_POINT('Ctrl Pts',(21.868138487219,53.1082787419663,-28.6277063301423));
#19852=CARTESIAN_POINT('Ctrl Pts',(18.4185251564057,53.2634759779658,-28.4697578069498));
#19853=CARTESIAN_POINT('Ctrl Pts',(16.4027869677635,50.4597788009081,-28.3118092837573));
#19854=CARTESIAN_POINT('Ctrl Pts',(17.6485324314252,47.2392141645673,-28.1538607605649));
#19855=CARTESIAN_POINT('Ctrl Pts',(21.026282022335,46.5217700877505,-27.9959122373724));
#19856=CARTESIAN_POINT('Ctrl Pts',(22.8973565003072,48.3843657956996,-27.8751508347916));
#19857=CARTESIAN_POINT('Ctrl Pts',(23.0742115359331,49.6984507670629,-27.8070389399417));
#19858=CARTESIAN_POINT('Ctrl Pts',(23.0717752285503,49.997407390237,-27.7915765528225));
#19859=CARTESIAN_POINT('Origin',(20.,50.,-42.2084234471774));
#19860=CARTESIAN_POINT('',(23.0699776589026,50.0019420177659,-29.7915765528226));
#19861=CARTESIAN_POINT('',(23.07484016668,49.9974042568772,-29.7084234471775));
#19862=CARTESIAN_POINT('',(23.0735,50.0000000000002,-42.2084234471774));
#19863=CARTESIAN_POINT('Ctrl Pts',(23.07484016668,49.9974042568772,-29.7084234471775));
#19864=CARTESIAN_POINT('Ctrl Pts',(23.0674594310508,50.819700244974,-29.6657846889788));
#19865=CARTESIAN_POINT('Ctrl Pts',(22.3060143175262,52.6694190871755,-29.5704964230494));
#19866=CARTESIAN_POINT('Ctrl Pts',(19.1896896859145,53.5347892302254,-29.4225586493891));
#19867=CARTESIAN_POINT('Ctrl Pts',(16.5971712887038,51.2538319138251,-29.2646101261966));
#19868=CARTESIAN_POINT('Ctrl Pts',(17.0898941915086,47.8360633349363,-29.1066616030042));
#19869=CARTESIAN_POINT('Ctrl Pts',(20.2211215243232,46.3802703166986,-28.9487130798117));
#19870=CARTESIAN_POINT('Ctrl Pts',(22.684231513376,47.9150003041815,-28.8159670278695));
#19871=CARTESIAN_POINT('Ctrl Pts',(23.0681157331418,49.4683179826435,-28.735870483658));
#19872=CARTESIAN_POINT('Ctrl Pts',(23.068659485942,50.0003484094753,-28.7084234471774));
#19873=CARTESIAN_POINT('Ctrl Pts',(23.0699776589026,50.0019420177659,-29.7915765528226));
#19874=CARTESIAN_POINT('Ctrl Pts',(23.0721772932313,50.3777822291758,-29.7721663660449));
#19875=CARTESIAN_POINT('Ctrl Pts',(22.8347475984832,51.7703948052325,-29.7001066715364));
#19876=CARTESIAN_POINT('Ctrl Pts',(20.7648506936511,53.5449036037592,-29.5753974692971));
#19877=CARTESIAN_POINT('Ctrl Pts',(17.4497877231476,52.5783241624032,-29.4174489461046));
#19878=CARTESIAN_POINT('Ctrl Pts',(16.4469246628638,49.2740566192138,-29.2595004229122));
#19879=CARTESIAN_POINT('Ctrl Pts',(18.665526948864,46.6279798607482,-29.1015518997197));
#19880=CARTESIAN_POINT('Ctrl Pts',(22.0512086726104,47.0340720045647,-28.9455772763565));
#19881=CARTESIAN_POINT('Ctrl Pts',(23.0753130296877,49.0262581068463,-28.8422521607241));
#19882=CARTESIAN_POINT('Ctrl Pts',(23.0782818809564,50.0006847935759,-28.7915765528225));
#19883=CARTESIAN_POINT('Origin',(20.,50.,-42.2084234471774));
#19884=CARTESIAN_POINT('',(23.071599139613,49.9974440494104,-30.7915765528225));
#19885=CARTESIAN_POINT('',(23.0762467922506,50.0022022521905,-30.7084234471775));
#19886=CARTESIAN_POINT('',(23.0735,50.0000000000002,-42.2084234471774));
#19887=CARTESIAN_POINT('Ctrl Pts',(23.0762467922506,50.0022022521905,-30.7084234471775));
#19888=CARTESIAN_POINT('Ctrl Pts',(23.0774076331198,50.1452351507021,-30.7009979097613));
#19889=CARTESIAN_POINT('Ctrl Pts',(23.003602741494,51.3012147603989,-30.6409228646142));
#19890=CARTESIAN_POINT('Ctrl Pts',(21.5394357280369,53.2835156991,-30.5281983117364));
#19891=CARTESIAN_POINT('Ctrl Pts',(18.0920999054453,53.0840322527814,-30.370249788544));
#19892=CARTESIAN_POINT('Ctrl Pts',(16.3745990724293,50.0883505594653,-30.2123012653514));
#19893=CARTESIAN_POINT('Ctrl Pts',(17.9441389988542,47.012564100946,-30.054352742159));
#19894=CARTESIAN_POINT('Ctrl Pts',(21.3776655688371,46.6453949133369,-29.8964042189665));
#19895=CARTESIAN_POINT('Ctrl Pts',(22.9724076658296,48.597794174159,-29.7810944539727));
#19896=CARTESIAN_POINT('Ctrl Pts',(23.0765730195789,49.8043451827873,-29.7184341967097));
#19897=CARTESIAN_POINT('Ctrl Pts',(23.07484016668,49.9974042568772,-29.7084234471775));
#19898=CARTESIAN_POINT('Ctrl Pts',(23.071599139613,49.9974440494104,-30.7915765528225));
#19899=CARTESIAN_POINT('Ctrl Pts',(23.0659001976564,50.7099535886278,-30.7547300790965));
#19900=CARTESIAN_POINT('Ctrl Pts',(22.4655605708053,52.449224872192,-30.6652340976396));
#19901=CARTESIAN_POINT('Ctrl Pts',(19.5796836281861,53.602037241767,-30.5230886084519));
#19902=CARTESIAN_POINT('Ctrl Pts',(16.7540571997694,51.6171559854022,-30.3651400852594));
#19903=CARTESIAN_POINT('Ctrl Pts',(16.8714283874341,48.1660485806496,-30.207191562067));
#19904=CARTESIAN_POINT('Ctrl Pts',(19.825380305008,46.3777291507101,-30.0492430388745));
#19905=CARTESIAN_POINT('Ctrl Pts',(22.5551893154724,47.6897844401465,-29.9107047024597));
#19906=CARTESIAN_POINT('Ctrl Pts',(23.0662108558178,49.3583277363963,-29.8248158737757));
#19907=CARTESIAN_POINT('Ctrl Pts',(23.0699776589026,50.0019420177659,-29.7915765528226));
#19908=CARTESIAN_POINT('Origin',(20.,50.,-42.2084234471774));
#19909=CARTESIAN_POINT('',(23.0783411161508,50.0005689006785,-31.7915765528225));
#19910=CARTESIAN_POINT('',(23.0686853624729,50.0004533262271,-31.7084234471775));
#19911=CARTESIAN_POINT('',(23.0735,50.0000000000002,-42.2084234471774));
#19912=CARTESIAN_POINT('Ctrl Pts',(23.0686853624729,50.0004533262271,-31.7084234471775));
#19913=CARTESIAN_POINT('Ctrl Pts',(23.0693265266791,50.4823621207053,-31.6835616228129));
#19914=CARTESIAN_POINT('Ctrl Pts',(22.7361512606728,51.9839633167782,-31.6060502907174));
#19915=CARTESIAN_POINT('Ctrl Pts',(20.397179025119,53.6046617773376,-31.4758894508912));
#19916=CARTESIAN_POINT('Ctrl Pts',(17.1987558318052,52.3031215376416,-31.3179409276987));
#19917=CARTESIAN_POINT('Ctrl Pts',(16.5401355298036,48.913411046041,-31.1599924045062));
#19918=CARTESIAN_POINT('Ctrl Pts',(19.0184691159077,46.508877711886,-31.0020438813138));
#19919=CARTESIAN_POINT('Ctrl Pts',(22.2283770573404,47.2338735834618,-30.8515208955375));
#19920=CARTESIAN_POINT('Ctrl Pts',(23.0691768887455,49.1310847567491,-30.7536474174921));
#19921=CARTESIAN_POINT('Ctrl Pts',(23.0762467922506,50.0022022521905,-30.7084234471775));
#19922=CARTESIAN_POINT('Ctrl Pts',(23.0783411161508,50.0005689006785,-31.7915765528225));
#19923=CARTESIAN_POINT('Ctrl Pts',(23.0784217978569,50.0319726308292,-31.7899432998789));
#19924=CARTESIAN_POINT('Ctrl Pts',(23.0638169133829,51.0756294932629,-31.7356605392045));
#19925=CARTESIAN_POINT('Ctrl Pts',(21.8880582287126,53.0962193508344,-31.6287282707992));
#19926=CARTESIAN_POINT('Ctrl Pts',(18.4395125322199,53.2735633499893,-31.4707797476067));
#19927=CARTESIAN_POINT('Ctrl Pts',(16.4058133626825,50.4828670206375,-31.3128312244142));
#19928=CARTESIAN_POINT('Ctrl Pts',(17.6308539049556,47.2543698494103,-31.1548827012218));
#19929=CARTESIAN_POINT('Ctrl Pts',(21.0039271572841,46.5152520311566,-30.9969341780293));
#19930=CARTESIAN_POINT('Ctrl Pts',(22.8922343895822,48.371015245975,-30.8758321285629));
#19931=CARTESIAN_POINT('Ctrl Pts',(23.0740433510782,49.6918568021561,-30.8073795868273));
#19932=CARTESIAN_POINT('Ctrl Pts',(23.071599139613,49.9974440494104,-30.7915765528225));
#19933=CARTESIAN_POINT('Origin',(20.,50.,-42.2084234471774));
#19934=CARTESIAN_POINT('',(23.0701085584971,50.0020159667116,-32.7915765528225));
#19935=CARTESIAN_POINT('',(23.0746459871597,49.9973711112026,-32.7084234471775));
#19936=CARTESIAN_POINT('',(23.0735,50.0000000000002,-42.2084234471774));
#19937=CARTESIAN_POINT('Ctrl Pts',(23.0746459871597,49.9973711112026,-32.7084234471775));
#19938=CARTESIAN_POINT('Ctrl Pts',(23.0672842995498,50.8132306194428,-32.6661253358645));
#19939=CARTESIAN_POINT('Ctrl Pts',(22.3159442955655,52.6565958105203,-32.5711777168206));
#19940=CARTESIAN_POINT('Ctrl Pts',(19.2124032663222,53.5399193623716,-32.423580590046));
#19941=CARTESIAN_POINT('Ctrl Pts',(16.6052922900793,51.2756556240609,-32.2656320668535));
#19942=CARTESIAN_POINT('Ctrl Pts',(17.0760595490536,47.8547937287262,-32.1076835436611));
#19943=CARTESIAN_POINT('Ctrl Pts',(20.197874687272,46.378925116056,-31.9497350204686));
#19944=CARTESIAN_POINT('Ctrl Pts',(22.6771342777603,47.9017055273113,-31.8166483216407));
#19945=CARTESIAN_POINT('Ctrl Pts',(23.0679687429807,49.4618311882865,-31.7362111305437));
#19946=CARTESIAN_POINT('Ctrl Pts',(23.0686853624729,50.0004533262271,-31.7084234471775));
#19947=CARTESIAN_POINT('Ctrl Pts',(23.0701085584971,50.0020159667116,-32.7915765528225));
#19948=CARTESIAN_POINT('Ctrl Pts',(23.0723580174886,50.3712206283648,-32.7725070129305));
#19949=CARTESIAN_POINT('Ctrl Pts',(22.840434117996,51.7570397268036,-32.7007879653077));
#19950=CARTESIAN_POINT('Ctrl Pts',(20.7875967467482,53.5399194211172,-32.5764194099539));
#19951=CARTESIAN_POINT('Ctrl Pts',(17.4663957106355,52.5946459196594,-32.4184708867616));
#19952=CARTESIAN_POINT('Ctrl Pts',(16.4423366275984,49.2968858754349,-32.260522363569));
#19953=CARTESIAN_POINT('Ctrl Pts',(18.6439027228774,46.6366180237041,-32.1025738403766));
#19954=CARTESIAN_POINT('Ctrl Pts',(22.0395220029246,47.0218017427905,-31.9462585701277));
#19955=CARTESIAN_POINT('Ctrl Pts',(23.0758209440669,49.0196426425154,-31.8425928076097));
#19956=CARTESIAN_POINT('Ctrl Pts',(23.0783411161508,50.0005689006785,-31.7915765528225));
#19957=CARTESIAN_POINT('Origin',(20.,50.,-42.2084234471774));
#19958=CARTESIAN_POINT('',(23.0714263576006,49.9974846737907,-33.7915765528225));
#19959=CARTESIAN_POINT('',(23.0764186910915,50.0021324681425,-33.7084234471775));
#19960=CARTESIAN_POINT('',(23.0735,50.0000000000002,-42.2084234471774));
#19961=CARTESIAN_POINT('Ctrl Pts',(23.0764186910915,50.0021324681425,-33.7084234471775));
#19962=CARTESIAN_POINT('Ctrl Pts',(23.0775012055128,50.1385838083694,-33.7013385566469));
#19963=CARTESIAN_POINT('Ctrl Pts',(23.0075098506611,51.2879204901039,-33.6416041583855));
#19964=CARTESIAN_POINT('Ctrl Pts',(21.5604874418836,53.2735632956638,-33.5292202523933));
#19965=CARTESIAN_POINT('Ctrl Pts',(18.1119418026202,53.0962192994522,-33.3712717292008));
#19966=CARTESIAN_POINT('Ctrl Pts',(16.3752411082267,50.1116274316806,-33.2133232060084));
#19967=CARTESIAN_POINT('Ctrl Pts',(17.9249990589457,47.0258263665991,-33.0553746828159));
#19968=CARTESIAN_POINT('Ctrl Pts',(21.3560972546178,46.63661807952,-32.8974261596234));
#19969=CARTESIAN_POINT('Ctrl Pts',(22.9680909366565,48.584474643407,-32.7817757477439));
#19970=CARTESIAN_POINT('Ctrl Pts',(23.0764475746156,49.7977100641984,-32.7187748435953));
#19971=CARTESIAN_POINT('Ctrl Pts',(23.0746459871597,49.9973711112026,-32.7084234471775));
#19972=CARTESIAN_POINT('Ctrl Pts',(23.0714263576006,49.9974846737907,-33.7915765528225));
#19973=CARTESIAN_POINT('Ctrl Pts',(23.0658928724823,50.7035076271574,-33.7550707259821));
#19974=CARTESIAN_POINT('Ctrl Pts',(22.4743381873349,52.4361500475419,-33.6659153914109));
#19975=CARTESIAN_POINT('Ctrl Pts',(19.6028209682899,53.6046618371577,-33.5241105491088));
#19976=CARTESIAN_POINT('Ctrl Pts',(16.7645078702952,51.6379648415364,-33.3661620259164));
#19977=CARTESIAN_POINT('Ctrl Pts',(16.8597170832589,48.1861749405428,-33.2082135027238));
#19978=CARTESIAN_POINT('Ctrl Pts',(19.8021253094441,46.3789250559636,-33.0502649795314));
#19979=CARTESIAN_POINT('Ctrl Pts',(22.5470355553875,47.6766081977323,-32.9113859962309));
#19980=CARTESIAN_POINT('Ctrl Pts',(23.0661474372001,49.3518754423758,-32.8251565206613));
#19981=CARTESIAN_POINT('Ctrl Pts',(23.0701085584971,50.0020159667116,-32.7915765528225));
#19982=CARTESIAN_POINT('Origin',(20.,50.,-42.2084234471774));
#19983=CARTESIAN_POINT('',(23.0783900204597,50.0004517332443,-34.7915765528225));
#19984=CARTESIAN_POINT('',(23.06871800645,50.0005575827461,-34.7084234471775));
#19985=CARTESIAN_POINT('',(23.0735,50.0000000000002,-42.2084234471774));
#19986=CARTESIAN_POINT('Ctrl Pts',(23.06871800645,50.0005575827462,-34.7084234471775));
#19987=CARTESIAN_POINT('Ctrl Pts',(23.0694962958913,50.4758508150922,-34.6839022696985));
#19988=CARTESIAN_POINT('Ctrl Pts',(22.7427398646814,51.9706343794756,-34.6067315844887));
#19989=CARTESIAN_POINT('Ctrl Pts',(20.4203163648388,53.6020371819906,-34.4769113915481));
#19990=CARTESIAN_POINT('Ctrl Pts',(17.2136019186591,52.3210608435138,-34.3189628683557));
#19991=CARTESIAN_POINT('Ctrl Pts',(16.5332298683643,48.9356492300977,-34.1610143451631));
#19992=CARTESIAN_POINT('Ctrl Pts',(18.9960728593762,46.5152520889867,-34.0030658219707));
#19993=CARTESIAN_POINT('Ctrl Pts',(22.2178445185897,47.2212162532767,-33.8522021893088));
#19994=CARTESIAN_POINT('Ctrl Pts',(23.0694567832106,49.1245814238351,-33.7539880643777));
#19995=CARTESIAN_POINT('Ctrl Pts',(23.0764186910915,50.0021324681425,-33.7084234471775));
#19996=CARTESIAN_POINT('Ctrl Pts',(23.0783900204597,50.0004517332443,-34.7915765528225));
#19997=CARTESIAN_POINT('Ctrl Pts',(23.0784415067144,50.0253045395665,-34.7902839467645));
#19998=CARTESIAN_POINT('Ctrl Pts',(23.0669562420345,51.062395329507,-34.7363418329757));
#19999=CARTESIAN_POINT('Ctrl Pts',(21.9079001262167,53.0840323039615,-34.6297502114561));
#20000=CARTESIAN_POINT('Ctrl Pts',(18.4605642464159,53.2835157535905,-34.4718016882636));
#20001=CARTESIAN_POINT('Ctrl Pts',(16.4089879445684,50.5059353330574,-34.3138531650712));
#20002=CARTESIAN_POINT('Ctrl Pts',(17.6132730576857,47.2696387333682,-34.1559046418787));
#20003=CARTESIAN_POINT('Ctrl Pts',(20.9815309003809,46.5088776539501,-33.9979561186862));
#20004=CARTESIAN_POINT('Ctrl Pts',(22.8870600694274,48.3576636413843,-33.8765134223341));
#20005=CARTESIAN_POINT('Ctrl Pts',(23.0738733866284,49.6852657693877,-33.8077202337129));
#20006=CARTESIAN_POINT('Ctrl Pts',(23.0714263576006,49.9974846737907,-33.7915765528225));
#20007=CARTESIAN_POINT('Origin',(20.,50.,-42.2084234471774));
#20008=CARTESIAN_POINT('',(23.0702445934797,50.0020868945689,-35.7915765528225));
#20009=CARTESIAN_POINT('',(23.0744507878878,49.9973424352097,-35.7084234471775));
#20010=CARTESIAN_POINT('',(23.0735,50.0000000000002,-42.2084234471774));
#20011=CARTESIAN_POINT('Ctrl Pts',(23.0744507878878,49.9973424352097,-35.7084234471775));
#20012=CARTESIAN_POINT('Ctrl Pts',(23.0671205125675,50.8067638727642,-35.6664659827501));
#20013=CARTESIAN_POINT('Ctrl Pts',(22.3258049686087,52.643754988248,-35.5718590105919));
#20014=CARTESIAN_POINT('Ctrl Pts',(19.2351493190419,53.5449035449308,-35.4246025307029));
#20015=CARTESIAN_POINT('Ctrl Pts',(16.6135532540943,51.2974267394088,-35.2666540075105));
#20016=CARTESIAN_POINT('Ctrl Pts',(17.0623454595379,47.8736125687236,-35.108705484318));
#20017=CARTESIAN_POINT('Ctrl Pts',(20.1746196920941,46.3777292108223,-34.9507569611255));
#20018=CARTESIAN_POINT('Ctrl Pts',(22.6699767186751,47.8884157689623,-34.817329615412));
#20019=CARTESIAN_POINT('Ctrl Pts',(23.0678252278526,49.4553470186378,-34.7365517774293));
#20020=CARTESIAN_POINT('Ctrl Pts',(23.06871800645,50.0005575827462,-34.7084234471775));
#20021=CARTESIAN_POINT('Ctrl Pts',(23.0702445934797,50.0020868945688,-35.7915765528225));
#20022=CARTESIAN_POINT('Ctrl Pts',(23.0725381809387,50.3646558763446,-35.7728476598162));
#20023=CARTESIAN_POINT('Ctrl Pts',(22.8460662390664,51.7436844134824,-35.7014692590789));
#20024=CARTESIAN_POINT('Ctrl Pts',(20.8103103275328,53.5347892888857,-35.5774413506109));
#20025=CARTESIAN_POINT('Ctrl Pts',(17.4831081577191,52.610860700561,-35.4194928274184));
#20026=CARTESIAN_POINT('Ctrl Pts',(16.4378952735367,49.3197441208273,-35.2615443042259));
#20027=CARTESIAN_POINT('Ctrl Pts',(18.6223344083003,46.6453948576666,-35.1035957810335));
#20028=CARTESIAN_POINT('Ctrl Pts',(22.0277620240878,47.0095592424952,-34.946939863899));
#20029=CARTESIAN_POINT('Ctrl Pts',(23.0763444053201,49.0130177639543,-34.8429334544954));
#20030=CARTESIAN_POINT('Ctrl Pts',(23.0783900204597,50.0004517332443,-34.7915765528225));
#20031=CARTESIAN_POINT('Origin',(20.,50.,-42.2084234471774));
#20032=CARTESIAN_POINT('',(23.0712571035372,49.9975291849918,-36.7915765528226));
#20033=CARTESIAN_POINT('',(23.0765863475585,50.0020587540993,-36.7084234471774));
#20034=CARTESIAN_POINT('',(23.0735,50.0000000000002,-42.2084234471774));
#20035=CARTESIAN_POINT('Ctrl Pts',(23.0765863475585,50.0020587540993,-36.7084234471774));
#20036=CARTESIAN_POINT('Ctrl Pts',(23.077590763035,50.1319308950101,-36.7016792035325));
#20037=CARTESIAN_POINT('Ctrl Pts',(23.011370253205,51.2746294458356,-36.6422854521568));
#20038=CARTESIAN_POINT('Ctrl Pts',(21.5814748173496,53.2634759238072,-36.5302421930502));
#20039=CARTESIAN_POINT('Ctrl Pts',(18.1318615437831,53.1082786903842,-36.3722936698577));
#20040=CARTESIAN_POINT('Ctrl Pts',(16.3760325915391,50.1348997013926,-36.2143451466653));
#20041=CARTESIAN_POINT('Ctrl Pts',(17.9059446705936,47.0392112564499,-36.0563966234728));
#20042=CARTESIAN_POINT('Ctrl Pts',(21.3344730289901,46.6279799167075,-35.8984481002803));
#20043=CARTESIAN_POINT('Ctrl Pts',(22.9637255136602,48.5711524990857,-35.7824570415152));
#20044=CARTESIAN_POINT('Ctrl Pts',(23.0763187659037,49.7910771334522,-35.7191154904809));
#20045=CARTESIAN_POINT('Ctrl Pts',(23.0744507878878,49.9973424352097,-35.7084234471775));
#20046=CARTESIAN_POINT('Ctrl Pts',(23.0712571035372,49.9975291849917,-36.7915765528226));
#20047=CARTESIAN_POINT('Ctrl Pts',(23.0658937343458,50.6970615757762,-36.7554113728678));
#20048=CARTESIAN_POINT('Ctrl Pts',(22.4830498332644,52.4230633627457,-36.6665966851821));
#20049=CARTESIAN_POINT('Ctrl Pts',(19.6259746853353,53.6071378153842,-36.5251324897657));
#20050=CARTESIAN_POINT('Ctrl Pts',(16.7750919383154,51.6587061640742,-36.3671839665732));
#20051=CARTESIAN_POINT('Ctrl Pts',(16.8481352521856,48.2063760842456,-36.2092354433807));
#20052=CARTESIAN_POINT('Ctrl Pts',(19.7788784720074,46.3802702566287,-36.0512869201883));
#20053=CARTESIAN_POINT('Ctrl Pts',(22.538817658055,47.6634412853501,-35.9120672900022));
#20054=CARTESIAN_POINT('Ctrl Pts',(23.0660905894759,49.3454243391448,-35.825497167547));
#20055=CARTESIAN_POINT('Ctrl Pts',(23.0702445934797,50.0020868945688,-35.7915765528225));
#20056=CARTESIAN_POINT('Origin',(20.,50.,-42.2084234471774));
#20057=CARTESIAN_POINT('',(23.0784282759302,50.0003336412877,-37.7915765528226));
#20058=CARTESIAN_POINT('',(23.0687573797509,50.0006610025294,-37.7084234471775));
#20059=CARTESIAN_POINT('',(23.0735,50.0000000000002,-42.2084234471774));
#20060=CARTESIAN_POINT('Ctrl Pts',(23.0687573797509,50.0006610025294,-37.7084234471775));
#20061=CARTESIAN_POINT('Ctrl Pts',(23.0696679145195,50.4693364673409,-37.6842429165841));
#20062=CARTESIAN_POINT('Ctrl Pts',(22.7492703636569,51.9573025041246,-37.60741287826));
#20063=CARTESIAN_POINT('Ctrl Pts',(20.4434363727656,53.5992640406764,-37.477933332205));
#20064=CARTESIAN_POINT('Ctrl Pts',(17.2285628888723,52.338904470578,-37.3199848090125));
#20065=CARTESIAN_POINT('Ctrl Pts',(16.5264671400482,48.9579312880643,-37.1620362858201));
#20066=CARTESIAN_POINT('Ctrl Pts',(18.9737179946959,46.5217701454759,-37.0040877626275));
#20067=CARTESIAN_POINT('Ctrl Pts',(22.2072410095807,47.2085800678294,-36.8528834830801));
#20068=CARTESIAN_POINT('Ctrl Pts',(23.0697497087703,49.1180730561048,-36.7543287112633));
#20069=CARTESIAN_POINT('Ctrl Pts',(23.0765863475585,50.0020587540993,-36.7084234471774));
#20070=CARTESIAN_POINT('Ctrl Pts',(23.0784282759302,50.0003336412877,-37.7915765528226));
#20071=CARTESIAN_POINT('Ctrl Pts',(23.0784567206548,50.0186362554802,-37.7906245936502));
#20072=CARTESIAN_POINT('Ctrl Pts',(23.0700522648677,51.0491651533383,-37.737023126747));
#20073=CARTESIAN_POINT('Ctrl Pts',(21.9276631892634,53.0717178847477,-37.6307721521129));
#20074=CARTESIAN_POINT('Ctrl Pts',(18.4816795176051,53.2933328888968,-37.4728236289205));
#20075=CARTESIAN_POINT('Ctrl Pts',(16.4123105391071,50.5289827307422,-37.314875105728));
#20076=CARTESIAN_POINT('Ctrl Pts',(17.595790636172,47.2850202168804,-37.1569265825356));
#20077=CARTESIAN_POINT('Ctrl Pts',(20.959094164331,46.5026472005525,-36.9989780593431));
#20078=CARTESIAN_POINT('Ctrl Pts',(22.8818333151723,48.3443111113272,-36.8771947161054));
#20079=CARTESIAN_POINT('Ctrl Pts',(23.0737017626221,49.6786777031506,-36.8080608805986));
#20080=CARTESIAN_POINT('Ctrl Pts',(23.0712571035372,49.9975291849917,-36.7915765528226));
#20081=CARTESIAN_POINT('Origin',(20.,50.,-42.2084234471774));
#20082=CARTESIAN_POINT('',(23.0703815974152,50.0021496035415,-38.7915765528225));
#20083=CARTESIAN_POINT('',(23.074254699799,49.9973154728993,-38.7084234471774));
#20084=CARTESIAN_POINT('',(23.0735,50.0000000000002,-42.2084234471774));
#20085=CARTESIAN_POINT('Ctrl Pts',(23.074254699799,49.9973154728993,-38.7084234471775));
#20086=CARTESIAN_POINT('Ctrl Pts',(23.0669677154469,50.8002971404021,-38.6668066296357));
#20087=CARTESIAN_POINT('Ctrl Pts',(22.3355967751289,52.6309008896528,-38.5725403043632));
#20088=CARTESIAN_POINT('Ctrl Pts',(19.257926763209,53.5497393781131,-38.4256244713598));
#20089=CARTESIAN_POINT('Ctrl Pts',(16.6219539119773,51.3191454645357,-38.2676759481674));
#20090=CARTESIAN_POINT('Ctrl Pts',(17.0487524523756,47.8925185252508,-38.1097274249749));
#20091=CARTESIAN_POINT('Ctrl Pts',(20.1513575155428,46.3766829286487,-37.9517789017824));
#20092=CARTESIAN_POINT('Ctrl Pts',(22.6627586022493,47.87513118127,-37.8180109091833));
#20093=CARTESIAN_POINT('Ctrl Pts',(23.0676853605324,49.4488653733505,-37.736892424315));
#20094=CARTESIAN_POINT('Ctrl Pts',(23.0687573797509,50.0006610025294,-37.7084234471775));
#20095=CARTESIAN_POINT('Ctrl Pts',(23.0703815974152,50.0021496035415,-38.7915765528225));
#20096=CARTESIAN_POINT('Ctrl Pts',(23.0727173594958,50.3580876206747,-38.7731883067018));
#20097=CARTESIAN_POINT('Ctrl Pts',(22.8516585980335,51.7303472925322,-38.7021505528502));
#20098=CARTESIAN_POINT('Ctrl Pts',(20.8329797652707,53.529499797304,-38.5784632912678));
#20099=CARTESIAN_POINT('Ctrl Pts',(17.4999297672036,52.6269746785947,-38.4205147680753));
#20100=CARTESIAN_POINT('Ctrl Pts',(16.4335980754498,49.3426269761734,-38.2625662448828));
#20101=CARTESIAN_POINT('Ctrl Pts',(18.6008242547947,46.6543117271026,-38.1046177216904));
#20102=CARTESIAN_POINT('Ctrl Pts',(22.0159279395425,46.9973440896119,-37.9476211576703));
#20103=CARTESIAN_POINT('Ctrl Pts',(23.0768835431613,49.0063831511548,-37.843274101381));
#20104=CARTESIAN_POINT('Ctrl Pts',(23.0784282759302,50.0003336412877,-37.7915765528226));
#20105=CARTESIAN_POINT('Origin',(20.,50.,-42.2084234471774));
#20106=CARTESIAN_POINT('',(23.0703066071761,49.9966560053347,-39.7915765528225));
#20107=CARTESIAN_POINT('',(23.0767446582541,50.0019103494728,-39.7084234471775));
#20108=CARTESIAN_POINT('',(23.0735,50.0000000000002,-42.2084234471774));
#20109=CARTESIAN_POINT('',(20.7937992825328,47.0307770462543,-40.));
#20110=CARTESIAN_POINT('Ctrl Pts',(20.7937992825328,47.0307770462543,-40.));
#20111=CARTESIAN_POINT('Ctrl Pts',(21.7760378723045,47.2933710986319,-39.9473504922692));
#20112=CARTESIAN_POINT('Ctrl Pts',(22.8758107695838,48.3306052064221,-39.8778760098767));
#20113=CARTESIAN_POINT('Ctrl Pts',(23.0726593916611,49.6711328391077,-39.8084015274842));
#20114=CARTESIAN_POINT('Ctrl Pts',(23.0703066071761,49.9966560053347,-39.7915765528225));
#20115=CARTESIAN_POINT('',(19.2043380770546,47.0257135261044,-40.));
#20116=CARTESIAN_POINT('Origin',(20.,50.,-40.));
#20117=CARTESIAN_POINT('Ctrl Pts',(19.2043342004084,47.0257029875827,-40.));
#20118=CARTESIAN_POINT('Ctrl Pts',(20.1513502732183,46.7747743426961,-39.9490537266973));
#20119=CARTESIAN_POINT('Ctrl Pts',(22.2116706660287,47.2298902467823,-39.8518615424231));
#20120=CARTESIAN_POINT('Ctrl Pts',(23.0700633101723,49.111677598951,-39.754669358149));
#20121=CARTESIAN_POINT('Ctrl Pts',(23.0767446582541,50.0019103494728,-39.7084234471775));
#20122=CARTESIAN_POINT('Origin',(-20.,50.,-32.));
#20123=CARTESIAN_POINT('',(-17.486538471654,50.0002728803002,-25.387416697508));
#20124=CARTESIAN_POINT('',(-17.4842348936637,49.9966178726365,-25.112583302492));
#20125=CARTESIAN_POINT('',(-17.4825,50.,-32.));
#20126=CARTESIAN_POINT('',(-18.0865340033349,51.6359872033749,-25.));
#20127=CARTESIAN_POINT('Ctrl Pts',(-17.4842348936637,49.9966178726365,-25.112583302492));
#20128=CARTESIAN_POINT('Ctrl Pts',(-17.4894449388897,50.5891792000144,-25.0750555349946));
#20129=CARTESIAN_POINT('Ctrl Pts',(-17.7007781719159,51.1848035603044,-25.0375277674973));
#20130=CARTESIAN_POINT('Ctrl Pts',(-18.0865340033349,51.6359872033749,-25.));
#20131=CARTESIAN_POINT('',(-17.4825,50.,-25.));
#20132=CARTESIAN_POINT('Origin',(-20.,50.,-25.));
#20133=CARTESIAN_POINT('',(-17.4825,50.,-24.));
#20134=CARTESIAN_POINT('',(-17.4825,50.,-32.));
#20135=CARTESIAN_POINT('Origin',(-20.,50.,-24.));
#20136=CARTESIAN_POINT('',(-21.9170729057076,51.63854067126,-25.));
#20137=CARTESIAN_POINT('Origin',(-20.,50.,-25.));
#20138=CARTESIAN_POINT('Ctrl Pts',(-21.9170804273993,51.6385459961512,-25.));
#20139=CARTESIAN_POINT('Ctrl Pts',(-21.3942486355313,52.2473162151012,-25.0509462733027));
#20140=CARTESIAN_POINT('Ctrl Pts',(-20.5545527314147,52.587362362996,-25.1018925466053));
#20141=CARTESIAN_POINT('Ctrl Pts',(-19.7559044795804,52.5095736846299,-25.152838819908));
#20142=CARTESIAN_POINT('Ctrl Pts',(-18.9305558410379,52.4291843772771,-25.2054883276388));
#20143=CARTESIAN_POINT('Ctrl Pts',(-18.1490453416046,51.902555145838,-25.2581378353696));
#20144=CARTESIAN_POINT('Ctrl Pts',(-17.7651664494765,51.1677990620503,-25.3107873431005));
#20145=CARTESIAN_POINT('Ctrl Pts',(-17.5789260777408,50.8113292248548,-25.3363304612363));
#20146=CARTESIAN_POINT('Ctrl Pts',(-17.4862780001353,50.4058716582546,-25.3618735793722));
#20147=CARTESIAN_POINT('Ctrl Pts',(-17.486538471654,50.0002728803002,-25.387416697508));
#20148=CARTESIAN_POINT('Origin',(-20.,50.,-32.));
#20149=CARTESIAN_POINT('',(-17.4812439066724,49.9979044740549,-26.387416697508));
#20150=CARTESIAN_POINT('',(-17.4786409565,50.0006703257771,-26.112583302492));
#20151=CARTESIAN_POINT('',(-17.4825,50.,-32.));
#20152=CARTESIAN_POINT('Ctrl Pts',(-17.4786409565,50.0006703257771,-26.112583302492));
#20153=CARTESIAN_POINT('Ctrl Pts',(-17.4785131615273,50.0371266681365,-26.1102687557771));
#20154=CARTESIAN_POINT('Ctrl Pts',(-17.4792361426369,50.0735777564612,-26.1079542090622));
#20155=CARTESIAN_POINT('Ctrl Pts',(-17.480825778613,50.1099909286062,-26.1056396623473));
#20156=CARTESIAN_POINT('Ctrl Pts',(-17.516985580908,50.9382894356126,-26.0529901546164));
#20157=CARTESIAN_POINT('Ctrl Pts',(-18.0015839011493,51.7469687422497,-26.0003406468856));
#20158=CARTESIAN_POINT('Ctrl Pts',(-18.7149419927441,52.1695268891006,-25.9476911391548));
#20159=CARTESIAN_POINT('Ctrl Pts',(-19.428300084339,52.5920850359516,-25.895041631424));
#20160=CARTESIAN_POINT('Ctrl Pts',(-20.3704179472873,52.6285220230163,-25.8423921236931));
#20161=CARTESIAN_POINT('Ctrl Pts',(-21.1141877771953,52.2621196062368,-25.7897426159623));
#20162=CARTESIAN_POINT('Ctrl Pts',(-21.8579576071032,51.8957171894573,-25.7370931082315));
#20163=CARTESIAN_POINT('Ctrl Pts',(-22.4033794039707,51.1264753688335,-25.6844436005007));
#20164=CARTESIAN_POINT('Ctrl Pts',(-22.503220283497,50.3035167497657,-25.6317940927699));
#20165=CARTESIAN_POINT('Ctrl Pts',(-22.6030611630233,49.4805581306978,-25.5791445850391));
#20166=CARTESIAN_POINT('Ctrl Pts',(-22.2573211252084,48.603882713186,-25.5264950773082));
#20167=CARTESIAN_POINT('Ctrl Pts',(-21.62268585804,48.0701218881779,-25.4738455695774));
#20168=CARTESIAN_POINT('Ctrl Pts',(-20.9880505908716,47.5363610631698,-25.4211960618466));
#20169=CARTESIAN_POINT('Ctrl Pts',(-20.0645200943497,47.3455148306655,-25.3685465541157));
#20170=CARTESIAN_POINT('Ctrl Pts',(-19.2708510806944,47.5857187630522,-25.3158970463849));
#20171=CARTESIAN_POINT('Ctrl Pts',(-18.4771820670391,47.8259226954389,-25.2632475386541));
#20172=CARTESIAN_POINT('Ctrl Pts',(-17.8133745362502,48.4971767927166,-25.2105980309233));
#20173=CARTESIAN_POINT('Ctrl Pts',(-17.5804136737438,49.2914461181452,-25.1579485231925));
#20174=CARTESIAN_POINT('Ctrl Pts',(-17.5135037670946,49.5195723615276,-25.142826782959));
#20175=CARTESIAN_POINT('Ctrl Pts',(-17.4821355161689,49.7578464491655,-25.1277050427255));
#20176=CARTESIAN_POINT('Ctrl Pts',(-17.4842348936637,49.9966178726365,-25.112583302492));
#20177=CARTESIAN_POINT('Ctrl Pts',(-17.486538471654,50.0002728803002,-25.387416697508));
#20178=CARTESIAN_POINT('Ctrl Pts',(-17.4868148843623,49.5698509390166,-25.414523087103));
#20179=CARTESIAN_POINT('Ctrl Pts',(-17.5917200878965,49.1392699728275,-25.4416294766979));
#20180=CARTESIAN_POINT('Ctrl Pts',(-17.8004369592101,48.7669049830551,-25.4687358662929));
#20181=CARTESIAN_POINT('Ctrl Pts',(-18.2058336458947,48.0436499239839,-25.5213853740237));
#20182=CARTESIAN_POINT('Ctrl Pts',(-19.0028743040869,47.5400227419779,-25.5740348817546));
#20183=CARTESIAN_POINT('Ctrl Pts',(-19.8301086827711,47.4841780405205,-25.6266843894854));
#20184=CARTESIAN_POINT('Ctrl Pts',(-20.6573430614552,47.428333339063,-25.6793338972162));
#20185=CARTESIAN_POINT('Ctrl Pts',(-21.5147711606312,47.8202711181543,-25.731983404947));
#20186=CARTESIAN_POINT('Ctrl Pts',(-22.0137532550528,48.4823912426514,-25.7846329126778));
#20187=CARTESIAN_POINT('Ctrl Pts',(-22.5127353494744,49.1445113671485,-25.8372824204087));
#20188=CARTESIAN_POINT('Ctrl Pts',(-22.6532714391415,50.0768138370515,-25.8899319281395));
#20189=CARTESIAN_POINT('Ctrl Pts',(-22.371620355899,50.8566138838869,-25.9425814358703));
#20190=CARTESIAN_POINT('Ctrl Pts',(-22.0899692726565,51.6364139307222,-25.9952309436011));
#20191=CARTESIAN_POINT('Ctrl Pts',(-21.3861310165042,52.2637115544899,-26.047880451332));
#20192=CARTESIAN_POINT('Ctrl Pts',(-20.5791956609239,52.4541508141935,-26.1005299590628));
#20193=CARTESIAN_POINT('Ctrl Pts',(-19.7722603053436,52.6445900738971,-26.1531794667936));
#20194=CARTESIAN_POINT('Ctrl Pts',(-18.8622278503352,52.3981709695366,-26.2058289745244));
#20195=CARTESIAN_POINT('Ctrl Pts',(-18.2616397845884,51.8265938623424,-26.2584784822552));
#20196=CARTESIAN_POINT('Ctrl Pts',(-17.7713613588437,51.3599979702671,-26.3014578873395));
#20197=CARTESIAN_POINT('Ctrl Pts',(-17.487295335698,50.6767181914727,-26.3444372924237));
#20198=CARTESIAN_POINT('Ctrl Pts',(-17.4812439066724,49.9979044740549,-26.387416697508));
#20199=CARTESIAN_POINT('Origin',(-20.,50.,-32.));
#20200=CARTESIAN_POINT('',(-17.4803937907486,50.0018577149014,-27.387416697508));
#20201=CARTESIAN_POINT('',(-17.4854881593906,50.0015280028117,-27.112583302492));
#20202=CARTESIAN_POINT('',(-17.4825,50.,-32.));
#20203=CARTESIAN_POINT('Ctrl Pts',(-17.4854881593906,50.0015280028117,-27.112583302492));
#20204=CARTESIAN_POINT('Ctrl Pts',(-17.4837319359023,50.314813245317,-27.0928324688287));
#20205=CARTESIAN_POINT('Ctrl Pts',(-17.5380280717696,50.627511664655,-27.0730816351654));
#20206=CARTESIAN_POINT('Ctrl Pts',(-17.651165447386,50.9172321802462,-27.0533308015021));
#20207=CARTESIAN_POINT('Ctrl Pts',(-17.9527540908682,51.6895359110876,-27.0006812937713));
#20208=CARTESIAN_POINT('Ctrl Pts',(-18.6724614246153,52.2985614536939,-26.9480317860404));
#20209=CARTESIAN_POINT('Ctrl Pts',(-19.4840191783241,52.46821795488,-26.8953822783096));
#20210=CARTESIAN_POINT('Ctrl Pts',(-20.2955769320328,52.6378744560661,-26.8427327705788));
#20211=CARTESIAN_POINT('Ctrl Pts',(-21.1989851057032,52.368161915832,-26.790083262848));
#20212=CARTESIAN_POINT('Ctrl Pts',(-21.7846971327504,51.7813471975056,-26.7374337551172));
#20213=CARTESIAN_POINT('Ctrl Pts',(-22.3704091597975,51.1945324791791,-26.6847842473863));
#20214=CARTESIAN_POINT('Ctrl Pts',(-22.6384250402214,50.2906155827604,-26.6321347396555));
#20215=CARTESIAN_POINT('Ctrl Pts',(-22.4672442663634,49.4793798880915,-26.5794852319247));
#20216=CARTESIAN_POINT('Ctrl Pts',(-22.2960634925054,48.6681441934227,-26.5268357241938));
#20217=CARTESIAN_POINT('Ctrl Pts',(-21.6856860643655,47.9495897005038,-26.474186216463));
#20218=CARTESIAN_POINT('Ctrl Pts',(-20.9128164788615,47.6494494205881,-26.4215367087322));
#20219=CARTESIAN_POINT('Ctrl Pts',(-20.1399468933575,47.3493091406725,-26.3688872010014));
#20220=CARTESIAN_POINT('Ctrl Pts',(-19.2045851504892,47.4675830737602,-26.3162376932706));
#20221=CARTESIAN_POINT('Ctrl Pts',(-18.5307649212294,47.950678893992,-26.2635881855397));
#20222=CARTESIAN_POINT('Ctrl Pts',(-17.8865667808605,48.4125371397071,-26.2132532245238));
#20223=CARTESIAN_POINT('Ctrl Pts',(-17.4814201421296,49.2078461586818,-26.1629182635079));
#20224=CARTESIAN_POINT('Ctrl Pts',(-17.4786409565,50.0006703257771,-26.112583302492));
#20225=CARTESIAN_POINT('Ctrl Pts',(-17.4812439066724,49.9979044740549,-26.387416697508));
#20226=CARTESIAN_POINT('Ctrl Pts',(-17.4798823722417,49.8451755492952,-26.3970868001546));
#20227=CARTESIAN_POINT('Ctrl Pts',(-17.4925945596475,49.6926727065716,-26.4067569028011));
#20228=CARTESIAN_POINT('Ctrl Pts',(-17.5201982738737,49.5429147761019,-26.4164270054477));
#20229=CARTESIAN_POINT('Ctrl Pts',(-17.6704885053911,48.7275479070835,-26.4690765131785));
#20230=CARTESIAN_POINT('Ctrl Pts',(-18.2622126449111,47.9935492790746,-26.5217260209094));
#20231=CARTESIAN_POINT('Ctrl Pts',(-19.0271195631323,47.6736634881809,-26.5743755286402));
#20232=CARTESIAN_POINT('Ctrl Pts',(-19.7920264813536,47.3537776972871,-26.627025036371));
#20233=CARTESIAN_POINT('Ctrl Pts',(-20.7301161782762,47.4480047435085,-26.6796745441018));
#20234=CARTESIAN_POINT('Ctrl Pts',(-21.4161209539682,47.9136294939318,-26.7323240518326));
#20235=CARTESIAN_POINT('Ctrl Pts',(-22.1021257296601,48.379254244355,-26.7849735595635));
#20236=CARTESIAN_POINT('Ctrl Pts',(-22.5360455841214,49.21627669898,-26.8376230672943));
#20237=CARTESIAN_POINT('Ctrl Pts',(-22.5211690482687,50.0452448208666,-26.8902725750251));
#20238=CARTESIAN_POINT('Ctrl Pts',(-22.5062925124159,50.8742129427532,-26.9429220827559));
#20239=CARTESIAN_POINT('Ctrl Pts',(-22.0426195862492,51.6951267319013,-26.9955715904868));
#20240=CARTESIAN_POINT('Ctrl Pts',(-21.3403495917614,52.1358377246691,-27.0482210982176));
#20241=CARTESIAN_POINT('Ctrl Pts',(-20.6380795972737,52.5765487174368,-27.1008706059484));
#20242=CARTESIAN_POINT('Ctrl Pts',(-19.6972125344649,52.6370569138241,-27.1535201136792));
#20243=CARTESIAN_POINT('Ctrl Pts',(-18.9442760521657,52.2899316828412,-27.2061696214101));
#20244=CARTESIAN_POINT('Ctrl Pts',(-18.1913395698665,51.9428064518583,-27.2588191291409));
#20245=CARTESIAN_POINT('Ctrl Pts',(-17.6263336680768,51.1880477935053,-27.3114686368717));
#20246=CARTESIAN_POINT('Ctrl Pts',(-17.5053952439644,50.3678141485724,-27.3641181446025));
#20247=CARTESIAN_POINT('Ctrl Pts',(-17.4875559491389,50.2468237360945,-27.3718843289044));
#20248=CARTESIAN_POINT('Ctrl Pts',(-17.4793788476514,50.1244086933274,-27.3796505132062));
#20249=CARTESIAN_POINT('Ctrl Pts',(-17.4803937907486,50.0018577149014,-27.387416697508));
#20250=CARTESIAN_POINT('Origin',(-20.,50.,-32.));
#20251=CARTESIAN_POINT('',(-17.4864645688206,50.0002853817988,-28.387416697508));
#20252=CARTESIAN_POINT('',(-17.4839128694198,49.9978763966856,-28.112583302492));
#20253=CARTESIAN_POINT('',(-17.4825,50.,-32.));
#20254=CARTESIAN_POINT('Ctrl Pts',(-17.4839128694198,49.9978763966856,-28.112583302492));
#20255=CARTESIAN_POINT('Ctrl Pts',(-17.4887122405414,50.5868019954094,-28.0753961818803));
#20256=CARTESIAN_POINT('Ctrl Pts',(-17.6952667199242,51.1787611136952,-28.0382090612686));
#20257=CARTESIAN_POINT('Ctrl Pts',(-18.0729549030142,51.6262950181732,-28.0010219406569));
#20258=CARTESIAN_POINT('Ctrl Pts',(-18.607685653563,52.2599133079476,-27.9483724329261));
#20259=CARTESIAN_POINT('Ctrl Pts',(-19.4854519104968,52.6040329467834,-27.8957229251952));
#20260=CARTESIAN_POINT('Ctrl Pts',(-20.3083316909491,52.5026525553353,-27.8430734174644));
#20261=CARTESIAN_POINT('Ctrl Pts',(-21.1312114714014,52.4012721638872,-27.7904239097336));
#20262=CARTESIAN_POINT('Ctrl Pts',(-21.8992047753722,51.8543917421554,-27.7377744020028));
#20263=CARTESIAN_POINT('Ctrl Pts',(-22.2641535138776,51.1099311613503,-27.685124894272));
#20264=CARTESIAN_POINT('Ctrl Pts',(-22.6291022523829,50.3654705805453,-27.6324753865411));
#20265=CARTESIAN_POINT('Ctrl Pts',(-22.5910064254228,49.4234298406672,-27.5798258788103));
#20266=CARTESIAN_POINT('Ctrl Pts',(-22.1671362035201,48.7108688885658,-27.5271763710795));
#20267=CARTESIAN_POINT('Ctrl Pts',(-21.7432659816174,47.9983079364644,-27.4745268633487));
#20268=CARTESIAN_POINT('Ctrl Pts',(-20.9336213647721,47.5152267721397,-27.4218773556178));
#20269=CARTESIAN_POINT('Ctrl Pts',(-20.1052424146065,47.4806226905502,-27.369227847887));
#20270=CARTESIAN_POINT('Ctrl Pts',(-19.2768634644409,47.4460186089606,-27.3165783401562));
#20271=CARTESIAN_POINT('Ctrl Pts',(-18.429750180955,47.8598916101062,-27.2639288324254));
#20272=CARTESIAN_POINT('Ctrl Pts',(-17.9479285158207,48.5346190702172,-27.2112793246946));
#20273=CARTESIAN_POINT('Ctrl Pts',(-17.6468564905899,48.9562305866647,-27.178380650627));
#20274=CARTESIAN_POINT('Ctrl Pts',(-17.488413475107,49.4796933674211,-27.1454819765595));
#20275=CARTESIAN_POINT('Ctrl Pts',(-17.4854881593906,50.0015280028117,-27.112583302492));
#20276=CARTESIAN_POINT('Ctrl Pts',(-17.4803937907486,50.0018577149014,-27.387416697508));
#20277=CARTESIAN_POINT('Ctrl Pts',(-17.4862594794222,49.2935954605613,-27.432300020937));
#20278=CARTESIAN_POINT('Ctrl Pts',(-17.7991452273176,48.5807928698821,-27.477183344366));
#20279=CARTESIAN_POINT('Ctrl Pts',(-18.3282967300838,48.1122107528984,-27.522066667795));
#20280=CARTESIAN_POINT('Ctrl Pts',(-18.9490075867506,47.5625496336702,-27.5747161755258));
#20281=CARTESIAN_POINT('Ctrl Pts',(-19.8673002465193,47.3489360267268,-27.6273656832566));
#20282=CARTESIAN_POINT('Ctrl Pts',(-20.6668807124105,47.5682084326959,-27.6800151909875));
#20283=CARTESIAN_POINT('Ctrl Pts',(-21.4664611783018,47.7874808386649,-27.7326646987183));
#20284=CARTESIAN_POINT('Ctrl Pts',(-22.1473294503157,48.4396392575466,-27.7853142064491));
#20285=CARTESIAN_POINT('Ctrl Pts',(-22.4008242431245,49.2290375771959,-27.8379637141799));
#20286=CARTESIAN_POINT('Ctrl Pts',(-22.6543190359332,50.0184358968453,-27.8906132219108));
#20287=CARTESIAN_POINT('Ctrl Pts',(-22.4804403495369,50.9450741172625,-27.9432627296416));
#20288=CARTESIAN_POINT('Ctrl Pts',(-21.9580134463135,51.5888748975553,-27.9959122373724));
#20289=CARTESIAN_POINT('Ctrl Pts',(-21.4355865430901,52.232675677848,-28.0485617451032));
#20290=CARTESIAN_POINT('Ctrl Pts',(-20.5646114230397,52.5936390180164,-28.1012112528341));
#20291=CARTESIAN_POINT('Ctrl Pts',(-19.7399314100524,52.5081276743256,-28.1538607605649));
#20292=CARTESIAN_POINT('Ctrl Pts',(-18.915251397065,52.4226163306348,-28.2065102682957));
#20293=CARTESIAN_POINT('Ctrl Pts',(-18.1368664911408,51.8906303030848,-28.2591597760265));
#20294=CARTESIAN_POINT('Ctrl Pts',(-17.7576456536461,51.153337368745,-28.3118092837573));
#20295=CARTESIAN_POINT('Ctrl Pts',(-17.5761187473869,50.8004071177026,-28.3370117550076));
#20296=CARTESIAN_POINT('Ctrl Pts',(-17.4860556044377,50.4004331976185,-28.3622142262578));
#20297=CARTESIAN_POINT('Ctrl Pts',(-17.4864645688206,50.0002853817988,-28.387416697508));
#20298=CARTESIAN_POINT('Origin',(-20.,50.,-32.));
#20299=CARTESIAN_POINT('',(-17.4814019803852,49.9978738298142,-29.387416697508));
#20300=CARTESIAN_POINT('',(-17.4785832788205,50.0005609135351,-29.112583302492));
#20301=CARTESIAN_POINT('',(-17.4825,50.,-32.));
#20302=CARTESIAN_POINT('Ctrl Pts',(-17.4785832788205,50.0005609135351,-29.112583302492));
#20303=CARTESIAN_POINT('Ctrl Pts',(-17.4784885568277,50.0316502572541,-29.1106094026627));
#20304=CARTESIAN_POINT('Ctrl Pts',(-17.4790143481923,50.0627363235243,-29.1086355028334));
#20305=CARTESIAN_POINT('Ctrl Pts',(-17.4801706320494,50.093798920144,-29.1066616030042));
#20306=CARTESIAN_POINT('Ctrl Pts',(-17.5110120025032,50.9223264860409,-29.0540120952733));
#20307=CARTESIAN_POINT('Ctrl Pts',(-17.9904110877069,51.734156798706,-29.0013625875425));
#20308=CARTESIAN_POINT('Ctrl Pts',(-18.7010396025018,52.1612589310346,-28.9487130798117));
#20309=CARTESIAN_POINT('Ctrl Pts',(-19.4116681172968,52.5883610633633,-28.8960635720809));
#20310=CARTESIAN_POINT('Ctrl Pts',(-20.3535260616831,52.6307350153553,-28.84341406435));
#20311=CARTESIAN_POINT('Ctrl Pts',(-21.0996364592575,52.269171200665,-28.7907645566192));
#20312=CARTESIAN_POINT('Ctrl Pts',(-21.8457468568319,51.9076073859748,-28.7381150488884));
#20313=CARTESIAN_POINT('Ctrl Pts',(-22.3961097075944,51.1421058046023,-28.6854655411576));
#20314=CARTESIAN_POINT('Ctrl Pts',(-22.5012263823627,50.3196949567933,-28.6328160334268));
#20315=CARTESIAN_POINT('Ctrl Pts',(-22.606343057131,49.4972841089843,-28.580166525696));
#20316=CARTESIAN_POINT('Ctrl Pts',(-22.2662135559049,48.6179639947387,-28.5275170179651));
#20317=CARTESIAN_POINT('Ctrl Pts',(-21.6350304158872,48.0803610178466,-28.4748675102343));
#20318=CARTESIAN_POINT('Ctrl Pts',(-21.0038472758696,47.5427580409546,-28.4222180025035));
#20319=CARTESIAN_POINT('Ctrl Pts',(-20.0816104970603,47.3468722014163,-28.3695684947726));
#20320=CARTESIAN_POINT('Ctrl Pts',(-19.2864020986368,47.5815053624962,-28.3169189870418));
#20321=CARTESIAN_POINT('Ctrl Pts',(-18.4911937002134,47.8161385235761,-28.264269479311));
#20322=CARTESIAN_POINT('Ctrl Pts',(-17.8230136821757,48.4812906852744,-28.2116199715802));
#20323=CARTESIAN_POINT('Ctrl Pts',(-17.5847712952388,49.27542523648,-28.1589704638494));
#20324=CARTESIAN_POINT('Ctrl Pts',(-17.5148030054337,49.5086508901404,-28.1435080767302));
#20325=CARTESIAN_POINT('Ctrl Pts',(-17.4819172931829,49.7530014119585,-28.1280456896111));
#20326=CARTESIAN_POINT('Ctrl Pts',(-17.4839128694198,49.9978763966856,-28.112583302492));
#20327=CARTESIAN_POINT('Ctrl Pts',(-17.4864645688206,50.0002853817988,-28.387416697508));
#20328=CARTESIAN_POINT('Ctrl Pts',(-17.4869099561092,49.5644998753144,-28.4148637339886));
#20329=CARTESIAN_POINT('Ctrl Pts',(-17.5946601977475,49.1285081190019,-28.4423107704692));
#20330=CARTESIAN_POINT('Ctrl Pts',(-17.8084343854675,48.752851148744,-28.4697578069498));
#20331=CARTESIAN_POINT('Ctrl Pts',(-18.2185007238488,48.0322577042129,-28.5224073146806));
#20332=CARTESIAN_POINT('Ctrl Pts',(-19.0186901696765,47.5336706562804,-28.5750568224115));
#20333=CARTESIAN_POINT('Ctrl Pts',(-19.8462490062726,47.4831168615326,-28.6277063301423));
#20334=CARTESIAN_POINT('Ctrl Pts',(-20.6738078428688,47.4325630667848,-28.6803558378731));
#20335=CARTESIAN_POINT('Ctrl Pts',(-21.5287360702333,47.8300425252218,-28.7330053456039));
#20336=CARTESIAN_POINT('Ctrl Pts',(-22.0234649770947,48.4953639685932,-28.7856548533347));
#20337=CARTESIAN_POINT('Ctrl Pts',(-22.5181938839562,49.1606854119646,-28.8383043610656));
#20338=CARTESIAN_POINT('Ctrl Pts',(-22.6527234703146,50.0938488402703,-28.8909538687964));
#20339=CARTESIAN_POINT('Ctrl Pts',(-22.3660667940254,50.8718188038116,-28.9436033765272));
#20340=CARTESIAN_POINT('Ctrl Pts',(-22.0794101177362,51.6497887673529,-28.996252884258));
#20341=CARTESIAN_POINT('Ctrl Pts',(-21.3715671787995,52.2725652661297,-29.0489023919889));
#20342=CARTESIAN_POINT('Ctrl Pts',(-20.5634278095146,52.4578220448258,-29.1015518997197));
#20343=CARTESIAN_POINT('Ctrl Pts',(-19.7552884402297,52.6430788235219,-29.1542014074505));
#20344=CARTESIAN_POINT('Ctrl Pts',(-18.8468526405967,52.3908158821372,-29.2068509151813));
#20345=CARTESIAN_POINT('Ctrl Pts',(-18.2499459659827,51.8153927890541,-29.2595004229121));
#20346=CARTESIAN_POINT('Ctrl Pts',(-17.766534810533,51.3493803383144,-29.3021391811108));
#20347=CARTESIAN_POINT('Ctrl Pts',(-17.4874475323917,50.6714155213793,-29.3447779393094));
#20348=CARTESIAN_POINT('Ctrl Pts',(-17.4814019803852,49.9978738298142,-29.387416697508));
#20349=CARTESIAN_POINT('Origin',(-20.,50.,-32.));
#20350=CARTESIAN_POINT('',(-17.4802498150093,50.0018038622189,-30.387416697508));
#20351=CARTESIAN_POINT('',(-17.4853852564016,50.0015907042489,-30.112583302492));
#20352=CARTESIAN_POINT('',(-17.4825,50.,-32.));
#20353=CARTESIAN_POINT('Ctrl Pts',(-17.4853852564016,50.0015907042489,-30.112583302492));
#20354=CARTESIAN_POINT('Ctrl Pts',(-17.483583538758,50.3094409370048,-30.0931731157143));
#20355=CARTESIAN_POINT('Ctrl Pts',(-17.5359687349261,50.6166993996009,-30.0737629289367));
#20356=CARTESIAN_POINT('Ctrl Pts',(-17.6453243085392,50.9021311817274,-30.054352742159));
#20357=CARTESIAN_POINT('Ctrl Pts',(-17.9419477869372,51.6763557160829,-30.0017032344282));
#20358=CARTESIAN_POINT('Ctrl Pts',(-18.6577297847812,52.2899908444972,-29.9490537266973));
#20359=CARTESIAN_POINT('Ctrl Pts',(-19.468181418111,52.4648544129348,-29.8964042189665));
#20360=CARTESIAN_POINT('Ctrl Pts',(-20.2786330514408,52.6397179813725,-29.8437547112357));
#20361=CARTESIAN_POINT('Ctrl Pts',(-21.1837543202565,52.3758099898334,-29.7911052035049));
#20362=CARTESIAN_POINT('Ctrl Pts',(-21.7732222613504,51.7927691130892,-29.738455695774));
#20363=CARTESIAN_POINT('Ctrl Pts',(-22.3626902024443,51.2097282363449,-29.6858061880432));
#20364=CARTESIAN_POINT('Ctrl Pts',(-22.6365048158163,50.3075544743955,-29.6331566803124));
#20365=CARTESIAN_POINT('Ctrl Pts',(-22.470536410341,49.4952345830201,-29.5805071725816));
#20366=CARTESIAN_POINT('Ctrl Pts',(-22.3045680048657,48.6829146916447,-29.5278576648507));
#20367=CARTESIAN_POINT('Ctrl Pts',(-21.698816580543,47.9604486708432,-29.4752081571199));
#20368=CARTESIAN_POINT('Ctrl Pts',(-20.927890334043,47.6553555047671,-29.4225586493891));
#20369=CARTESIAN_POINT('Ctrl Pts',(-20.156964087543,47.3502623386911,-29.3699091416583));
#20370=CARTESIAN_POINT('Ctrl Pts',(-19.2208630188656,47.4625420273406,-29.3172596339275));
#20371=CARTESIAN_POINT('Ctrl Pts',(-18.5439543123787,47.9412942812296,-29.2646101261966));
#20372=CARTESIAN_POINT('Ctrl Pts',(-17.8924238105087,48.4020974785568,-29.2139345182951));
#20373=CARTESIAN_POINT('Ctrl Pts',(-17.4810150610682,49.2024092703463,-29.1632589103935));
#20374=CARTESIAN_POINT('Ctrl Pts',(-17.4785832788205,50.0005609135351,-29.112583302492));
#20375=CARTESIAN_POINT('Ctrl Pts',(-17.4814019803852,49.9978738298142,-29.387416697508));
#20376=CARTESIAN_POINT('Ctrl Pts',(-17.4799826025825,49.8397393658052,-29.3974274470402));
#20377=CARTESIAN_POINT('Ctrl Pts',(-17.4936138006039,49.6818487128234,-29.4074381965724));
#20378=CARTESIAN_POINT('Ctrl Pts',(-17.5231848896151,49.5270021041333,-29.4174489461046));
#20379=CARTESIAN_POINT('Ctrl Pts',(-17.6787080374567,48.7126177570775,-29.4700984538354));
#20380=CARTESIAN_POINT('Ctrl Pts',(-18.275131882735,47.9824323077474,-29.5227479615663));
#20381=CARTESIAN_POINT('Ctrl Pts',(-19.0420767449029,47.6674642258089,-29.5753974692971));
#20382=CARTESIAN_POINT('Ctrl Pts',(-19.8090216070708,47.3524961438704,-29.6280469770279));
#20383=CARTESIAN_POINT('Ctrl Pts',(-20.7464874861283,47.4527454293235,-29.6806964847587));
#20384=CARTESIAN_POINT('Ctrl Pts',(-21.4294884816705,47.9227655930774,-29.7333459924895));
#20385=CARTESIAN_POINT('Ctrl Pts',(-22.1124894772127,48.3927857568314,-29.7859955002204));
#20386=CARTESIAN_POINT('Ctrl Pts',(-22.5410255892397,49.2325767988862,-29.8386450079512));
#20387=CARTESIAN_POINT('Ctrl Pts',(-22.5208264880333,50.0614322208726,-29.891294515682));
#20388=CARTESIAN_POINT('Ctrl Pts',(-22.5006273868269,50.8902876428591,-29.9439440234128));
#20389=CARTESIAN_POINT('Ctrl Pts',(-22.0316930723873,51.7082074447772,-29.9965935311437));
#20390=CARTESIAN_POINT('Ctrl Pts',(-21.3266077851688,52.1444001223798,-30.0492430388745));
#20391=CARTESIAN_POINT('Ctrl Pts',(-20.6215224979503,52.5805927999825,-30.1018925466053));
#20392=CARTESIAN_POINT('Ctrl Pts',(-19.680286237953,52.6350583532697,-30.1545420543361));
#20393=CARTESIAN_POINT('Ctrl Pts',(-18.9295941504434,52.2831056519065,-30.207191562067));
#20394=CARTESIAN_POINT('Ctrl Pts',(-18.1789020629339,51.9311529505433,-30.2598410697978));
#20395=CARTESIAN_POINT('Ctrl Pts',(-17.6187541479122,51.1727819945297,-30.3124905775286));
#20396=CARTESIAN_POINT('Ctrl Pts',(-17.5030849445888,50.3517887243693,-30.3651400852594));
#20397=CARTESIAN_POINT('Ctrl Pts',(-17.4867712878388,50.2359981593902,-30.3725656226756));
#20398=CARTESIAN_POINT('Ctrl Pts',(-17.4792989715977,50.1189619437461,-30.3799911600918));
#20399=CARTESIAN_POINT('Ctrl Pts',(-17.4802498150093,50.0018038622189,-30.387416697508));
#20400=CARTESIAN_POINT('Origin',(-20.,50.,-32.));
#20401=CARTESIAN_POINT('',(-17.4864433733835,50.0003713189876,-31.387416697508));
#20402=CARTESIAN_POINT('',(-17.4840571036416,49.9979064241661,-31.112583302492));
#20403=CARTESIAN_POINT('',(-17.4825,50.,-32.));
#20404=CARTESIAN_POINT('Ctrl Pts',(-17.4840571036416,49.9979064241661,-31.112583302492));
#20405=CARTESIAN_POINT('Ctrl Pts',(-17.488725099653,50.5815220694055,-31.0757368287659));
#20406=CARTESIAN_POINT('Ctrl Pts',(-17.6911787677614,51.1680598147817,-31.0388903550398));
#20407=CARTESIAN_POINT('Ctrl Pts',(-18.0625521907884,51.6138879352617,-31.0020438813138));
#20408=CARTESIAN_POINT('Ctrl Pts',(-18.5932034561454,52.2509266720031,-30.949394373583));
#20409=CARTESIAN_POINT('Ctrl Pts',(-19.4687420272821,52.6006753670845,-30.8967448658522));
#20410=CARTESIAN_POINT('Ctrl Pts',(-20.2922558071245,52.5045807681535,-30.8440953581213));
#20411=CARTESIAN_POINT('Ctrl Pts',(-21.115769586967,52.4084861692224,-30.7914458503905));
#20412=CARTESIAN_POINT('Ctrl Pts',(-21.8872585755153,51.866548276279,-30.7387963426597));
#20413=CARTESIAN_POINT('Ctrl Pts',(-22.2569799716995,51.1244463919412,-30.6861468349288));
#20414=CARTESIAN_POINT('Ctrl Pts',(-22.6267013678837,50.3823445076034,-30.633497327198));
#20415=CARTESIAN_POINT('Ctrl Pts',(-22.5946551717038,49.4400786318712,-30.5808478194672));
#20416=CARTESIAN_POINT('Ctrl Pts',(-22.1753690388774,48.7248106706471,-30.5281983117364));
#20417=CARTESIAN_POINT('Ctrl Pts',(-21.7560829060511,48.0095427094229,-30.4755488040056));
#20418=CARTESIAN_POINT('Ctrl Pts',(-20.9495568365783,47.5212726627068,-30.4228992962747));
#20419=CARTESIAN_POINT('Ctrl Pts',(-20.1214171593638,47.4813503311467,-30.3702497885439));
#20420=CARTESIAN_POINT('Ctrl Pts',(-19.2932774821493,47.4414279995867,-30.3176002808131));
#20421=CARTESIAN_POINT('Ctrl Pts',(-18.4435241971931,47.8498533831827,-30.2649507730823));
#20422=CARTESIAN_POINT('Ctrl Pts',(-17.957380034191,48.521473045129,-30.2123012653514));
#20423=CARTESIAN_POINT('Ctrl Pts',(-17.6504616495758,48.9454880542725,-30.1790619443983));
#20424=CARTESIAN_POINT('Ctrl Pts',(-17.4884706399535,49.4744070759156,-30.1458226234451));
#20425=CARTESIAN_POINT('Ctrl Pts',(-17.4853852564016,50.0015907042489,-30.112583302492));
#20426=CARTESIAN_POINT('Ctrl Pts',(-17.4802498150093,50.0018038622189,-30.387416697508));
#20427=CARTESIAN_POINT('Ctrl Pts',(-17.4860407647828,49.2882725305271,-30.4326406678226));
#20428=CARTESIAN_POINT('Ctrl Pts',(-17.804264517897,48.5702209355301,-30.4778646381373));
#20429=CARTESIAN_POINT('Ctrl Pts',(-18.3404526792369,48.1015156596168,-30.5230886084519));
#20430=CARTESIAN_POINT('Ctrl Pts',(-18.9646801088331,47.5558514493319,-30.5757381161827));
#20431=CARTESIAN_POINT('Ctrl Pts',(-19.8843254596506,47.3481386130694,-30.6283876239135));
#20432=CARTESIAN_POINT('Ctrl Pts',(-20.6824814967706,47.5725406064986,-30.6810371316444));
#20433=CARTESIAN_POINT('Ctrl Pts',(-21.4806375338907,47.7969425999279,-30.7336866393752));
#20434=CARTESIAN_POINT('Ctrl Pts',(-22.1573042573133,48.4534594230489,-30.786336147106));
#20435=CARTESIAN_POINT('Ctrl Pts',(-22.4057250979189,49.244469157628,-30.8389856548368));
#20436=CARTESIAN_POINT('Ctrl Pts',(-22.6541459385245,50.0354788922071,-30.8916351625677));
#20437=CARTESIAN_POINT('Ctrl Pts',(-22.4743208963131,50.9609815382444,-30.9442846702985));
#20438=CARTESIAN_POINT('Ctrl Pts',(-21.9477709196056,51.6014145451042,-30.9969341780293));
#20439=CARTESIAN_POINT('Ctrl Pts',(-21.421220942898,52.2418475519639,-31.0495836857601));
#20440=CARTESIAN_POINT('Ctrl Pts',(-20.5479460316942,52.5972109196462,-31.1022331934909));
#20441=CARTESIAN_POINT('Ctrl Pts',(-19.7238320872605,52.5064060693562,-31.1548827012218));
#20442=CARTESIAN_POINT('Ctrl Pts',(-18.8997181428269,52.4156012190662,-31.2075322089526));
#20443=CARTESIAN_POINT('Ctrl Pts',(-18.1247651651633,51.8786281508041,-31.2601817166834));
#20444=CARTESIAN_POINT('Ctrl Pts',(-17.750286302129,51.1389154394177,-31.3128312244142));
#20445=CARTESIAN_POINT('Ctrl Pts',(-17.5734522134114,50.7896128855406,-31.3376930487788));
#20446=CARTESIAN_POINT('Ctrl Pts',(-17.4859181965247,50.3951022544555,-31.3625548731434));
#20447=CARTESIAN_POINT('Ctrl Pts',(-17.4864433733835,50.0003713189876,-31.387416697508));
#20448=CARTESIAN_POINT('Origin',(-20.,50.,-32.));
#20449=CARTESIAN_POINT('',(-17.4815610326054,49.9978466802305,-32.387416697508));
#20450=CARTESIAN_POINT('',(-17.478534759349,50.0004659858125,-32.112583302492));
#20451=CARTESIAN_POINT('',(-17.4825,50.,-32.));
#20452=CARTESIAN_POINT('Ctrl Pts',(-17.478534759349,50.0004659858125,-32.112583302492));
#20453=CARTESIAN_POINT('Ctrl Pts',(-17.4784686730675,50.0261887407035,-32.1109500495484));
#20454=CARTESIAN_POINT('Ctrl Pts',(-17.4788286095695,50.0519096014822,-32.1093167966047));
#20455=CARTESIAN_POINT('Ctrl Pts',(-17.4796202951709,50.0776171661923,-32.1076835436611));
#20456=CARTESIAN_POINT('Ctrl Pts',(-17.5051410556608,50.9063256845015,-32.0550340359303));
#20457=CARTESIAN_POINT('Ctrl Pts',(-17.979317496994,51.7212174820695,-32.0023845281994));
#20458=CARTESIAN_POINT('Ctrl Pts',(-18.6871889402044,52.1528737543759,-31.9497350204686));
#20459=CARTESIAN_POINT('Ctrl Pts',(-19.3950603834147,52.5845300266822,-31.8970855127378));
#20460=CARTESIAN_POINT('Ctrl Pts',(-20.3366268285023,52.6329507737268,-31.844436005007));
#20461=CARTESIAN_POINT('Ctrl Pts',(-21.085043445811,52.2761851861623,-31.7917864972761));
#20462=CARTESIAN_POINT('Ctrl Pts',(-21.8334600631198,51.9194195985978,-31.7391369895453));
#20463=CARTESIAN_POINT('Ctrl Pts',(-22.3887268526497,51.1574676764241,-31.6864874818145));
#20464=CARTESIAN_POINT('Ctrl Pts',(-22.4991220592055,50.3357487366985,-31.6338379740837));
#20465=CARTESIAN_POINT('Ctrl Pts',(-22.6095172657613,49.514029796973,-31.5811884663529));
#20466=CARTESIAN_POINT('Ctrl Pts',(-22.2750408893429,48.6325438396956,-31.528538958622));
#20467=CARTESIAN_POINT('Ctrl Pts',(-21.64732270888,48.0908991190064,-31.4758894508912));
#20468=CARTESIAN_POINT('Ctrl Pts',(-21.0196045284171,47.5492543983172,-31.4232399431604));
#20469=CARTESIAN_POINT('Ctrl Pts',(-20.0986445439097,47.3474509142161,-31.3705904354296));
#20470=CARTESIAN_POINT('Ctrl Pts',(-19.3019459594684,47.5769732074326,-31.3179409276987));
#20471=CARTESIAN_POINT('Ctrl Pts',(-18.5052473750271,47.8064955006491,-31.2652914199679));
#20472=CARTESIAN_POINT('Ctrl Pts',(-17.8328101906518,48.4673435711831,-31.2126419122371));
#20473=CARTESIAN_POINT('Ctrl Pts',(-17.5894735782529,49.2599319956509,-31.1599924045063));
#20474=CARTESIAN_POINT('Ctrl Pts',(-17.5164347802454,49.49783169051,-31.1441893705015));
#20475=CARTESIAN_POINT('Ctrl Pts',(-17.4820550531808,49.7476003038031,-31.1283863364967));
#20476=CARTESIAN_POINT('Ctrl Pts',(-17.4840571036416,49.9979064241661,-31.112583302492));
#20477=CARTESIAN_POINT('Ctrl Pts',(-17.4864433733835,50.0003713189876,-31.387416697508));
#20478=CARTESIAN_POINT('Ctrl Pts',(-17.4870303555796,49.5591865495684,-31.4152043808743));
#20479=CARTESIAN_POINT('Ctrl Pts',(-17.59762258459,49.1177265716563,-31.4429920642405));
#20480=CARTESIAN_POINT('Ctrl Pts',(-17.8164875049079,48.7388048191065,-31.4707797476067));
#20481=CARTESIAN_POINT('Ctrl Pts',(-18.2311723191263,48.0208592646925,-31.5234292553375));
#20482=CARTESIAN_POINT('Ctrl Pts',(-19.0345466959683,47.5274205103753,-31.5760787630684));
#20483=CARTESIAN_POINT('Ctrl Pts',(-19.8624130784562,47.4821815117939,-31.6287282707992));
#20484=CARTESIAN_POINT('Ctrl Pts',(-20.690279460944,47.4369425132125,-31.68137777853));
#20485=CARTESIAN_POINT('Ctrl Pts',(-21.5426378490777,47.839903270367,-31.7340272862608));
#20486=CARTESIAN_POINT('Ctrl Pts',(-22.0330845292512,48.50838765175,-31.7866767939916));
#20487=CARTESIAN_POINT('Ctrl Pts',(-22.5235312094246,49.176872033133,-31.8393263017225));
#20488=CARTESIAN_POINT('Ctrl Pts',(-22.6520661816377,50.1108800387446,-31.8919758094533));
#20489=CARTESIAN_POINT('Ctrl Pts',(-22.360420070845,50.8869933425255,-31.9446253171841));
#20490=CARTESIAN_POINT('Ctrl Pts',(-22.0687739600522,51.6631066463064,-31.9972748249149));
#20491=CARTESIAN_POINT('Ctrl Pts',(-21.3569467662536,52.2813252482565,-32.0499243326458));
#20492=CARTESIAN_POINT('Ctrl Pts',(-20.547634523135,52.4613891463162,-32.1025738403766));
#20493=CARTESIAN_POINT('Ctrl Pts',(-19.7383222800163,52.6414530443759,-32.1552233481074));
#20494=CARTESIAN_POINT('Ctrl Pts',(-18.8315249875777,52.3833622385452,-32.2078728558382));
#20495=CARTESIAN_POINT('Ctrl Pts',(-18.2383254088496,51.8041182709089,-32.2605223635691));
#20496=CARTESIAN_POINT('Ctrl Pts',(-17.7617545368076,51.3387592034373,-32.302820474882));
#20497=CARTESIAN_POINT('Ctrl Pts',(-17.4875909824012,50.6661162585989,-32.345118586195));
#20498=CARTESIAN_POINT('Ctrl Pts',(-17.4815610326054,49.9978466802305,-32.387416697508));
#20499=CARTESIAN_POINT('Origin',(-20.,50.,-32.));
#20500=CARTESIAN_POINT('',(-17.4801090128678,50.0017467021859,-33.387416697508));
#20501=CARTESIAN_POINT('',(-17.4852780367125,50.001651275735,-33.112583302492));
#20502=CARTESIAN_POINT('',(-17.4825,50.,-32.));
#20503=CARTESIAN_POINT('Ctrl Pts',(-17.4852780367125,50.001651275735,-33.112583302492));
#20504=CARTESIAN_POINT('Ctrl Pts',(-17.4834355077518,50.3040663382375,-33.0935137626));
#20505=CARTESIAN_POINT('Ctrl Pts',(-17.5339466800226,50.6058866653819,-33.0744442227079));
#20506=CARTESIAN_POINT('Ctrl Pts',(-17.639580266889,50.8869932156125,-33.0553746828159));
#20507=CARTESIAN_POINT('Ctrl Pts',(-17.9312263359524,51.6631064083454,-33.0027251750851));
#20508=CARTESIAN_POINT('Ctrl Pts',(-18.6430534279012,52.2813249218394,-32.9500756673542));
#20509=CARTESIAN_POINT('Ctrl Pts',(-19.4523655552217,52.4613887941352,-32.8974261596234));
#20510=CARTESIAN_POINT('Ctrl Pts',(-20.2616776825422,52.641452666431,-32.8447766518926));
#20511=CARTESIAN_POINT('Ctrl Pts',(-21.1684748452343,52.3833618975286,-32.7921271441618));
#20512=CARTESIAN_POINT('Ctrl Pts',(-21.7616743390861,51.8041180127718,-32.739477636431));
#20513=CARTESIAN_POINT('Ctrl Pts',(-22.3548738329379,51.224874128015,-32.6868281287001));
#20514=CARTESIAN_POINT('Ctrl Pts',(-22.6344756579494,50.3244771274039,-32.6341786209693));
#20515=CARTESIAN_POINT('Ctrl Pts',(-22.4737265786042,49.5111082989972,-32.5815291132385));
#20516=CARTESIAN_POINT('Ctrl Pts',(-22.312977499259,48.6977394705904,-32.5288796055076));
#20517=CARTESIAN_POINT('Ctrl Pts',(-21.711877515557,47.9713988143879,-32.4762300977768));
#20518=CARTESIAN_POINT('Ctrl Pts',(-20.9429261642948,47.6613618215529,-32.423580590046));
#20519=CARTESIAN_POINT('Ctrl Pts',(-20.1739748130326,47.3513248287178,-32.3709310823152));
#20520=CARTESIAN_POINT('Ctrl Pts',(-19.2371720942102,47.4575914992502,-32.3182815745843));
#20521=CARTESIAN_POINT('Ctrl Pts',(-18.5572032746223,47.9319874540416,-32.2656320668535));
#20522=CARTESIAN_POINT('Ctrl Pts',(-17.8983279300551,48.3916670587091,-32.2146158120663));
#20523=CARTESIAN_POINT('Ctrl Pts',(-17.4805990290548,49.1969905520396,-32.1635995572792));
#20524=CARTESIAN_POINT('Ctrl Pts',(-17.478534759349,50.0004659858125,-32.112583302492));
#20525=CARTESIAN_POINT('Ctrl Pts',(-17.4815610326054,49.9978466802305,-32.387416697508));
#20526=CARTESIAN_POINT('Ctrl Pts',(-17.4800853544066,49.8343045478529,-32.3977680939258));
#20527=CARTESIAN_POINT('Ctrl Pts',(-17.494668257568,49.6710243373683,-32.4081194903437));
#20528=CARTESIAN_POINT('Ctrl Pts',(-17.5262730674496,49.5111082290455,-32.4184708867615));
#20529=CARTESIAN_POINT('Ctrl Pts',(-17.6870221697952,48.6977392842601,-32.4711203944923));
#20530=CARTESIAN_POINT('Ctrl Pts',(-18.2881222395038,47.9713985241312,-32.5237699022232));
#20531=CARTESIAN_POINT('Ctrl Pts',(-19.0570737007893,47.6613614869354,-32.576419409954));
#20532=CARTESIAN_POINT('Ctrl Pts',(-19.8260251620747,47.3513244497396,-32.6290689176848));
#20533=CARTESIAN_POINT('Ctrl Pts',(-20.762828014937,47.4575911354768,-32.6817184254156));
#20534=CARTESIAN_POINT('Ctrl Pts',(-21.4427969318163,47.9319871581458,-32.7343679331465));
#20535=CARTESIAN_POINT('Ctrl Pts',(-22.1227658486956,48.4063831808148,-32.7870174408773));
#20536=CARTESIAN_POINT('Ctrl Pts',(-22.5459008295921,49.2489085404154,-32.8396669486081));
#20537=CARTESIAN_POINT('Ctrl Pts',(-22.5203800654506,50.077617177298,-32.8923164563389));
#20538=CARTESIAN_POINT('Ctrl Pts',(-22.4948593013091,50.9063258141806,-32.9449659640697));
#20539=CARTESIAN_POINT('Ctrl Pts',(-22.0206827921297,51.7212177283451,-32.9976154718006));
#20540=CARTESIAN_POINT('Ctrl Pts',(-21.3128112476355,52.1528740624138,-33.0502649795314));
#20541=CARTESIAN_POINT('Ctrl Pts',(-20.6049397031413,52.5845303964825,-33.1029144872622));
#20542=CARTESIAN_POINT('Ctrl Pts',(-19.6633731233323,52.6329511504552,-33.155563994993));
#20543=CARTESIAN_POINT('Ctrl Pts',(-18.9149563989385,52.2761855118439,-33.2082135027239));
#20544=CARTESIAN_POINT('Ctrl Pts',(-18.1665396745447,51.9194198732325,-33.2608630104547));
#20545=CARTESIAN_POINT('Ctrl Pts',(-17.6112728055659,51.157467842037,-33.3135125181855));
#20546=CARTESIAN_POINT('Ctrl Pts',(-17.5008775832146,50.3357487847381,-33.3661620259163));
#20547=CARTESIAN_POINT('Ctrl Pts',(-17.4860220204721,50.225172450433,-33.3732469164469));
#20548=CARTESIAN_POINT('Ctrl Pts',(-17.479222326559,50.1135138369441,-33.3803318069775));
#20549=CARTESIAN_POINT('Ctrl Pts',(-17.4801090128678,50.0017467021859,-33.387416697508));
#20550=CARTESIAN_POINT('Origin',(-20.,50.,-32.));
#20551=CARTESIAN_POINT('',(-17.4864166347396,50.0004567153817,-34.387416697508));
#20552=CARTESIAN_POINT('',(-17.4841986291653,49.9979396995438,-34.112583302492));
#20553=CARTESIAN_POINT('',(-17.4825,50.,-32.));
#20554=CARTESIAN_POINT('Ctrl Pts',(-17.4841986291653,49.9979396995438,-34.112583302492));
#20555=CARTESIAN_POINT('Ctrl Pts',(-17.4887310996937,50.5762421906731,-34.0760774756515));
#20556=CARTESIAN_POINT('Ctrl Pts',(-17.6871330770759,51.1573544545628,-34.0395716488111));
#20557=CARTESIAN_POINT('Ctrl Pts',(-18.0522293590857,51.6014143159703,-34.0030658219707));
#20558=CARTESIAN_POINT('Ctrl Pts',(-18.5787792604534,52.2418472311955,-33.9504163142398));
#20559=CARTESIAN_POINT('Ctrl Pts',(-19.4520540467071,52.5972105480315,-33.897766806509));
#20560=CARTESIAN_POINT('Ctrl Pts',(-20.2761678732247,52.5064057107341,-33.8451172987782));
#20561=CARTESIAN_POINT('Ctrl Pts',(-21.1002816997423,52.4156008734368,-33.7924677910474));
#20562=CARTESIAN_POINT('Ctrl Pts',(-21.8752345665239,51.878627882006,-33.7398182833166));
#20563=CARTESIAN_POINT('Ctrl Pts',(-22.249713375977,51.1389152764592,-33.6871687755858));
#20564=CARTESIAN_POINT('Ctrl Pts',(-22.6241921854301,50.3992026709125,-33.6345192678549));
#20565=CARTESIAN_POINT('Ctrl Pts',(-22.5981969375548,49.4567504512499,-33.5818697601241));
#20566=CARTESIAN_POINT('Ctrl Pts',(-22.1835121826704,48.7388049995611,-33.5292202523933));
#20567=CARTESIAN_POINT('Ctrl Pts',(-21.768827427786,48.0208595478723,-33.4765707446624));
#20568=CARTESIAN_POINT('Ctrl Pts',(-20.9654531658926,47.5274208641573,-33.4239212369316));
#20569=CARTESIAN_POINT('Ctrl Pts',(-20.1375869018576,47.4821818720488,-33.3712717292008));
#20570=CARTESIAN_POINT('Ctrl Pts',(-19.3097206378227,47.4369428799404,-33.31862222147));
#20571=CARTESIAN_POINT('Ctrl Pts',(-18.4573623716463,47.8399035794383,-33.2659727137392));
#20572=CARTESIAN_POINT('Ctrl Pts',(-17.966915761647,48.5083878651731,-33.2133232060083));
#20573=CARTESIAN_POINT('Ctrl Pts',(-17.6541078722624,48.934748562228,-33.1797432381695));
#20574=CARTESIAN_POINT('Ctrl Pts',(-17.4885225860615,49.4691220101996,-33.1461632703308));
#20575=CARTESIAN_POINT('Ctrl Pts',(-17.4852780367125,50.001651275735,-33.112583302492));
#20576=CARTESIAN_POINT('Ctrl Pts',(-17.4801090128678,50.0017467021859,-33.387416697508));
#20577=CARTESIAN_POINT('Ctrl Pts',(-17.4858115035506,49.2829456580686,-33.4329813147083));
#20578=CARTESIAN_POINT('Ctrl Pts',(-17.8094289999739,48.5596560850262,-33.4785459319085));
#20579=CARTESIAN_POINT('Ctrl Pts',(-18.3526770554175,48.090898845848,-33.5241105491088));
#20580=CARTESIAN_POINT('Ctrl Pts',(-18.9803953256957,47.5492540476591,-33.5767600568396));
#20581=CARTESIAN_POINT('Ctrl Pts',(-19.9013554419761,47.3474505346835,-33.6294095645704));
#20582=CARTESIAN_POINT('Ctrl Pts',(-20.6980541404108,47.5769728607406,-33.6820590723013));
#20583=CARTESIAN_POINT('Ctrl Pts',(-21.4947528388455,47.8064951867976,-33.7347085800321));
#20584=CARTESIAN_POINT('Ctrl Pts',(-22.1671901194345,48.4673433518873,-33.7873580877629));
#20585=CARTESIAN_POINT('Ctrl Pts',(-22.4105267666506,49.2599318897604,-33.8400075954937));
#20586=CARTESIAN_POINT('Ctrl Pts',(-22.6538634138666,50.0525204276335,-33.8926571032246));
#20587=CARTESIAN_POINT('Ctrl Pts',(-22.4680994277097,50.97684933829,-33.9453066109554));
#20588=CARTESIAN_POINT('Ctrl Pts',(-21.9374480864259,51.6138881661804,-33.9979561186862));
#20589=CARTESIAN_POINT('Ctrl Pts',(-21.4067967451421,52.2509269940707,-34.050605626417));
#20590=CARTESIAN_POINT('Ctrl Pts',(-20.5312580487314,52.6006757391949,-34.1032551341478));
#20591=CARTESIAN_POINT('Ctrl Pts',(-19.7077441510588,52.5045811265144,-34.1559046418787));
#20592=CARTESIAN_POINT('Ctrl Pts',(-18.8842302533861,52.4084865138339,-34.2085541496095));
#20593=CARTESIAN_POINT('Ctrl Pts',(-18.1127411544516,51.8665485433488,-34.2612036573403));
#20594=CARTESIAN_POINT('Ctrl Pts',(-17.7430197053668,51.1244465528294,-34.3138531650711));
#20595=CARTESIAN_POINT('Ctrl Pts',(-17.5708242630631,50.7788172126644,-34.3383743425501));
#20596=CARTESIAN_POINT('Ctrl Pts',(-17.4857791387596,50.3897688515684,-34.3628955200291));
#20597=CARTESIAN_POINT('Ctrl Pts',(-17.4864166347396,50.0004567153817,-34.387416697508));
#20598=CARTESIAN_POINT('Origin',(-20.,50.,-32.));
#20599=CARTESIAN_POINT('',(-17.481720920103,49.9978231917579,-35.387416697508));
#20600=CARTESIAN_POINT('',(-17.4784947018927,50.0003700141181,-35.112583302492));
#20601=CARTESIAN_POINT('',(-17.4825,50.,-32.));
#20602=CARTESIAN_POINT('Ctrl Pts',(-17.4784947018927,50.0003700141181,-35.112583302492));
#20603=CARTESIAN_POINT('Ctrl Pts',(-17.4784525295678,50.0207269157445,-35.111290696434));
#20604=CARTESIAN_POINT('Ctrl Pts',(-17.4786779615225,50.0410828596851,-35.109998090376));
#20605=CARTESIAN_POINT('Ctrl Pts',(-17.4791738726521,50.0614322120827,-35.108705484318));
#20606=CARTESIAN_POINT('Ctrl Pts',(-17.4993729709683,50.8902875154747,-35.0560559765872));
#20607=CARTESIAN_POINT('Ctrl Pts',(-17.9683072183117,51.708207200363,-35.0034064688563));
#20608=CARTESIAN_POINT('Ctrl Pts',(-18.6733924046451,52.1443998155543,-34.9507569611255));
#20609=CARTESIAN_POINT('Ctrl Pts',(-19.3784775909784,52.5805924307456,-34.8981074533947));
#20610=CARTESIAN_POINT('Ctrl Pts',(-20.3197137163016,52.6350579762398,-34.8454579456639));
#20611=CARTESIAN_POINT('Ctrl Pts',(-21.0704056964005,52.2831053252348,-34.792808437933));
#20612=CARTESIAN_POINT('Ctrl Pts',(-21.8210976764994,51.9311526742298,-34.7401589302022));
#20613=CARTESIAN_POINT('Ctrl Pts',(-22.381245511374,51.1727818267255,-34.6875094224714));
#20614=CARTESIAN_POINT('Ctrl Pts',(-22.4969146981471,50.3517886740346,-34.6348599147406));
#20615=CARTESIAN_POINT('Ctrl Pts',(-22.6125838849203,49.5307955213437,-34.5822104070097));
#20616=CARTESIAN_POINT('Ctrl Pts',(-22.283774423592,48.6471800634662,-34.5295608992789));
#20617=CARTESIAN_POINT('Ctrl Pts',(-21.6595470833116,48.1015159312561,-34.4769113915481));
#20618=CARTESIAN_POINT('Ctrl Pts',(-21.0353197430311,47.5558517990461,-34.4242618838173));
#20619=CARTESIAN_POINT('Ctrl Pts',(-20.1156745237985,47.3481389925035,-34.3716123760864));
#20620=CARTESIAN_POINT('Ctrl Pts',(-19.3175186008803,47.5725409538248,-34.3189628683556));
#20621=CARTESIAN_POINT('Ctrl Pts',(-18.5193626779622,47.7969429151461,-34.2663133606248));
#20622=CARTESIAN_POINT('Ctrl Pts',(-17.8426960513585,48.4534596443312,-34.213663852894));
#20623=CARTESIAN_POINT('Ctrl Pts',(-17.5942752462975,49.2444692657309,-34.1610143451631));
#20624=CARTESIAN_POINT('Ctrl Pts',(-17.5181030962378,49.4870129752447,-34.1448706642728));
#20625=CARTESIAN_POINT('Ctrl Pts',(-17.4821942708426,49.7422015973575,-34.1287269833824));
#20626=CARTESIAN_POINT('Ctrl Pts',(-17.4841986291653,49.9979396995438,-34.112583302492));
#20627=CARTESIAN_POINT('Ctrl Pts',(-17.4864166347396,50.0004567153817,-34.387416697508));
#20628=CARTESIAN_POINT('Ctrl Pts',(-17.4871479086549,49.5538753737183,-34.4155450277599));
#20629=CARTESIAN_POINT('Ctrl Pts',(-17.6006243673771,49.1069469444978,-34.4436733580117));
#20630=CARTESIAN_POINT('Ctrl Pts',(-17.824630649866,48.7248104881901,-34.4718016882636));
#20631=CARTESIAN_POINT('Ctrl Pts',(-18.2439168426848,48.0095424246239,-34.5244511959944));
#20632=CARTESIAN_POINT('Ctrl Pts',(-19.0504430275571,47.521272308045,-34.5771007037253));
#20633=CARTESIAN_POINT('Ctrl Pts',(-19.8785828232637,47.4813499707728,-34.6297502114561));
#20634=CARTESIAN_POINT('Ctrl Pts',(-20.7067226189702,47.4414276335006,-34.6823997191869));
#20635=CARTESIAN_POINT('Ctrl Pts',(-21.556476025511,47.8498530755351,-34.7350492269177));
#20636=CARTESIAN_POINT('Ctrl Pts',(-22.0426202580716,48.5214728335782,-34.7876987346486));
#20637=CARTESIAN_POINT('Ctrl Pts',(-22.5287644906322,49.1930925916214,-34.8403482423794));
#20638=CARTESIAN_POINT('Ctrl Pts',(-22.6512995492126,50.1279066656732,-34.8929977501102));
#20639=CARTESIAN_POINT('Ctrl Pts',(-22.354676028373,50.9021313108064,-34.945647257841));
#20640=CARTESIAN_POINT('Ctrl Pts',(-22.0580525075334,51.6763559559396,-34.9982967655718));
#20641=CARTESIAN_POINT('Ctrl Pts',(-21.3422704072737,52.2899911721542,-35.0509462733027));
#20642=CARTESIAN_POINT('Ctrl Pts',(-20.5318186579827,52.4648547656116,-35.1035957810335));
#20643=CARTESIAN_POINT('Ctrl Pts',(-19.7213669086916,52.6397183590691,-35.1562452887643));
#20644=CARTESIAN_POINT('Ctrl Pts',(-18.8162455103692,52.3758103297695,-35.2088947964951));
#20645=CARTESIAN_POINT('Ctrl Pts',(-18.226777484933,51.7927693696024,-35.2615443042259));
#20646=CARTESIAN_POINT('Ctrl Pts',(-17.7570184164389,51.3281321602486,-35.3035017686533));
#20647=CARTESIAN_POINT('Ctrl Pts',(-17.4877251401288,50.6608193538835,-35.3454592330807));
#20648=CARTESIAN_POINT('Ctrl Pts',(-17.481720920103,49.9978231917579,-35.387416697508));
#20649=CARTESIAN_POINT('Origin',(-20.,50.,-32.));
#20650=CARTESIAN_POINT('',(-17.4799716856498,50.0016863230979,-36.387416697508));
#20651=CARTESIAN_POINT('',(-17.4851666106336,50.0017093726515,-36.112583302492));
#20652=CARTESIAN_POINT('',(-17.4825,50.,-32.));
#20653=CARTESIAN_POINT('Ctrl Pts',(-17.4851666106336,50.0017093726515,-36.112583302492));
#20654=CARTESIAN_POINT('Ctrl Pts',(-17.483287936102,50.298689158319,-36.0938544094856));
#20655=CARTESIAN_POINT('Ctrl Pts',(-17.5319618132886,50.5950731831941,-36.0751255164792));
#20656=CARTESIAN_POINT('Ctrl Pts',(-17.6339335445166,50.8718186790697,-36.0563966234728));
#20657=CARTESIAN_POINT('Ctrl Pts',(-17.9205901797904,51.6497885312973,-36.003747115742));
#20658=CARTESIAN_POINT('Ctrl Pts',(-18.6284330174474,52.2725649409661,-35.9510976080111));
#20659=CARTESIAN_POINT('Ctrl Pts',(-19.4365722711018,52.4578216931553,-35.8984481002803));
#20660=CARTESIAN_POINT('Ctrl Pts',(-20.2447115247563,52.6430784453445,-35.8457985925495));
#20661=CARTESIAN_POINT('Ctrl Pts',(-21.1531471944084,52.3908155400541,-35.7931490848187));
#20662=CARTESIAN_POINT('Ctrl Pts',(-21.7500537836158,51.8153925293037,-35.7404995770878));
#20663=CARTESIAN_POINT('Ctrl Pts',(-22.3469603728231,51.2399695185533,-35.687850069357));
#20664=CARTESIAN_POINT('Ctrl Pts',(-22.6323378815858,50.3413864023429,-35.6352005616262));
#20665=CARTESIAN_POINT('Ctrl Pts',(-22.4768147559968,49.5270021718109,-35.5825510538954));
#20666=CARTESIAN_POINT('Ctrl Pts',(-22.3212916304078,48.712617941279,-35.5299015461646));
#20667=CARTESIAN_POINT('Ctrl Pts',(-21.7248678704671,47.9824325964254,-35.4772520384337));
#20668=CARTESIAN_POINT('Ctrl Pts',(-20.9579231180354,47.6674645595532,-35.4246025307029));
#20669=CARTESIAN_POINT('Ctrl Pts',(-20.1909783656036,47.3524965226811,-35.3719530229721));
#20670=CARTESIAN_POINT('Ctrl Pts',(-19.2535126206808,47.4527457937902,-35.3193035152412));
#20671=CARTESIAN_POINT('Ctrl Pts',(-18.5705117228638,47.9227658902926,-35.2666540075104));
#20672=CARTESIAN_POINT('Ctrl Pts',(-17.9042792837883,48.3812464520433,-35.2152971058376));
#20673=CARTESIAN_POINT('Ctrl Pts',(-17.480170262617,49.1915641225488,-35.1639402041648));
#20674=CARTESIAN_POINT('Ctrl Pts',(-17.4784947018927,50.0003700141181,-35.112583302492));
#20675=CARTESIAN_POINT('Ctrl Pts',(-17.481720920103,49.9978231917579,-35.387416697508));
#20676=CARTESIAN_POINT('Ctrl Pts',(-17.4801908614735,49.8288715219602,-35.3981087408115));
#20677=CARTESIAN_POINT('Ctrl Pts',(-17.4957584265948,49.6602001690132,-35.408800784115));
#20678=CARTESIAN_POINT('Ctrl Pts',(-17.5294632361692,49.4952345107971,-35.4194928274184));
#20679=CARTESIAN_POINT('Ctrl Pts',(-17.6954316653917,48.6829145031932,-35.4721423351493));
#20680=CARTESIAN_POINT('Ctrl Pts',(-18.3011831763866,47.9604483790198,-35.52479184288));
#20681=CARTESIAN_POINT('Ctrl Pts',(-19.0721095331925,47.6553551692903,-35.5774413506109));
#20682=CARTESIAN_POINT('Ctrl Pts',(-19.8430358899984,47.3502619595608,-35.6300908583417));
#20683=CARTESIAN_POINT('Ctrl Pts',(-20.7791370926151,47.4625416642753,-35.6827403660725));
#20684=CARTESIAN_POINT('Ctrl Pts',(-21.4560458959555,47.9412939866653,-35.7353898738034));
#20685=CARTESIAN_POINT('Ctrl Pts',(-22.1329546992959,48.4200463090554,-35.7880393815342));
#20686=CARTESIAN_POINT('Ctrl Pts',(-22.5506711033599,49.2652712491211,-35.840688889265));
#20687=CARTESIAN_POINT('Ctrl Pts',(-22.5198297284933,50.0937989335653,-35.8933383969958));
#20688=CARTESIAN_POINT('Ctrl Pts',(-22.4889883536267,50.9223266180095,-35.9459879047266));
#20689=CARTESIAN_POINT('Ctrl Pts',(-22.0095891998295,51.7341570468322,-35.9986374124575));
#20690=CARTESIAN_POINT('Ctrl Pts',(-21.2989605833562,52.1612592402719,-36.0512869201883));
#20691=CARTESIAN_POINT('Ctrl Pts',(-20.588331966883,52.5883614337116,-36.1039364279191));
#20692=CARTESIAN_POINT('Ctrl Pts',(-19.6464738877337,52.6307353917684,-36.1565859356499));
#20693=CARTESIAN_POINT('Ctrl Pts',(-18.9003633834041,52.2691715253439,-36.2092354433808));
#20694=CARTESIAN_POINT('Ctrl Pts',(-18.1542528790745,51.9076076589195,-36.2618849511116));
#20695=CARTESIAN_POINT('Ctrl Pts',(-17.6038899495646,51.1421059680139,-36.3145344588424));
#20696=CARTESIAN_POINT('Ctrl Pts',(-17.4987732597562,50.3196950025341,-36.3671839665732));
#20697=CARTESIAN_POINT('Ctrl Pts',(-17.4853081278343,50.2143466305072,-36.3739282102182));
#20698=CARTESIAN_POINT('Ctrl Pts',(-17.4791489700962,50.1080644433152,-36.3806724538631));
#20699=CARTESIAN_POINT('Ctrl Pts',(-17.4799716856498,50.0016863230979,-36.387416697508));
#20700=CARTESIAN_POINT('Origin',(-20.,50.,-32.));
#20701=CARTESIAN_POINT('',(-17.4863843841259,50.0005414264851,-37.387416697508));
#20702=CARTESIAN_POINT('',(-17.4843372649484,49.997976158615,-37.112583302492));
#20703=CARTESIAN_POINT('',(-17.4825,50.,-32.));
#20704=CARTESIAN_POINT('Ctrl Pts',(-17.4843372649484,49.997976158615,-37.112583302492));
#20705=CARTESIAN_POINT('Ctrl Pts',(-17.4887303937409,50.5709622382976,-37.0764181225372));
#20706=CARTESIAN_POINT('Ctrl Pts',(-17.6831295324326,51.1466451272143,-37.0402529425824));
#20707=CARTESIAN_POINT('Ctrl Pts',(-18.0419868338466,51.5888746702098,-37.0040877626276));
#20708=CARTESIAN_POINT('Ctrl Pts',(-18.5644136623227,52.2326753583812,-36.9514382548968));
#20709=CARTESIAN_POINT('Ctrl Pts',(-19.4353886577459,52.5936386469132,-36.8987887471659));
#20710=CARTESIAN_POINT('Ctrl Pts',(-20.2600685527347,52.5081273154602,-36.8461392394351));
#20711=CARTESIAN_POINT('Ctrl Pts',(-21.0847484477236,52.4226159840072,-36.7934897317043));
#20712=CARTESIAN_POINT('Ctrl Pts',(-21.8631332422781,51.8906300325692,-36.7408402239735));
#20713=CARTESIAN_POINT('Ctrl Pts',(-22.2423540255139,51.1533372037214,-36.6881907162427));
#20714=CARTESIAN_POINT('Ctrl Pts',(-22.6215748087496,50.4160443748736,-36.6355412085118));
#20715=CARTESIAN_POINT('Ctrl Pts',(-22.6016315806666,49.473444668616,-36.582891700781));
#20716=CARTESIAN_POINT('Ctrl Pts',(-22.1915653009581,48.7528513271896,-36.5302421930502));
#20717=CARTESIAN_POINT('Ctrl Pts',(-21.7814990212495,48.0322579857633,-36.4775926853194));
#20718=CARTESIAN_POINT('Ctrl Pts',(-20.9813096899156,47.5336710091681,-36.4249431775885));
#20719=CARTESIAN_POINT('Ctrl Pts',(-20.1537509717286,47.4831172216533,-36.3722936698577));
#20720=CARTESIAN_POINT('Ctrl Pts',(-19.3261922535416,47.4325634341385,-36.3196441621269));
#20721=CARTESIAN_POINT('Ctrl Pts',(-18.4712641485017,47.830042835704,-36.2669946543961));
#20722=CARTESIAN_POINT('Ctrl Pts',(-17.976535312427,48.4953641838799,-36.2143451466653));
#20723=CARTESIAN_POINT('Ctrl Pts',(-17.6577952716397,48.9240122395235,-36.1804245319408));
#20724=CARTESIAN_POINT('Ctrl Pts',(-17.4885691499591,49.4638379198578,-36.1465039172164));
#20725=CARTESIAN_POINT('Ctrl Pts',(-17.4851666106336,50.0017093726515,-36.112583302492));
#20726=CARTESIAN_POINT('Ctrl Pts',(-17.4799716856498,50.0016863230979,-36.387416697508));
#20727=CARTESIAN_POINT('Ctrl Pts',(-17.4855715685639,49.277614661599,-36.4333219615939));
#20728=CARTESIAN_POINT('Ctrl Pts',(-17.8146387939379,48.5490984621573,-36.4792272256798));
#20729=CARTESIAN_POINT('Ctrl Pts',(-18.3649693501693,48.0803607431838,-36.5251324897657));
#20730=CARTESIAN_POINT('Ctrl Pts',(-18.9961525804978,47.5427576893674,-36.5777819974965));
#20731=CARTESIAN_POINT('Ctrl Pts',(-19.9183894912617,47.3468718217887,-36.6304315052273));
#20732=CARTESIAN_POINT('Ctrl Pts',(-20.7135980034659,47.5815050164462,-36.6830810129582));
#20733=CARTESIAN_POINT('Ctrl Pts',(-21.5088065156701,47.8161382111036,-36.735730520689));
#20734=CARTESIAN_POINT('Ctrl Pts',(-22.1769866293146,48.4812904679973,-36.7883800284198));
#20735=CARTESIAN_POINT('Ctrl Pts',(-22.4152290503386,49.2754251328188,-36.8410295361506));
#20736=CARTESIAN_POINT('Ctrl Pts',(-22.6534714713626,50.0695597976402,-36.8936790438815));
#20737=CARTESIAN_POINT('Ctrl Pts',(-22.4617761997662,50.9926768703893,-36.9463285516123));
#20738=CARTESIAN_POINT('Ctrl Pts',(-21.9270453727093,51.6262952508436,-36.9989780593431));
#20739=CARTESIAN_POINT('Ctrl Pts',(-21.3923145456525,52.2599136312978,-37.0516275670739));
#20740=CARTESIAN_POINT('Ctrl Pts',(-20.5145481631352,52.6040333194572,-37.1042770748047));
#20741=CARTESIAN_POINT('Ctrl Pts',(-19.6916682649385,52.502652913465,-37.1569265825356));
#20742=CARTESIAN_POINT('Ctrl Pts',(-18.8687883667419,52.4012725074729,-37.2095760902664));
#20743=CARTESIAN_POINT('Ctrl Pts',(-18.100794952866,51.8543920073292,-37.2622255979972));
#20744=CARTESIAN_POINT('Ctrl Pts',(-17.735846162153,51.1099313200771,-37.314875105728));
#20745=CARTESIAN_POINT('Ctrl Pts',(-17.5682348058617,50.768020157001,-37.3390556363214));
#20746=CARTESIAN_POINT('Ctrl Pts',(-17.4856385661448,50.3844329568945,-37.3632361669147));
#20747=CARTESIAN_POINT('Ctrl Pts',(-17.4863843841259,50.0005414264851,-37.387416697508));
#20748=CARTESIAN_POINT('Origin',(-20.,50.,-32.));
#20749=CARTESIAN_POINT('',(-17.4818815371047,49.9978011132584,-38.387416697508));
#20750=CARTESIAN_POINT('',(-17.4784633668112,50.000273285299,-38.112583302492));
#20751=CARTESIAN_POINT('',(-17.4825,50.,-32.));
#20752=CARTESIAN_POINT('Ctrl Pts',(-17.4784633668112,50.000273285299,-38.112583302492));
#20753=CARTESIAN_POINT('Ctrl Pts',(-17.4784400677728,50.0152649329971,-38.1116313433196));
#20754=CARTESIAN_POINT('Ctrl Pts',(-17.4785623286431,50.0302561905308,-38.1106793841472));
#20755=CARTESIAN_POINT('Ctrl Pts',(-17.4788313122131,50.0452448149025,-38.1097274249749));
#20756=CARTESIAN_POINT('Ctrl Pts',(-17.4937078457445,50.87421281861,-38.0570779172441));
#20757=CARTESIAN_POINT('Ctrl Pts',(-17.9573807060435,51.6951264893194,-38.0044284095132));
#20758=CARTESIAN_POINT('Ctrl Pts',(-18.6596506001565,52.1358374187989,-37.9517789017824));
#20759=CARTESIAN_POINT('Ctrl Pts',(-19.3619204942694,52.5765483482785,-37.8991293940516));
#20760=CARTESIAN_POINT('Ctrl Pts',(-20.3027874221963,52.6370565365281,-37.8464798863208));
#20761=CARTESIAN_POINT('Ctrl Pts',(-21.0557237967043,52.2899313553352,-37.7938303785899));
#20762=CARTESIAN_POINT('Ctrl Pts',(-21.8086601712123,51.9428061741423,-37.7411808708591));
#20763=CARTESIAN_POINT('Ctrl Pts',(-22.3736659923015,51.1880476235069,-37.6885313631283));
#20764=CARTESIAN_POINT('Ctrl Pts',(-22.4946043991423,50.3678140958698,-37.6358818553975));
#20765=CARTESIAN_POINT('Ctrl Pts',(-22.6155428059831,49.5475805682327,-37.5832323476666));
#20766=CARTESIAN_POINT('Ctrl Pts',(-22.2924137985756,48.661872063594,-37.5305828399358));
#20767=CARTESIAN_POINT('Ctrl Pts',(-21.6717030307037,48.1122110230468,-37.477933332205));
#20768=CARTESIAN_POINT('Ctrl Pts',(-21.0509922628319,47.5625499824997,-37.4252838244742));
#20769=CARTESIAN_POINT('Ctrl Pts',(-20.1326997344957,47.3489364060442,-37.3726343167433));
#20770=CARTESIAN_POINT('Ctrl Pts',(-19.3331193830197,47.5682087806212,-37.3199848090125));
#20771=CARTESIAN_POINT('Ctrl Pts',(-18.5335390315437,47.7874811551982,-37.2673353012817));
#20772=CARTESIAN_POINT('Ctrl Pts',(-17.8526708569279,48.4396394808077,-37.2146857935509));
#20773=CARTESIAN_POINT('Ctrl Pts',(-17.5991761003846,49.2290376875177,-37.1620362858201));
#20774=CARTESIAN_POINT('Ctrl Pts',(-17.519808014405,49.476194771146,-37.1455519580441));
#20775=CARTESIAN_POINT('Ctrl Pts',(-17.4823348478425,49.7368053207982,-37.129067630268));
#20776=CARTESIAN_POINT('Ctrl Pts',(-17.4843372649484,49.997976158615,-37.112583302492));
#20777=CARTESIAN_POINT('Ctrl Pts',(-17.4863843841259,50.0005414264851,-37.387416697508));
#20778=CARTESIAN_POINT('Ctrl Pts',(-17.4872624738341,49.5485662657117,-37.4158856746455));
#20779=CARTESIAN_POINT('Ctrl Pts',(-17.6036656476806,49.0961692556964,-37.444354651783));
#20780=CARTESIAN_POINT('Ctrl Pts',(-17.8328634864205,48.7108687042736,-37.4728236289205));
#20781=CARTESIAN_POINT('Ctrl Pts',(-18.256733768951,47.9983076500828,-37.5254731366513));
#20782=CARTESIAN_POINT('Ctrl Pts',(-19.0663785015622,47.5152264160619,-37.5781226443822));
#20783=CARTESIAN_POINT('Ctrl Pts',(-19.894757570296,47.4806223297718,-37.630772152113));
#20784=CARTESIAN_POINT('Ctrl Pts',(-20.7231366390297,47.4460182434818,-37.6834216598438));
#20785=CARTESIAN_POINT('Ctrl Pts',(-21.5702500438859,47.8598913049226,-37.7360711675746));
#20786=CARTESIAN_POINT('Ctrl Pts',(-22.0520717778747,48.5346188611104,-37.7887206753054));
#20787=CARTESIAN_POINT('Ctrl Pts',(-22.5338935118636,49.2093464172982,-37.8413701830363));
#20788=CARTESIAN_POINT('Ctrl Pts',(-22.6504235749849,50.144928468233,-37.8940196907671));
#20789=CARTESIAN_POINT('Ctrl Pts',(-22.3488348885255,50.9172323104341,-37.9466691984979));
#20790=CARTESIAN_POINT('Ctrl Pts',(-22.0472462020662,51.6895361526352,-37.9993187062287));
#20791=CARTESIAN_POINT('Ctrl Pts',(-21.327538766026,52.2985617861026,-38.0519682139595));
#20792=CARTESIAN_POINT('Ctrl Pts',(-20.5159808958408,52.468218309994,-38.1046177216904));
#20793=CARTESIAN_POINT('Ctrl Pts',(-19.7044230256556,52.6378748338855,-38.1572672294212));
#20794=CARTESIAN_POINT('Ctrl Pts',(-18.8010147213253,52.3681622482009,-38.209916737152));
#20795=CARTESIAN_POINT('Ctrl Pts',(-18.2153026112017,51.781347448765,-38.2625662448829));
#20796=CARTESIAN_POINT('Ctrl Pts',(-17.7523263162739,51.3174995327738,-38.3041830624246));
#20797=CARTESIAN_POINT('Ctrl Pts',(-17.4878502975171,50.6555224665065,-38.3457998799663));
#20798=CARTESIAN_POINT('Ctrl Pts',(-17.4818815371047,49.9978011132584,-38.387416697508));
#20799=CARTESIAN_POINT('Origin',(-20.,50.,-32.));
#20800=CARTESIAN_POINT('',(-17.4798420534852,50.0015648820515,-39.387416697508));
#20801=CARTESIAN_POINT('',(-17.4850543912228,50.0017607343381,-39.112583302492));
#20802=CARTESIAN_POINT('',(-17.4825,50.,-32.));
#20803=CARTESIAN_POINT('',(-21.913465996665,51.635987203375,-40.));
#20804=CARTESIAN_POINT('Ctrl Pts',(-17.4798420534852,50.0015648820515,-39.387416697508));
#20805=CARTESIAN_POINT('Ctrl Pts',(-17.4853146187272,49.2723761097304,-39.4336626084795));
#20806=CARTESIAN_POINT('Ctrl Pts',(-17.8198668900926,48.5389623205324,-39.4799085194511));
#20807=CARTESIAN_POINT('Ctrl Pts',(-18.3773137076179,48.0701212737088,-39.5261544304226));
#20808=CARTESIAN_POINT('Ctrl Pts',(-19.0119492875483,47.5363605627465,-39.5788039381534));
#20809=CARTESIAN_POINT('Ctrl Pts',(-19.9354807781592,47.345515300665,-39.6314534458843));
#20810=CARTESIAN_POINT('Ctrl Pts',(-20.7291493676954,47.5857188348087,-39.6841029536151));
#20811=CARTESIAN_POINT('Ctrl Pts',(-21.5228179572316,47.8259223689524,-39.7367524613459));
#20812=CARTESIAN_POINT('Ctrl Pts',(-22.186623645693,48.4971746993212,-39.7894019690767));
#20813=CARTESIAN_POINT('Ctrl Pts',(-22.4195845021318,49.2914441063715,-39.8420514768075));
#20814=CARTESIAN_POINT('Ctrl Pts',(-22.6525453585705,50.0857135134218,-39.8947009845384));
#20815=CARTESIAN_POINT('Ctrl Pts',(-22.4546613829867,51.0029999971535,-39.9473504922692));
#20816=CARTESIAN_POINT('Ctrl Pts',(-21.913465996665,51.635987203375,-40.));
#20817=CARTESIAN_POINT('',(-18.0829274149968,51.6385410457703,-40.));
#20818=CARTESIAN_POINT('Origin',(-20.,50.,-40.));
#20819=CARTESIAN_POINT('Ctrl Pts',(-18.0829199122823,51.6385463584782,-40.));
#20820=CARTESIAN_POINT('Ctrl Pts',(-18.6057517999179,52.2473170096207,-39.9490537266974));
#20821=CARTESIAN_POINT('Ctrl Pts',(-19.4454474456028,52.5873618729563,-39.8981074533947));
#20822=CARTESIAN_POINT('Ctrl Pts',(-20.2440955105381,52.5095729322154,-39.847161180092));
#20823=CARTESIAN_POINT('Ctrl Pts',(-21.0694439559331,52.429183353716,-39.7945116723612));
#20824=CARTESIAN_POINT('Ctrl Pts',(-21.8509543386143,51.9025549428044,-39.7418621646304));
#20825=CARTESIAN_POINT('Ctrl Pts',(-22.23483319536,51.1677991240005,-39.6892126568996));
#20826=CARTESIAN_POINT('Ctrl Pts',(-22.6187120521057,50.4330433051966,-39.6365631491688));
#20827=CARTESIAN_POINT('Ctrl Pts',(-22.6049593829159,49.4901600785004,-39.5839136414379));
#20828=CARTESIAN_POINT('Ctrl Pts',(-22.1995627546363,48.7669050303447,-39.5312641337071));
#20829=CARTESIAN_POINT('Ctrl Pts',(-21.7941661263566,48.0436499821891,-39.4786146259763));
#20830=CARTESIAN_POINT('Ctrl Pts',(-20.9971255389871,47.5400231125739,-39.4259651182454));
#20831=CARTESIAN_POINT('Ctrl Pts',(-20.1698912732234,47.4841784721833,-39.3733156105146));
#20832=CARTESIAN_POINT('Ctrl Pts',(-19.3426570074598,47.4283338317928,-39.3206661027838));
#20833=CARTESIAN_POINT('Ctrl Pts',(-18.4852290633019,47.8202714206268,-39.268016595053));
#20834=CARTESIAN_POINT('Ctrl Pts',(-17.9862470456528,48.4823914203806,-39.2153670873221));
#20835=CARTESIAN_POINT('Ctrl Pts',(-17.6615383411993,48.9132609100784,-39.1811058257121));
#20836=CARTESIAN_POINT('Ctrl Pts',(-17.4886191336564,49.4585433396218,-39.146844564102));
#20837=CARTESIAN_POINT('Ctrl Pts',(-17.4850543912228,50.0017607343381,-39.112583302492));
#20838=CARTESIAN_POINT('Origin',(-20.,50.,-42.2084234471774));
#20839=CARTESIAN_POINT('',(-16.9217886712226,50.0008183699211,-25.7915765528226));
#20840=CARTESIAN_POINT('',(-16.9314303843609,50.000333147012,-25.7084234471775));
#20841=CARTESIAN_POINT('',(-16.9265,50.0000000000002,-42.2084234471774));
#20842=CARTESIAN_POINT('',(-20.7937992825328,47.0307770462543,-25.));
#20843=CARTESIAN_POINT('Ctrl Pts',(-16.9314303843609,50.000333147012,-25.7084234471775));
#20844=CARTESIAN_POINT('Ctrl Pts',(-16.9311123866597,50.4955100463338,-25.6828803290416));
#20845=CARTESIAN_POINT('Ctrl Pts',(-17.2773641840547,52.0108184567304,-25.6046877031749));
#20846=CARTESIAN_POINT('Ctrl Pts',(-19.6484750337391,53.6086169320315,-25.4738455695774));
#20847=CARTESIAN_POINT('Ctrl Pts',(-22.8319255534364,52.2686663415281,-25.315897046385));
#20848=CARTESIAN_POINT('Ctrl Pts',(-23.4429082212044,48.865459646895,-25.1579485231924));
#20849=CARTESIAN_POINT('Ctrl Pts',(-21.7760378723045,47.2933710986319,-25.0526495077308));
#20850=CARTESIAN_POINT('Ctrl Pts',(-20.7937992825328,47.0307770462543,-25.));
#20851=CARTESIAN_POINT('',(-19.2062007174672,47.0307770462543,-25.));
#20852=CARTESIAN_POINT('Origin',(-20.,50.,-25.));
#20853=CARTESIAN_POINT('Ctrl Pts',(-16.9217886712226,50.0008183699211,-25.7915765528226));
#20854=CARTESIAN_POINT('Ctrl Pts',(-16.9216326522162,50.0453262421124,-25.7892620061077));
#20855=CARTESIAN_POINT('Ctrl Pts',(-16.9425932420072,51.1021122351085,-25.7342979516619));
#20856=CARTESIAN_POINT('Ctrl Pts',(-18.1518494766411,53.1200731989091,-25.6266843894854));
#20857=CARTESIAN_POINT('Ctrl Pts',(-21.6024146227446,53.2535259255151,-25.4687358662929));
#20858=CARTESIAN_POINT('Ctrl Pts',(-23.6000558056709,50.4361300140704,-25.3107873431005));
#20859=CARTESIAN_POINT('Ctrl Pts',(-22.3474165158894,47.2598763198176,-25.1545420543361));
#20860=CARTESIAN_POINT('Ctrl Pts',(-20.1513504643245,46.7747742461176,-25.0509462733027));
#20861=CARTESIAN_POINT('Ctrl Pts',(-19.2043343151472,47.0257029622097,-25.));
#20862=CARTESIAN_POINT('Origin',(-20.,50.,-42.2084234471774));
#20863=CARTESIAN_POINT('',(-16.9301481064099,50.0018654683783,-26.7915765528225));
#20864=CARTESIAN_POINT('',(-16.9249664934092,49.9974416687219,-26.7084234471774));
#20865=CARTESIAN_POINT('',(-16.9265,50.0000000000002,-42.2084234471774));
#20866=CARTESIAN_POINT('Ctrl Pts',(-16.9249664934092,49.9974416687219,-26.7084234471774));
#20867=CARTESIAN_POINT('Ctrl Pts',(-16.932354404873,50.8261741257165,-26.6654440420932));
#20868=CARTESIAN_POINT('Ctrl Pts',(-17.7039892803895,52.6822303383337,-26.5698151292781));
#20869=CARTESIAN_POINT('Ctrl Pts',(-20.8329798605529,53.5295001824726,-26.4215367087322));
#20870=CARTESIAN_POINT('Ctrl Pts',(-23.4108311578128,51.2319837018569,-26.2635881855397));
#20871=CARTESIAN_POINT('Ctrl Pts',(-22.8961090069582,47.8173680419797,-26.1056396623473));
#20872=CARTESIAN_POINT('Ctrl Pts',(-19.7557253769871,46.3818716002278,-25.9476911391548));
#20873=CARTESIAN_POINT('Ctrl Pts',(-17.3086034215628,47.9281379315223,-25.8152857340982));
#20874=CARTESIAN_POINT('Ctrl Pts',(-16.9317678439275,49.4748507889046,-25.7355298367724));
#20875=CARTESIAN_POINT('Ctrl Pts',(-16.9314303843609,50.000333147012,-25.7084234471775));
#20876=CARTESIAN_POINT('Ctrl Pts',(-16.9301481064099,50.0018654683783,-26.7915765528225));
#20877=CARTESIAN_POINT('Ctrl Pts',(-16.9280040139011,50.3843410166761,-26.7718257191592));
#20878=CARTESIAN_POINT('Ctrl Pts',(-17.1709937020916,51.7837498364551,-26.6994253777651));
#20879=CARTESIAN_POINT('Ctrl Pts',(-19.2579267840424,53.5497392783032,-26.5743755286402));
#20880=CARTESIAN_POINT('Ctrl Pts',(-22.5667152906276,52.5619003598412,-26.4164270054477));
#20881=CARTESIAN_POINT('Ctrl Pts',(-23.5483400872305,49.251248624616,-26.2584784822553));
#20882=CARTESIAN_POINT('Ctrl Pts',(-21.3127948732631,46.619498196827,-26.1005299590628));
#20883=CARTESIAN_POINT('Ctrl Pts',(-17.9371757378006,47.0463360002771,-25.9448959825852));
#20884=CARTESIAN_POINT('Ctrl Pts',(-16.9251816511758,49.0328957969052,-25.8419115138385));
#20885=CARTESIAN_POINT('Ctrl Pts',(-16.9217886712226,50.0008183699211,-25.7915765528226));
#20886=CARTESIAN_POINT('Origin',(-20.,50.,-42.2084234471774));
#20887=CARTESIAN_POINT('',(-16.9282249073135,49.997407390353,-27.7915765528225));
#20888=CARTESIAN_POINT('',(-16.9239286259646,50.0022679987088,-27.7084234471775));
#20889=CARTESIAN_POINT('',(-16.9265,50.0000000000002,-42.2084234471774));
#20890=CARTESIAN_POINT('Ctrl Pts',(-16.9239286259646,50.0022679987088,-27.7084234471775));
#20891=CARTESIAN_POINT('Ctrl Pts',(-16.9226895286024,50.1518848536015,-27.7006572628756));
#20892=CARTESIAN_POINT('Ctrl Pts',(-17.0003509237025,51.314512346611,-27.640241570843));
#20893=CARTESIAN_POINT('Ctrl Pts',(-18.4816793672832,53.2933332139959,-27.5271763710795));
#20894=CARTESIAN_POINT('Ctrl Pts',(-21.9276633802435,53.0717181892534,-27.369227847887));
#20895=CARTESIAN_POINT('Ctrl Pts',(-23.6258942504405,50.0650704860399,-27.2112793246945));
#20896=CARTESIAN_POINT('Ctrl Pts',(-22.0366358520053,46.9994237957239,-27.0533308015021));
#20897=CARTESIAN_POINT('Ctrl Pts',(-18.6008241139817,46.6543113906855,-26.8953822783096));
#20898=CARTESIAN_POINT('Ctrl Pts',(-17.0233221444774,48.6111088305139,-26.7804131602014));
#20899=CARTESIAN_POINT('Ctrl Pts',(-16.9233042586235,49.8109819466767,-26.718093549824));
#20900=CARTESIAN_POINT('Ctrl Pts',(-16.9249664934092,49.9974416687219,-26.7084234471774));
#20901=CARTESIAN_POINT('Ctrl Pts',(-16.9282249073135,49.997407390353,-27.7915765528225));
#20902=CARTESIAN_POINT('Ctrl Pts',(-16.9340842388497,50.7163995761236,-27.7543894322109));
#20903=CARTESIAN_POINT('Ctrl Pts',(-17.5432833311101,52.462287433857,-27.6645528038683));
#20904=CARTESIAN_POINT('Ctrl Pts',(-20.4434363605156,53.599263941172,-27.522066667795));
#20905=CARTESIAN_POINT('Ctrl Pts',(-23.2562595022286,51.5962804541496,-27.3641181446025));
#20906=CARTESIAN_POINT('Ctrl Pts',(-23.1167311715492,48.1459977760775,-27.2061696214101));
#20907=CARTESIAN_POINT('Ctrl Pts',(-20.151357511322,46.3766830290446,-27.0482210982176));
#20908=CARTESIAN_POINT('Ctrl Pts',(-17.4367209277074,47.7029693850521,-26.9100234086884));
#20909=CARTESIAN_POINT('Ctrl Pts',(-16.9337194898675,49.3647815550225,-26.8244752268901));
#20910=CARTESIAN_POINT('Ctrl Pts',(-16.9301481064099,50.0018654683783,-26.7915765528225));
#20911=CARTESIAN_POINT('Origin',(-20.,50.,-42.2084234471774));
#20912=CARTESIAN_POINT('',(-16.9217182551955,50.0006847935455,-28.7915765528225));
#20913=CARTESIAN_POINT('',(-16.9313401597895,50.0003484095168,-28.7084234471775));
#20914=CARTESIAN_POINT('',(-16.9265,50.0000000000002,-42.2084234471774));
#20915=CARTESIAN_POINT('Ctrl Pts',(-16.9313401597895,50.0003484095168,-28.7084234471775));
#20916=CARTESIAN_POINT('Ctrl Pts',(-16.9308408739778,50.4888704797936,-28.6832209759272));
#20917=CARTESIAN_POINT('Ctrl Pts',(-17.2704953682473,51.9972892968429,-28.6053689969462));
#20918=CARTESIAN_POINT('Ctrl Pts',(-19.6259746483565,53.6071381719488,-28.4748675102343));
#20919=CARTESIAN_POINT('Ctrl Pts',(-22.8159750830834,52.2850875351969,-28.3169189870418));
#20920=CARTESIAN_POINT('Ctrl Pts',(-23.4528165638848,48.8912175406165,-28.1589704638494));
#20921=CARTESIAN_POINT('Ctrl Pts',(-20.9590942591762,46.5026468548974,-28.0010219406569));
#20922=CARTESIAN_POINT('Ctrl Pts',(-17.7611609705603,47.2465513795375,-27.8508396017663));
#20923=CARTESIAN_POINT('Ctrl Pts',(-16.9310897755726,49.1375831769752,-27.7533067706065));
#20924=CARTESIAN_POINT('Ctrl Pts',(-16.9239286259646,50.0022679987088,-27.7084234471775));
#20925=CARTESIAN_POINT('Ctrl Pts',(-16.9217182551955,50.0006847935455,-28.7915765528225));
#20926=CARTESIAN_POINT('Ctrl Pts',(-16.9216026134698,50.0386403438613,-28.7896026529933));
#20927=CARTESIAN_POINT('Ctrl Pts',(-16.9393662086373,51.0888673611757,-28.7349792454332));
#20928=CARTESIAN_POINT('Ctrl Pts',(-18.1318615954084,53.1082786044884,-28.6277063301423));
#20929=CARTESIAN_POINT('Ctrl Pts',(-21.5814747736461,53.2634758336214,-28.4697578069498));
#20930=CARTESIAN_POINT('Ctrl Pts',(-23.5972128731322,50.4597787805748,-28.3118092837574));
#20931=CARTESIAN_POINT('Ctrl Pts',(-22.3514674645701,47.2392142866714,-28.1538607605649));
#20932=CARTESIAN_POINT('Ctrl Pts',(-18.9737180230564,46.5217702416014,-27.9959122373724));
#20933=CARTESIAN_POINT('Ctrl Pts',(-17.1026436278435,48.3843658671474,-27.8751508347916));
#20934=CARTESIAN_POINT('Ctrl Pts',(-16.9257886000388,49.6984507803992,-27.8070389399417));
#20935=CARTESIAN_POINT('Ctrl Pts',(-16.9282249073135,49.997407390353,-27.7915765528225));
#20936=CARTESIAN_POINT('Origin',(-20.,50.,-42.2084234471774));
#20937=CARTESIAN_POINT('',(-16.930022476882,50.0019420176801,-29.7915765528225));
#20938=CARTESIAN_POINT('',(-16.9251594783372,49.9974042565776,-29.7084234471774));
#20939=CARTESIAN_POINT('',(-16.9265,50.0000000000002,-42.2084234471774));
#20940=CARTESIAN_POINT('Ctrl Pts',(-16.9251594783372,49.9974042565776,-29.7084234471775));
#20941=CARTESIAN_POINT('Ctrl Pts',(-16.9325402148186,50.8197003396064,-29.6657846889788));
#20942=CARTESIAN_POINT('Ctrl Pts',(-17.6939854162501,52.6694193953535,-29.5704964230494));
#20943=CARTESIAN_POINT('Ctrl Pts',(-20.8103104076337,53.5347896383079,-29.4225586493891));
#20944=CARTESIAN_POINT('Ctrl Pts',(-23.4028291041448,51.2538320585774,-29.2646101261967));
#20945=CARTESIAN_POINT('Ctrl Pts',(-22.9101061444555,47.8360630851142,-29.1066616030042));
#20946=CARTESIAN_POINT('Ctrl Pts',(-19.7788784501499,46.3802698988112,-28.9487130798117));
#20947=CARTESIAN_POINT('Ctrl Pts',(-17.3157681767346,47.9150000634711,-28.8159670278695));
#20948=CARTESIAN_POINT('Ctrl Pts',(-16.9318839126521,49.4683179212627,-28.735870483658));
#20949=CARTESIAN_POINT('Ctrl Pts',(-16.9313401597895,50.0003484095168,-28.7084234471775));
#20950=CARTESIAN_POINT('Ctrl Pts',(-16.930022476882,50.0019420176801,-29.7915765528225));
#20951=CARTESIAN_POINT('Ctrl Pts',(-16.9278228426505,50.3777822124665,-29.7721663660449));
#20952=CARTESIAN_POINT('Ctrl Pts',(-17.1652525268972,51.7703947269283,-29.7001066715364));
#20953=CARTESIAN_POINT('Ctrl Pts',(-19.2351493401782,53.5449034469686,-29.5753974692971));
#20954=CARTESIAN_POINT('Ctrl Pts',(-22.5502121640569,52.5783240483645,-29.4174489461047));
#20955=CARTESIAN_POINT('Ctrl Pts',(-23.5530751799844,49.274056651322,-29.2595004229121));
#20956=CARTESIAN_POINT('Ctrl Pts',(-21.3344729921125,46.627980009892,-29.1015518997197));
#20957=CARTESIAN_POINT('Ctrl Pts',(-17.9487914181142,47.0340721357474,-28.9455772763565));
#20958=CARTESIAN_POINT('Ctrl Pts',(-16.9246871063329,49.0262581499145,-28.8422521607241));
#20959=CARTESIAN_POINT('Ctrl Pts',(-16.9217182551955,50.0006847935455,-28.7915765528225));
#20960=CARTESIAN_POINT('Origin',(-20.,50.,-42.2084234471774));
#20961=CARTESIAN_POINT('',(-16.9284009962433,49.9974440495234,-30.7915765528225));
#20962=CARTESIAN_POINT('',(-16.9237528526042,50.0022022524448,-30.7084234471775));
#20963=CARTESIAN_POINT('',(-16.9265,50.0000000000002,-42.2084234471774));
#20964=CARTESIAN_POINT('Ctrl Pts',(-16.9237528526042,50.0022022524448,-30.7084234471775));
#20965=CARTESIAN_POINT('Ctrl Pts',(-16.922592011601,50.1452351674692,-30.7009979097613));
#20966=CARTESIAN_POINT('Ctrl Pts',(-16.9963969117474,51.301214910621,-30.6409228646143));
#20967=CARTESIAN_POINT('Ctrl Pts',(-18.460564094239,53.2835160781738,-30.5281983117364));
#20968=CARTESIAN_POINT('Ctrl Pts',(-21.9079003148171,53.0840326088254,-30.3702497885439));
#20969=CARTESIAN_POINT('Ctrl Pts',(-23.6254013461144,50.0883505696652,-30.2123012653514));
#20970=CARTESIAN_POINT('Ctrl Pts',(-22.05586123849,47.0125637560539,-30.054352742159));
#20971=CARTESIAN_POINT('Ctrl Pts',(-18.6223342721148,46.6453945260559,-29.8964042189665));
#20972=CARTESIAN_POINT('Ctrl Pts',(-17.0275919910131,48.5977940122777,-29.7810944539727));
#20973=CARTESIAN_POINT('Ctrl Pts',(-16.9234266252383,49.8043451601994,-29.7184341967097));
#20974=CARTESIAN_POINT('Ctrl Pts',(-16.9251594783372,49.9974042565776,-29.7084234471775));
#20975=CARTESIAN_POINT('Ctrl Pts',(-16.9284009962433,49.9974440495234,-30.7915765528225));
#20976=CARTESIAN_POINT('Ctrl Pts',(-16.9340999379478,50.7099535572267,-30.7547300790965));
#20977=CARTESIAN_POINT('Ctrl Pts',(-17.534439538246,52.4492247638631,-30.6652340976396));
#20978=CARTESIAN_POINT('Ctrl Pts',(-20.4203163532235,53.6020370824496,-30.5230886084519));
#20979=CARTESIAN_POINT('Ctrl Pts',(-23.2459426566631,51.6171559138756,-30.3651400852594));
#20980=CARTESIAN_POINT('Ctrl Pts',(-23.1285714741897,48.166048661765,-30.207191562067));
#20981=CARTESIAN_POINT('Ctrl Pts',(-20.1746196872686,46.3777293109224,-30.0492430388745));
#20982=CARTESIAN_POINT('Ctrl Pts',(-17.4448107975432,47.689784542327,-29.9107047024597));
#20983=CARTESIAN_POINT('Ctrl Pts',(-16.9337892798002,49.3583277647774,-29.8248158737757));
#20984=CARTESIAN_POINT('Ctrl Pts',(-16.930022476882,50.0019420176801,-29.7915765528225));
#20985=CARTESIAN_POINT('Origin',(-20.,50.,-42.2084234471774));
#20986=CARTESIAN_POINT('',(-16.9216590200037,50.0005689006534,-31.7915765528225));
#20987=CARTESIAN_POINT('',(-16.9313142832549,50.0004533262794,-31.7084234471775));
#20988=CARTESIAN_POINT('',(-16.9265,50.0000000000002,-42.2084234471774));
#20989=CARTESIAN_POINT('Ctrl Pts',(-16.9313142832549,50.0004533262794,-31.7084234471775));
#20990=CARTESIAN_POINT('Ctrl Pts',(-16.9306731189746,50.4823621763928,-31.6835616228129));
#20991=CARTESIAN_POINT('Ctrl Pts',(-17.2638484234452,51.9839635458219,-31.6060502907175));
#20992=CARTESIAN_POINT('Ctrl Pts',(-19.6028209290277,53.604662193487,-31.4758894508912));
#20993=CARTESIAN_POINT('Ctrl Pts',(-22.8012444915916,52.3031218035313,-31.3179409276987));
#20994=CARTESIAN_POINT('Ctrl Pts',(-23.4598648696293,48.913410920597,-31.1599924045063));
#20995=CARTESIAN_POINT('Ctrl Pts',(-20.9815309974076,46.5088773088445,-31.0020438813138));
#20996=CARTESIAN_POINT('Ctrl Pts',(-17.7716226853989,47.2338732641192,-30.8515208955375));
#20997=CARTESIAN_POINT('Ctrl Pts',(-16.9308227569255,49.131084656435,-30.7536474174921));
#20998=CARTESIAN_POINT('Ctrl Pts',(-16.9237528526042,50.0022022524448,-30.7084234471775));
#20999=CARTESIAN_POINT('Ctrl Pts',(-16.9216590200037,50.0005689006534,-31.7915765528225));
#21000=CARTESIAN_POINT('Ctrl Pts',(-16.9215783383011,50.031972629415,-31.7899432998789));
#21001=CARTESIAN_POINT('Ctrl Pts',(-16.9361832221292,51.075629445688,-31.7356605392045));
#21002=CARTESIAN_POINT('Ctrl Pts',(-18.1119418547959,53.0962192138892,-31.6287282707992));
#21003=CARTESIAN_POINT('Ctrl Pts',(-21.56048739876,53.2735632052001,-31.4707797476067));
#21004=CARTESIAN_POINT('Ctrl Pts',(-23.5941864783473,50.4828669992804,-31.3128312244143));
#21005=CARTESIAN_POINT('Ctrl Pts',(-22.3691459902575,47.2543699708491,-31.1548827012218));
#21006=CARTESIAN_POINT('Ctrl Pts',(-18.9960728871194,46.5152521852863,-30.9969341780293));
#21007=CARTESIAN_POINT('Ctrl Pts',(-17.1077657383409,48.3710153180247,-30.8758321285629));
#21008=CARTESIAN_POINT('Ctrl Pts',(-16.9259567848863,49.6918568157852,-30.8073795868273));
#21009=CARTESIAN_POINT('Ctrl Pts',(-16.9284009962433,49.9974440495234,-30.7915765528225));
#21010=CARTESIAN_POINT('Origin',(-20.,50.,-42.2084234471774));
#21011=CARTESIAN_POINT('',(-16.9298915772933,50.0020159666225,-32.7915765528225));
#21012=CARTESIAN_POINT('',(-16.92535365788,49.9973711108991,-32.7084234471774));
#21013=CARTESIAN_POINT('',(-16.9265,50.0000000000002,-42.2084234471774));
#21014=CARTESIAN_POINT('Ctrl Pts',(-16.92535365788,49.9973711108991,-32.7084234471774));
#21015=CARTESIAN_POINT('Ctrl Pts',(-16.9327153463397,50.8132307133283,-32.6661253358645));
#21016=CARTESIAN_POINT('Ctrl Pts',(-17.6840554370644,52.6565961172178,-32.5711777168207));
#21017=CARTESIAN_POINT('Ctrl Pts',(-20.7875968246039,53.5399197710466,-32.423580590046));
#21018=CARTESIAN_POINT('Ctrl Pts',(-23.3947081018314,51.2756557713323,-32.2656320668536));
#21019=CARTESIAN_POINT('Ctrl Pts',(-22.9239407885082,47.8547934810673,-32.107683543661));
#21020=CARTESIAN_POINT('Ctrl Pts',(-19.8021252898838,46.3789246980118,-31.9497350204686));
#21021=CARTESIAN_POINT('Ctrl Pts',(-17.3228654131711,47.9017052850683,-31.8166483216407));
#21022=CARTESIAN_POINT('Ctrl Pts',(-16.9320309028298,49.4618311261562,-31.7362111305437));
#21023=CARTESIAN_POINT('Ctrl Pts',(-16.9313142832549,50.0004533262794,-31.7084234471775));
#21024=CARTESIAN_POINT('Ctrl Pts',(-16.9298915772933,50.0020159666225,-32.7915765528225));
#21025=CARTESIAN_POINT('Ctrl Pts',(-16.9276421184013,50.3712206119457,-32.7725070129305));
#21026=CARTESIAN_POINT('Ctrl Pts',(-17.1595660076359,51.75703964909,-32.7007879653076));
#21027=CARTESIAN_POINT('Ctrl Pts',(-19.2124032880871,53.5399192645472,-32.576419409954));
#21028=CARTESIAN_POINT('Ctrl Pts',(-22.5336041773036,52.5946458048986,-32.4184708867615));
#21029=CARTESIAN_POINT('Ctrl Pts',(-23.5576632150468,49.2968859065335,-32.260522363569));
#21030=CARTESIAN_POINT('Ctrl Pts',(-21.3560972171426,46.6366181724659,-32.1025738403766));
#21031=CARTESIAN_POINT('Ctrl Pts',(-17.9604780872831,47.0218018745157,-31.9462585701278));
#21032=CARTESIAN_POINT('Ctrl Pts',(-16.9241791919761,49.0196426858764,-31.8425928076097));
#21033=CARTESIAN_POINT('Ctrl Pts',(-16.9216590200037,50.0005689006534,-31.7915765528225));
#21034=CARTESIAN_POINT('Origin',(-20.,50.,-42.2084234471774));
#21035=CARTESIAN_POINT('',(-16.9285737782481,49.997484673902,-33.7915765528225));
#21036=CARTESIAN_POINT('',(-16.9235809537435,50.0021324683887,-33.7084234471775));
#21037=CARTESIAN_POINT('',(-16.9265,50.0000000000002,-42.2084234471774));
#21038=CARTESIAN_POINT('Ctrl Pts',(-16.9235809537435,50.0021324683887,-33.7084234471775));
#21039=CARTESIAN_POINT('Ctrl Pts',(-16.9224984391972,50.1385838243685,-33.7013385566469));
#21040=CARTESIAN_POINT('Ctrl Pts',(-16.9924898021293,51.2879206387911,-33.6416041583855));
#21041=CARTESIAN_POINT('Ctrl Pts',(-18.4395123779619,53.2735636735887,-33.5292202523933));
#21042=CARTESIAN_POINT('Ctrl Pts',(-21.8880584153516,53.0962196569031,-33.3712717292008));
#21043=CARTESIAN_POINT('Ctrl Pts',(-23.6247593102429,50.1116274445677,-33.2133232060084));
#21044=CARTESIAN_POINT('Ctrl Pts',(-22.0750011806081,47.025826023238,-33.0553746828159));
#21045=CARTESIAN_POINT('Ctrl Pts',(-18.6439025888241,46.6366176912258,-32.8974261596234));
#21046=CARTESIAN_POINT('Ctrl Pts',(-17.0319087206847,48.584474479988,-32.7817757477439));
#21047=CARTESIAN_POINT('Ctrl Pts',(-16.923552070216,49.7977100408445,-32.7187748435953));
#21048=CARTESIAN_POINT('Ctrl Pts',(-16.92535365788,49.9973711108991,-32.7084234471774));
#21049=CARTESIAN_POINT('Ctrl Pts',(-16.9285737782481,49.997484673902,-33.7915765528225));
#21050=CARTESIAN_POINT('Ctrl Pts',(-16.9341072631217,50.7035075960413,-33.7550707259821));
#21051=CARTESIAN_POINT('Ctrl Pts',(-17.5256619221046,52.4361499397914,-33.6659153914109));
#21052=CARTESIAN_POINT('Ctrl Pts',(-20.3971790141429,53.6046616777241,-33.5241105491088));
#21053=CARTESIAN_POINT('Ctrl Pts',(-23.2354919865996,51.6379647690895,-33.3661620259163));
#21054=CARTESIAN_POINT('Ctrl Pts',(-23.140282777847,48.1861750207679,-33.2082135027238));
#21055=CARTESIAN_POINT('Ctrl Pts',(-20.1978746818039,46.3789252161231,-33.0502649795314));
#21056=CARTESIAN_POINT('Ctrl Pts',(-17.4529645572674,47.6766083004955,-32.911385996231));
#21057=CARTESIAN_POINT('Ctrl Pts',(-16.9338526984151,49.3518754710422,-32.8251565206613));
#21058=CARTESIAN_POINT('Ctrl Pts',(-16.9298915772933,50.0020159666225,-32.7915765528225));
#21059=CARTESIAN_POINT('Origin',(-20.,50.,-42.2084234471774));
#21060=CARTESIAN_POINT('',(-16.921610115697,50.0004517332244,-34.7915765528225));
#21061=CARTESIAN_POINT('',(-16.931281639274,50.0005575828105,-34.7084234471775));
#21062=CARTESIAN_POINT('',(-16.9265,50.0000000000002,-42.2084234471774));
#21063=CARTESIAN_POINT('Ctrl Pts',(-16.931281639274,50.0005575828105,-34.7084234471775));
#21064=CARTESIAN_POINT('Ctrl Pts',(-16.9305033497428,50.4758508700281,-34.6839022696985));
#21065=CARTESIAN_POINT('Ctrl Pts',(-17.257259818676,51.9706346069805,-34.6067315844887));
#21066=CARTESIAN_POINT('Ctrl Pts',(-19.5796835866367,53.602037597837,-34.4769113915481));
#21067=CARTESIAN_POINT('Ctrl Pts',(-22.7863984030238,52.3210611114746,-34.3189628683556));
#21068=CARTESIAN_POINT('Ctrl Pts',(-23.4667705318659,48.935649107221,-34.1610143451632));
#21069=CARTESIAN_POINT('Ctrl Pts',(-21.0039272565248,46.515251686681,-34.0030658219707));
#21070=CARTESIAN_POINT('Ctrl Pts',(-17.7821552253656,47.2212159324729,-33.8522021893088));
#21071=CARTESIAN_POINT('Ctrl Pts',(-16.9305428624281,49.1245813227702,-33.7539880643777));
#21072=CARTESIAN_POINT('Ctrl Pts',(-16.9235809537435,50.0021324683887,-33.7084234471775));
#21073=CARTESIAN_POINT('Ctrl Pts',(-16.921610115697,50.0004517332244,-34.7915765528225));
#21074=CARTESIAN_POINT('Ctrl Pts',(-16.9215586294445,50.0253045384473,-34.7902839467645));
#21075=CARTESIAN_POINT('Ctrl Pts',(-16.9330438936165,51.0623952825175,-34.7363418329757));
#21076=CARTESIAN_POINT('Ctrl Pts',(-18.0920999581694,53.0840321675552,-34.6297502114561));
#21077=CARTESIAN_POINT('Ctrl Pts',(-21.5394356854951,53.2835156083612,-34.4718016882636));
#21078=CARTESIAN_POINT('Ctrl Pts',(-23.5910118966017,50.50593531068,-34.3138531650712));
#21079=CARTESIAN_POINT('Ctrl Pts',(-22.3867268367498,47.2696388541317,-34.1559046418787));
#21080=CARTESIAN_POINT('Ctrl Pts',(-19.0184691430321,46.5088778083619,-33.9979561186862));
#21081=CARTESIAN_POINT('Ctrl Pts',(-17.1129400582668,48.3576637140246,-33.8765134223342));
#21082=CARTESIAN_POINT('Ctrl Pts',(-16.9261267493285,49.6852657833083,-33.8077202337129));
#21083=CARTESIAN_POINT('Ctrl Pts',(-16.9285737782481,49.997484673902,-33.7915765528225));
#21084=CARTESIAN_POINT('Origin',(-20.,50.,-42.2084234471774));
#21085=CARTESIAN_POINT('',(-16.9297555423167,50.0020868944765,-35.7915765528225));
#21086=CARTESIAN_POINT('',(-16.9255488571744,49.9973424349028,-35.7084234471775));
#21087=CARTESIAN_POINT('',(-16.9265,50.0000000000002,-42.2084234471774));
#21088=CARTESIAN_POINT('Ctrl Pts',(-16.9255488571744,49.9973424349028,-35.7084234471775));
#21089=CARTESIAN_POINT('Ctrl Pts',(-16.9328791333409,50.8067639659031,-35.6664659827501));
#21090=CARTESIAN_POINT('Ctrl Pts',(-17.6741947628828,52.6437552934631,-35.5718590105919));
#21091=CARTESIAN_POINT('Ctrl Pts',(-20.7648507692583,53.5449039541813,-35.4246025307029));
#21092=CARTESIAN_POINT('Ctrl Pts',(-23.3864471368627,51.2974268891935,-35.2666540075105));
#21093=CARTESIAN_POINT('Ctrl Pts',(-22.9376548796072,47.8736123232374,-35.108705484318));
#21094=CARTESIAN_POINT('Ctrl Pts',(-19.8253802877465,46.3777287926399,-34.9507569611255));
#21095=CARTESIAN_POINT('Ctrl Pts',(-17.3300229730827,47.8884155251851,-34.817329615412));
#21096=CARTESIAN_POINT('Ctrl Pts',(-16.9321744179745,49.455346955759,-34.7365517774293));
#21097=CARTESIAN_POINT('Ctrl Pts',(-16.931281639274,50.0005575828105,-34.7084234471775));
#21098=CARTESIAN_POINT('Ctrl Pts',(-16.9297555423167,50.0020868944766,-35.7915765528225));
#21099=CARTESIAN_POINT('Ctrl Pts',(-16.9274619549591,50.3646558602159,-35.7728476598162));
#21100=CARTESIAN_POINT('Ctrl Pts',(-17.1539338868147,51.7436843363594,-35.7014692590789));
#21101=CARTESIAN_POINT('Ctrl Pts',(-19.1896897083071,53.5347891325428,-35.5774413506109));
#21102=CARTESIAN_POINT('Ctrl Pts',(-22.5168917309592,52.6108605850829,-35.4194928274184));
#21103=CARTESIAN_POINT('Ctrl Pts',(-23.562104568912,49.319744150915,-35.261544304226));
#21104=CARTESIAN_POINT('Ctrl Pts',(-21.3776655307659,46.6453950060402,-35.1035957810335));
#21105=CARTESIAN_POINT('Ctrl Pts',(-17.9722380655997,47.0095593747619,-34.946939863899));
#21106=CARTESIAN_POINT('Ctrl Pts',(-16.9236557307461,49.0130178076084,-34.8429334544954));
#21107=CARTESIAN_POINT('Ctrl Pts',(-16.921610115697,50.0004517332244,-34.7915765528225));
#21108=CARTESIAN_POINT('Origin',(-20.,50.,-42.2084234471774));
#21109=CARTESIAN_POINT('',(-16.9287430323014,49.9975291851057,-36.7915765528226));
#21110=CARTESIAN_POINT('',(-16.9234132972571,50.0020587543361,-36.7084234471775));
#21111=CARTESIAN_POINT('',(-16.9265,50.0000000000002,-42.2084234471774));
#21112=CARTESIAN_POINT('Ctrl Pts',(-16.9234132972571,50.0020587543361,-36.7084234471775));
#21113=CARTESIAN_POINT('Ctrl Pts',(-16.9224088816646,50.13193091024,-36.7016792035325));
#21114=CARTESIAN_POINT('Ctrl Pts',(-16.9886293991394,51.2746295929847,-36.6422854521568));
#21115=CARTESIAN_POINT('Ctrl Pts',(-18.4185250000732,53.263476300571,-36.5302421930502));
#21116=CARTESIAN_POINT('Ctrl Pts',(-21.8681386718888,53.1082790492255,-36.3722936698577));
#21117=CARTESIAN_POINT('Ctrl Pts',(-23.6239678268391,50.1348997169674,-36.2143451466652));
#21118=CARTESIAN_POINT('Ctrl Pts',(-22.09405557116,47.0392109146336,-36.0563966234728));
#21119=CARTESIAN_POINT('Ctrl Pts',(-18.6655268169483,46.6279795274162,-35.8984481002803));
#21120=CARTESIAN_POINT('Ctrl Pts',(-17.036274144185,48.5711523341288,-35.7824570415152));
#21121=CARTESIAN_POINT('Ctrl Pts',(-16.9236808789428,49.7910771093326,-35.7191154904809));
#21122=CARTESIAN_POINT('Ctrl Pts',(-16.9255488571744,49.9973424349028,-35.7084234471775));
#21123=CARTESIAN_POINT('Ctrl Pts',(-16.9287430323014,49.9975291851057,-36.7915765528226));
#21124=CARTESIAN_POINT('Ctrl Pts',(-16.9341064012563,50.6970615449486,-36.7554113728678));
#21125=CARTESIAN_POINT('Ctrl Pts',(-17.5169502765644,52.4230632555672,-36.6665966851821));
#21126=CARTESIAN_POINT('Ctrl Pts',(-20.3740252981191,53.6071376558454,-36.5251324897657));
#21127=CARTESIAN_POINT('Ctrl Pts',(-23.2249079190488,51.6587060907077,-36.3671839665732));
#21128=CARTESIAN_POINT('Ctrl Pts',(-23.1518646084073,48.2063761635784,-36.2092354433808));
#21129=CARTESIAN_POINT('Ctrl Pts',(-20.2211215182128,46.3802704167281,-36.0512869201883));
#21130=CARTESIAN_POINT('Ctrl Pts',(-17.4611824542364,47.6634413886959,-35.9120672900023));
#21131=CARTESIAN_POINT('Ctrl Pts',(-16.9339095461368,49.3454243680967,-35.825497167547));
#21132=CARTESIAN_POINT('Ctrl Pts',(-16.9297555423167,50.0020868944766,-35.7915765528225));
#21133=CARTESIAN_POINT('Origin',(-20.,50.,-42.2084234471774));
#21134=CARTESIAN_POINT('',(-16.9215718601367,50.0003336414566,-37.7915765528225));
#21135=CARTESIAN_POINT('',(-16.9312422659825,50.0006610027018,-37.7084234471775));
#21136=CARTESIAN_POINT('',(-16.9265,50.0000000000002,-42.2084234471774));
#21137=CARTESIAN_POINT('Ctrl Pts',(-16.9312422659825,50.0006610027018,-37.7084234471775));
#21138=CARTESIAN_POINT('Ctrl Pts',(-16.9303317311006,50.4693365215552,-37.6842429165841));
#21139=CARTESIAN_POINT('Ctrl Pts',(-17.250729318919,51.9573027298628,-37.60741287826));
#21140=CARTESIAN_POINT('Ctrl Pts',(-19.5565635760592,53.5992644563693,-37.477933332205));
#21141=CARTESIAN_POINT('Ctrl Pts',(-22.7714374310744,52.3389047405107,-37.3199848090126));
#21142=CARTESIAN_POINT('Ctrl Pts',(-23.4735332609671,48.9579311678064,-37.16203628582));
#21143=CARTESIAN_POINT('Ctrl Pts',(-21.0262821237837,46.5217697438983,-37.0040877626276));
#21144=CARTESIAN_POINT('Ctrl Pts',(-17.7927587355996,47.2085797455779,-36.85288348308));
#21145=CARTESIAN_POINT('Ctrl Pts',(-16.9302499368347,49.1180729542898,-36.7543287112633));
#21146=CARTESIAN_POINT('Ctrl Pts',(-16.9234132972571,50.0020587543361,-36.7084234471775));
#21147=CARTESIAN_POINT('Ctrl Pts',(-16.9215718601367,50.0003336414566,-37.7915765528225));
#21148=CARTESIAN_POINT('Ctrl Pts',(-16.921543415412,50.0186362548428,-37.7906245936502));
#21149=CARTESIAN_POINT('Ctrl Pts',(-16.9299478707484,51.0491651072969,-37.737023126747));
#21150=CARTESIAN_POINT('Ctrl Pts',(-18.0723368961882,53.0717177485,-37.630772152113));
#21151=CARTESIAN_POINT('Ctrl Pts',(-21.5183204151355,53.2933327434377,-37.4728236289205));
#21152=CARTESIAN_POINT('Ctrl Pts',(-23.5876893022666,50.5289827072374,-37.314875105728));
#21153=CARTESIAN_POINT('Ctrl Pts',(-22.4042092574597,47.2850203370204,-37.1569265825356));
#21154=CARTESIAN_POINT('Ctrl Pts',(-19.0409058781059,46.5026473552099,-36.9989780593431));
#21155=CARTESIAN_POINT('Ctrl Pts',(-17.1181668122877,48.3443111845633,-36.8771947161054));
#21156=CARTESIAN_POINT('Ctrl Pts',(-16.9262983733243,49.6786777173678,-36.8080608805986));
#21157=CARTESIAN_POINT('Ctrl Pts',(-16.9287430323014,49.9975291851057,-36.7915765528226));
#21158=CARTESIAN_POINT('Origin',(-20.,50.,-42.2084234471774));
#21159=CARTESIAN_POINT('',(-16.9296185387977,50.0021495995983,-38.7915765528225));
#21160=CARTESIAN_POINT('',(-16.9257449470869,49.9973154802779,-38.7084234471774));
#21161=CARTESIAN_POINT('',(-16.9265,50.0000000000002,-42.2084234471774));
#21162=CARTESIAN_POINT('Ctrl Pts',(-16.9257449470869,49.9973154802779,-38.7084234471774));
#21163=CARTESIAN_POINT('Ctrl Pts',(-16.9330319322419,50.8002972396456,-38.6668066296357));
#21164=CARTESIAN_POINT('Ctrl Pts',(-17.6644029527493,52.6309011816754,-38.5725403043632));
#21165=CARTESIAN_POINT('Ctrl Pts',(-20.7420733238179,53.5497397950539,-38.4256244713598));
#21166=CARTESIAN_POINT('Ctrl Pts',(-23.3780464773465,51.3191456129741,-38.2676759481674));
#21167=CARTESIAN_POINT('Ctrl Pts',(-22.951247888663,47.8925182840191,-38.1097274249748));
#21168=CARTESIAN_POINT('Ctrl Pts',(-19.8486424668251,46.3766825092365,-37.9517789017824));
#21169=CARTESIAN_POINT('Ctrl Pts',(-17.3372410903829,47.8751309362902,-37.8180109091832));
#21170=CARTESIAN_POINT('Ctrl Pts',(-16.9323142853343,49.4488653098967,-37.736892424315));
#21171=CARTESIAN_POINT('Ctrl Pts',(-16.9312422659825,50.0006610027018,-37.7084234471775));
#21172=CARTESIAN_POINT('Ctrl Pts',(-16.9296185387977,50.0021495995983,-38.7915765528225));
#21173=CARTESIAN_POINT('Ctrl Pts',(-16.9272827753867,50.3580876058963,-38.7731883067018));
#21174=CARTESIAN_POINT('Ctrl Pts',(-17.1483415218904,51.7303472358439,-38.7021505528502));
#21175=CARTESIAN_POINT('Ctrl Pts',(-19.167020277377,53.5294996249073,-38.5784632912678));
#21176=CARTESIAN_POINT('Ctrl Pts',(-22.5000701187915,52.6269745712345,-38.4205147680753));
#21177=CARTESIAN_POINT('Ctrl Pts',(-23.5664017687871,49.3426270004872,-38.2625662448828));
#21178=CARTESIAN_POINT('Ctrl Pts',(-21.3991756821973,46.6543118776375,-38.1046177216904));
#21179=CARTESIAN_POINT('Ctrl Pts',(-17.9840721502399,46.9973442210765,-37.9476211576703));
#21180=CARTESIAN_POINT('Ctrl Pts',(-16.9231165929177,49.0063831951071,-37.843274101381));
#21181=CARTESIAN_POINT('Ctrl Pts',(-16.9215718601367,50.0003336414566,-37.7915765528225));
#21182=CARTESIAN_POINT('Origin',(-20.,50.,-42.2084234471774));
#21183=CARTESIAN_POINT('',(-16.9296933173407,49.9966552073599,-39.7915765528226));
#21184=CARTESIAN_POINT('',(-16.9232550353076,50.0019104925463,-39.7084234471775));
#21185=CARTESIAN_POINT('',(-16.9265,50.0000000000002,-42.2084234471774));
#21186=CARTESIAN_POINT('',(-19.2062007174672,47.0307770462543,-40.));
#21187=CARTESIAN_POINT('Ctrl Pts',(-19.2062007174672,47.0307770462543,-40.));
#21188=CARTESIAN_POINT('Ctrl Pts',(-18.2239621276955,47.2933710986319,-39.9473504922692));
#21189=CARTESIAN_POINT('Ctrl Pts',(-17.1241890235734,48.3306038970069,-39.8778760098767));
#21190=CARTESIAN_POINT('Ctrl Pts',(-16.9273405012997,49.6711319064253,-39.8084015274842));
#21191=CARTESIAN_POINT('Ctrl Pts',(-16.9296933173407,49.9966552073599,-39.7915765528225));
#21192=CARTESIAN_POINT('',(-20.7956623919264,47.025713650831,-40.));
#21193=CARTESIAN_POINT('Origin',(-20.,50.,-40.));
#21194=CARTESIAN_POINT('Ctrl Pts',(-20.7956662771739,47.0257030918457,-40.));
#21195=CARTESIAN_POINT('Ctrl Pts',(-19.8486505232287,46.7747747443585,-39.9490537266973));
#21196=CARTESIAN_POINT('Ctrl Pts',(-17.7883283635535,47.2298889349752,-39.8518615424232));
#21197=CARTESIAN_POINT('Ctrl Pts',(-16.929936238593,49.1116774471724,-39.754669358149));
#21198=CARTESIAN_POINT('Ctrl Pts',(-16.9232550353076,50.0019104925463,-39.7084234471775));
#21199=CARTESIAN_POINT('Origin',(-20.,-50.,-32.));
#21200=CARTESIAN_POINT('',(-17.4865385565584,-49.9997270833425,-25.387416697508));
#21201=CARTESIAN_POINT('',(-17.4842343961705,-50.0033815919295,-25.112583302492));
#21202=CARTESIAN_POINT('',(-17.4825,-50.,-32.));
#21203=CARTESIAN_POINT('',(-18.0865340033349,-48.3640127966251,-25.));
#21204=CARTESIAN_POINT('Ctrl Pts',(-17.4842343961705,-50.0033815919295,
-25.112583302492));
#21205=CARTESIAN_POINT('Ctrl Pts',(-17.4894446223952,-49.4108204662451,
-25.0750555349947));
#21206=CARTESIAN_POINT('Ctrl Pts',(-17.7007781719159,-48.8151964396956,
-25.0375277674973));
#21207=CARTESIAN_POINT('Ctrl Pts',(-18.0865340033349,-48.3640127966251,
-25.));
#21208=CARTESIAN_POINT('',(-17.4825,-50.,-25.));
#21209=CARTESIAN_POINT('Origin',(-20.,-50.,-25.));
#21210=CARTESIAN_POINT('',(-17.4825,-50.,-24.));
#21211=CARTESIAN_POINT('',(-17.4825,-50.,-32.));
#21212=CARTESIAN_POINT('Origin',(-20.,-50.,-24.));
#21213=CARTESIAN_POINT('',(-21.9170728295299,-48.3614592401522,-25.));
#21214=CARTESIAN_POINT('Origin',(-20.,-50.,-25.));
#21215=CARTESIAN_POINT('Ctrl Pts',(-21.9170803467229,-48.3614539181488,
-25.));
#21216=CARTESIAN_POINT('Ctrl Pts',(-21.3942485321037,-47.7526835964708,
-25.0509462733027));
#21217=CARTESIAN_POINT('Ctrl Pts',(-20.5545526893521,-47.4126377534433,
-25.1018925466053));
#21218=CARTESIAN_POINT('Ctrl Pts',(-19.7559044819232,-47.4904264940795,
-25.152838819908));
#21219=CARTESIAN_POINT('Ctrl Pts',(-18.9305558892707,-47.5708158657842,
-25.2054883276388));
#21220=CARTESIAN_POINT('Ctrl Pts',(-18.1490454176151,-48.0974449024861,
-25.2581378353696));
#21221=CARTESIAN_POINT('Ctrl Pts',(-17.7651665339121,-48.8322009233391,
-25.3107873431004));
#21222=CARTESIAN_POINT('Ctrl Pts',(-17.5789261662639,-49.1886707300015,
-25.3363304612363));
#21223=CARTESIAN_POINT('Ctrl Pts',(-17.4862780881908,-49.5941282970916,
-25.3618735793722));
#21224=CARTESIAN_POINT('Ctrl Pts',(-17.4865385565584,-49.9997270833425,
-25.387416697508));
#21225=CARTESIAN_POINT('Origin',(-20.,-50.,-32.));
#21226=CARTESIAN_POINT('',(-17.4812439922137,-50.0020955261299,-26.387416697508));
#21227=CARTESIAN_POINT('',(-17.478641074515,-49.9993296596843,-26.112583302492));
#21228=CARTESIAN_POINT('',(-17.4825,-50.,-32.));
#21229=CARTESIAN_POINT('Ctrl Pts',(-17.478641074515,-49.9993296596843,-26.112583302492));
#21230=CARTESIAN_POINT('Ctrl Pts',(-17.4785132796901,-49.9628733193853,
-26.1102687557771));
#21231=CARTESIAN_POINT('Ctrl Pts',(-17.4792362609288,-49.9264222331827,
-26.1079542090622));
#21232=CARTESIAN_POINT('Ctrl Pts',(-17.4808258970162,-49.8900090632248,
-26.1056396623473));
#21233=CARTESIAN_POINT('Ctrl Pts',(-17.516985701843,-49.0617106059675,-26.0529901546164));
#21234=CARTESIAN_POINT('Ctrl Pts',(-18.0015840153798,-48.2530313826314,
-26.0003406468856));
#21235=CARTESIAN_POINT('Ctrl Pts',(-18.7149420635586,-47.8304732403596,
-25.9476911391548));
#21236=CARTESIAN_POINT('Ctrl Pts',(-19.4283001117373,-47.4079150980878,
-25.895041631424));
#21237=CARTESIAN_POINT('Ctrl Pts',(-20.3704178945579,-47.3714780368803,
-25.8423921236932));
#21238=CARTESIAN_POINT('Ctrl Pts',(-21.1141877060749,-47.7378804619289,
-25.7897426159623));
#21239=CARTESIAN_POINT('Ctrl Pts',(-21.8579575175919,-48.1042828869776,
-25.7370931082315));
#21240=CARTESIAN_POINT('Ctrl Pts',(-22.4033793578053,-48.8735247982823,
-25.6844436005007));
#21241=CARTESIAN_POINT('Ctrl Pts',(-22.5032201961104,-49.6964833362074,
-25.6317940927699));
#21242=CARTESIAN_POINT('Ctrl Pts',(-22.6030610344155,-50.5194418741325,
-25.5791445850391));
#21243=CARTESIAN_POINT('Ctrl Pts',(-22.2573208708123,-51.396117038678,-25.5264950773082));
#21244=CARTESIAN_POINT('Ctrl Pts',(-21.6226857101616,-51.9298779026354,
-25.4738455695774));
#21245=CARTESIAN_POINT('Ctrl Pts',(-20.988050549511,-52.4636387665928,-25.4211960618466));
#21246=CARTESIAN_POINT('Ctrl Pts',(-20.0645203918128,-52.654485329962,-25.3685465541158));
#21247=CARTESIAN_POINT('Ctrl Pts',(-19.2708512338734,-52.4142812621293,
-25.3158970463849));
#21248=CARTESIAN_POINT('Ctrl Pts',(-18.477182075934,-52.1740771942966,-25.2632475386541));
#21249=CARTESIAN_POINT('Ctrl Pts',(-17.8133739177533,-51.5028224952619,
-25.2105980309233));
#21250=CARTESIAN_POINT('Ctrl Pts',(-17.5804130530232,-50.7085531973994,
-25.1579485231925));
#21251=CARTESIAN_POINT('Ctrl Pts',(-17.5135031457353,-50.4804269619344,
-25.142826782959));
#21252=CARTESIAN_POINT('Ctrl Pts',(-17.4821349457426,-50.2421529341285,
-25.1277050427255));
#21253=CARTESIAN_POINT('Ctrl Pts',(-17.4842343961705,-50.0033815919295,
-25.112583302492));
#21254=CARTESIAN_POINT('Ctrl Pts',(-17.4865385565584,-49.9997270833425,
-25.387416697508));
#21255=CARTESIAN_POINT('Ctrl Pts',(-17.4868149659228,-50.4301490334305,
-25.414523087103));
#21256=CARTESIAN_POINT('Ctrl Pts',(-17.5917201630912,-50.8607300172153,
-25.4416294766979));
#21257=CARTESIAN_POINT('Ctrl Pts',(-17.800437027254,-51.2330950056298,-25.4687358662929));
#21258=CARTESIAN_POINT('Ctrl Pts',(-18.2058337000493,-51.9563500620634,
-25.5213853740237));
#21259=CARTESIAN_POINT('Ctrl Pts',(-19.0028743413902,-52.4599771699264,
-25.5740348817546));
#21260=CARTESIAN_POINT('Ctrl Pts',(-19.8301086932262,-52.5158218568911,
-25.6266843894854));
#21261=CARTESIAN_POINT('Ctrl Pts',(-20.6573430450623,-52.5716665438558,
-25.6793338972162));
#21262=CARTESIAN_POINT('Ctrl Pts',(-21.5147711073935,-52.1797288099222,
-25.731983404947));
#21263=CARTESIAN_POINT('Ctrl Pts',(-22.0137531835634,-51.5176087150676,
-25.7846329126778));
#21264=CARTESIAN_POINT('Ctrl Pts',(-22.5127352597332,-50.855488620213,-25.8372824204087));
#21265=CARTESIAN_POINT('Ctrl Pts',(-22.6532713497417,-49.9231861644375,
-25.8899319281395));
#21266=CARTESIAN_POINT('Ctrl Pts',(-22.3716202770373,-49.1433861401557,
-25.9425814358703));
#21267=CARTESIAN_POINT('Ctrl Pts',(-22.0899692043328,-48.3635861158738,
-25.9952309436012));
#21268=CARTESIAN_POINT('Ctrl Pts',(-21.3861309689154,-47.7362885230857,
-26.0478804513319));
#21269=CARTESIAN_POINT('Ctrl Pts',(-20.5791956401472,-47.5458492720573,
-26.1005299590628));
#21270=CARTESIAN_POINT('Ctrl Pts',(-19.7722603113789,-47.355410021029,-26.1531794667936));
#21271=CARTESIAN_POINT('Ctrl Pts',(-18.8622278892599,-47.6018291117603,
-26.2058289745244));
#21272=CARTESIAN_POINT('Ctrl Pts',(-18.2616398443447,-48.1734061983061,
-26.2584784822553));
#21273=CARTESIAN_POINT('Ctrl Pts',(-17.7713614356055,-48.6400020735255,
-26.3014578873395));
#21274=CARTESIAN_POINT('Ctrl Pts',(-17.4872954214302,-49.3232818307864,
-26.3444372924238));
#21275=CARTESIAN_POINT('Ctrl Pts',(-17.4812439922137,-50.0020955261299,
-26.387416697508));
#21276=CARTESIAN_POINT('Origin',(-20.,-50.,-32.));
#21277=CARTESIAN_POINT('',(-17.4803938764511,-49.9981422851833,-27.387416697508));
#21278=CARTESIAN_POINT('',(-17.4854882815929,-49.9984719969074,-27.112583302492));
#21279=CARTESIAN_POINT('',(-17.4825,-50.,-32.));
#21280=CARTESIAN_POINT('Ctrl Pts',(-17.4854882815929,-49.9984719969074,
-27.112583302492));
#21281=CARTESIAN_POINT('Ctrl Pts',(-17.4837320581771,-49.6851867695493,
-27.0928324688287));
#21282=CARTESIAN_POINT('Ctrl Pts',(-17.5380281914022,-49.372488365388,-27.0730816351654));
#21283=CARTESIAN_POINT('Ctrl Pts',(-17.6511655615397,-49.0827678639941,
-27.0533308015021));
#21284=CARTESIAN_POINT('Ctrl Pts',(-17.9527541904173,-48.3104641709981,
-27.0006812937713));
#21285=CARTESIAN_POINT('Ctrl Pts',(-18.6724614894036,-47.7014386592764,
-26.9480317860404));
#21286=CARTESIAN_POINT('Ctrl Pts',(-19.4840192035288,-47.5317821658037,
-26.8953822783096));
#21287=CARTESIAN_POINT('Ctrl Pts',(-20.295576917654,-47.362125672331,-26.8427327705788));
#21288=CARTESIAN_POINT('Ctrl Pts',(-21.1989850469181,-47.6318381971073,
-26.790083262848));
#21289=CARTESIAN_POINT('Ctrl Pts',(-21.7846970457346,-48.2186528878745,
-26.7374337551172));
#21290=CARTESIAN_POINT('Ctrl Pts',(-22.3704090445512,-48.8054675786417,
-26.6847842473863));
#21291=CARTESIAN_POINT('Ctrl Pts',(-22.6384249129202,-49.7093844353998,
-26.6321347396555));
#21292=CARTESIAN_POINT('Ctrl Pts',(-22.4672441468777,-50.5206200888683,
-26.5794852319247));
#21293=CARTESIAN_POINT('Ctrl Pts',(-22.2960633808352,-51.3318557423367,
-26.5268357241939));
#21294=CARTESIAN_POINT('Ctrl Pts',(-21.6856859803813,-52.0504101925156,
-26.474186216463));
#21295=CARTESIAN_POINT('Ctrl Pts',(-20.9128164334925,-52.3505504609625,
-26.4215367087322));
#21296=CARTESIAN_POINT('Ctrl Pts',(-20.1399468866037,-52.6506907294095,
-26.3688872010014));
#21297=CARTESIAN_POINT('Ctrl Pts',(-19.2045851932801,-52.5324168161245,
-26.3162376932706));
#21298=CARTESIAN_POINT('Ctrl Pts',(-18.5307649946765,-52.0493210138927,
-26.2635881855398));
#21299=CARTESIAN_POINT('Ctrl Pts',(-17.8865668836162,-51.5874627853863,
-26.2132532245238));
#21300=CARTESIAN_POINT('Ctrl Pts',(-17.4814202569298,-50.7921537819725,
-26.1629182635079));
#21301=CARTESIAN_POINT('Ctrl Pts',(-17.478641074515,-49.9993296596843,-26.112583302492));
#21302=CARTESIAN_POINT('Ctrl Pts',(-17.4812439922137,-50.0020955261299,
-26.387416697508));
#21303=CARTESIAN_POINT('Ctrl Pts',(-17.4798824577399,-50.154824445923,-26.3970868001546));
#21304=CARTESIAN_POINT('Ctrl Pts',(-17.4925946446391,-50.3073272836526,
-26.4067569028011));
#21305=CARTESIAN_POINT('Ctrl Pts',(-17.5201983578819,-50.4570852091481,
-26.4164270054477));
#21306=CARTESIAN_POINT('Ctrl Pts',(-17.6704885840456,-51.2724520510841,
-26.4690765131785));
#21307=CARTESIAN_POINT('Ctrl Pts',(-18.2622127040842,-52.0064506525957,
-26.5217260209094));
#21308=CARTESIAN_POINT('Ctrl Pts',(-19.0271195964254,-52.3263364322528,
-26.5743755286402));
#21309=CARTESIAN_POINT('Ctrl Pts',(-19.7920264887666,-52.6462222119098,
-26.627025036371));
#21310=CARTESIAN_POINT('Ctrl Pts',(-20.7301161534105,-52.5519951697124,
-26.6796745441018));
#21311=CARTESIAN_POINT('Ctrl Pts',(-21.4161209056844,-52.08637043532,-26.7323240518326));
#21312=CARTESIAN_POINT('Ctrl Pts',(-22.1021256579584,-51.6207457009276,
-26.7849735595635));
#21313=CARTESIAN_POINT('Ctrl Pts',(-22.5360454978625,-50.7837232743402,
-26.8376230672943));
#21314=CARTESIAN_POINT('Ctrl Pts',(-22.5211689625615,-49.9547551805518,
-26.8902725750251));
#21315=CARTESIAN_POINT('Ctrl Pts',(-22.5062924272606,-49.1257870867634,
-26.942922082756));
#21316=CARTESIAN_POINT('Ctrl Pts',(-22.0426195167546,-48.3048733257741,
-26.9955715904868));
#21317=CARTESIAN_POINT('Ctrl Pts',(-21.3403495461317,-47.8641623480534,
-27.0482210982176));
#21318=CARTESIAN_POINT('Ctrl Pts',(-20.6380795755089,-47.4234513703327,
-27.1008706059484));
#21319=CARTESIAN_POINT('Ctrl Pts',(-19.697212544769,-47.3629431758806,-27.1535201136792));
#21320=CARTESIAN_POINT('Ctrl Pts',(-18.9442760880979,-47.7100683950257,
-27.2061696214101));
#21321=CARTESIAN_POINT('Ctrl Pts',(-18.1913396314267,-48.0571936141707,
-27.2588191291409));
#21322=CARTESIAN_POINT('Ctrl Pts',(-17.6263337488242,-48.811952246913,-27.3114686368717));
#21323=CARTESIAN_POINT('Ctrl Pts',(-17.5053953288183,-49.632185863958,-27.3641181446025));
#21324=CARTESIAN_POINT('Ctrl Pts',(-17.4875560345985,-49.7531762723222,
-27.3718843289044));
#21325=CARTESIAN_POINT('Ctrl Pts',(-17.4793789333885,-49.875591310926,-27.3796505132062));
#21326=CARTESIAN_POINT('Ctrl Pts',(-17.4803938764511,-49.9981422851833,
-27.387416697508));
#21327=CARTESIAN_POINT('Origin',(-20.,-50.,-32.));
#21328=CARTESIAN_POINT('',(-17.4864646543277,-49.9997146182113,-28.387416697508));
#21329=CARTESIAN_POINT('',(-17.4839129917625,-50.00212360321,-28.112583302492));
#21330=CARTESIAN_POINT('',(-17.4825,-50.,-32.));
#21331=CARTESIAN_POINT('Ctrl Pts',(-17.4839129917625,-50.00212360321,-28.112583302492));
#21332=CARTESIAN_POINT('Ctrl Pts',(-17.4887123626501,-49.4131980331168,
-28.0753961818803));
#21333=CARTESIAN_POINT('Ctrl Pts',(-17.6952668319888,-48.8212389436082,
-28.0382090612686));
#21334=CARTESIAN_POINT('Ctrl Pts',(-18.0729549967146,-48.3737050608961,
-28.0010219406569));
#21335=CARTESIAN_POINT('Ctrl Pts',(-18.6076857212633,-47.7400868019379,
-27.9483724329261));
#21336=CARTESIAN_POINT('Ctrl Pts',(-19.4854519355195,-47.3959671798642,
-27.8957229251952));
#21337=CARTESIAN_POINT('Ctrl Pts',(-20.3083316759583,-47.4973475663696,
-27.8430734174644));
#21338=CARTESIAN_POINT('Ctrl Pts',(-21.131211416397,-47.598727952875,-27.7904239097336));
#21339=CARTESIAN_POINT('Ctrl Pts',(-21.8992046830182,-48.1456083479595,
-27.7377744020028));
#21340=CARTESIAN_POINT('Ctrl Pts',(-22.2641534037816,-48.8900688925903,
-27.685124894272));
#21341=CARTESIAN_POINT('Ctrl Pts',(-22.629102124545,-49.6345294372211,-27.6324753865412));
#21342=CARTESIAN_POINT('Ctrl Pts',(-22.5910062994507,-50.5765701313981,
-27.5798258788103));
#21343=CARTESIAN_POINT('Ctrl Pts',(-22.1671360981513,-51.2891310488058,
-27.5271763710795));
#21344=CARTESIAN_POINT('Ctrl Pts',(-21.743265896852,-52.0016919662134,-27.4745268633487));
#21345=CARTESIAN_POINT('Ctrl Pts',(-20.9336213193477,-52.4847731068517,
-27.4218773556179));
#21346=CARTESIAN_POINT('Ctrl Pts',(-20.1052424094757,-52.5193771868443,
-27.369227847887));
#21347=CARTESIAN_POINT('Ctrl Pts',(-19.2768634996038,-52.5539812668369,
-27.3165783401562));
#21348=CARTESIAN_POINT('Ctrl Pts',(-18.4297502573642,-52.1401082861839,
-27.2639288324254));
#21349=CARTESIAN_POINT('Ctrl Pts',(-17.9479286156288,-51.4653808587222,
-27.2112793246945));
#21350=CARTESIAN_POINT('Ctrl Pts',(-17.646856605019,-51.0437693626761,-27.178380650627));
#21351=CARTESIAN_POINT('Ctrl Pts',(-17.4884135971887,-50.5203066070677,
-27.1454819765595));
#21352=CARTESIAN_POINT('Ctrl Pts',(-17.4854882815929,-49.9984719969074,
-27.112583302492));
#21353=CARTESIAN_POINT('Ctrl Pts',(-17.4803938764511,-49.9981422851833,
-27.387416697508));
#21354=CARTESIAN_POINT('Ctrl Pts',(-17.4862595649243,-50.7064045154313,
-27.432300020937));
#21355=CARTESIAN_POINT('Ctrl Pts',(-17.7991453021895,-51.4192070818358,
-27.477183344366));
#21356=CARTESIAN_POINT('Ctrl Pts',(-18.3282967869582,-51.887789182872,-27.522066667795));
#21357=CARTESIAN_POINT('Ctrl Pts',(-18.9490076225134,-52.4374502833933,
-27.5747161755258));
#21358=CARTESIAN_POINT('Ctrl Pts',(-19.8673002510331,-52.6510638830879,
-27.6273656832566));
#21359=CARTESIAN_POINT('Ctrl Pts',(-20.6668806897214,-52.4317914845825,
-27.6800151909875));
#21360=CARTESIAN_POINT('Ctrl Pts',(-21.4664611284097,-52.2125190860771,
-27.7326646987183));
#21361=CARTESIAN_POINT('Ctrl Pts',(-22.1473293772665,-51.5603606893716,
-27.7853142064491));
#21362=CARTESIAN_POINT('Ctrl Pts',(-22.4008241614529,-50.7709623965743,
-27.8379637141799));
#21363=CARTESIAN_POINT('Ctrl Pts',(-22.6543189456393,-49.981564103777,-27.8906132219107));
#21364=CARTESIAN_POINT('Ctrl Pts',(-22.4804402651553,-49.0549259148879,
-27.9432627296416));
#21365=CARTESIAN_POINT('Ctrl Pts',(-21.9580133797035,-48.4111251564977,
-27.9959122373724));
#21366=CARTESIAN_POINT('Ctrl Pts',(-21.4355864942518,-47.7673243981074,
-28.0485617451032));
#21367=CARTESIAN_POINT('Ctrl Pts',(-20.5646114038323,-47.4063610702159,
-28.1012112528341));
#21368=CARTESIAN_POINT('Ctrl Pts',(-19.7399314188999,-47.4918724109971,
-28.1538607605649));
#21369=CARTESIAN_POINT('Ctrl Pts',(-18.9152514339676,-47.5773837517783,
-28.2065102682957));
#21370=CARTESIAN_POINT('Ctrl Pts',(-18.1368665545222,-48.1093697612321,
-28.2591597760265));
#21371=CARTESIAN_POINT('Ctrl Pts',(-17.757645729928,-48.8466626704905,-28.3118092837573));
#21372=CARTESIAN_POINT('Ctrl Pts',(-17.576118829844,-49.1995929095268,-28.3370117550076));
#21373=CARTESIAN_POINT('Ctrl Pts',(-17.4860556899587,-49.5995668160042,
-28.3622142262578));
#21374=CARTESIAN_POINT('Ctrl Pts',(-17.4864646543277,-49.9997146182113,
-28.387416697508));
#21375=CARTESIAN_POINT('Origin',(-20.,-50.,-32.));
#21376=CARTESIAN_POINT('',(-17.4814020660648,-50.0021261701134,-29.387416697508));
#21377=CARTESIAN_POINT('',(-17.4785834014225,-49.9994390864922,-29.112583302492));
#21378=CARTESIAN_POINT('',(-17.4825,-50.,-32.));
#21379=CARTESIAN_POINT('Ctrl Pts',(-17.4785834014225,-49.9994390864922,
-29.112583302492));
#21380=CARTESIAN_POINT('Ctrl Pts',(-17.4784886794343,-49.968349744285,-29.1106094026627));
#21381=CARTESIAN_POINT('Ctrl Pts',(-17.4790144707734,-49.9372636795263,
-29.1086355028335));
#21382=CARTESIAN_POINT('Ctrl Pts',(-17.4801707545743,-49.906201084417,-29.1066616030042));
#21383=CARTESIAN_POINT('Ctrl Pts',(-17.5110121235283,-49.0776735588066,
-29.0540120952734));
#21384=CARTESIAN_POINT('Ctrl Pts',(-17.9904111854216,-48.2658432856158,
-29.0013625875425));
#21385=CARTESIAN_POINT('Ctrl Pts',(-18.7010396656628,-47.8387411740548,
-28.9487130798117));
#21386=CARTESIAN_POINT('Ctrl Pts',(-19.411668145904,-47.4116390624939,-28.8960635720809));
#21387=CARTESIAN_POINT('Ctrl Pts',(-20.3535260444932,-47.3692651125628,
-28.8434140643501));
#21388=CARTESIAN_POINT('Ctrl Pts',(-21.0996364057885,-47.730828909672,-28.7907645566192));
#21389=CARTESIAN_POINT('Ctrl Pts',(-21.8457467670838,-48.0923927067812,
-28.7381150488884));
#21390=CARTESIAN_POINT('Ctrl Pts',(-22.3961095910853,-48.8578942509305,
-28.6854655411576));
#21391=CARTESIAN_POINT('Ctrl Pts',(-22.5012262607424,-49.680305058751,-28.6328160334268));
#21392=CARTESIAN_POINT('Ctrl Pts',(-22.6063429303995,-50.5027158665715,
-28.580166525696));
#21393=CARTESIAN_POINT('Ctrl Pts',(-22.2662134457122,-51.3820359380631,
-28.5275170179651));
#21394=CARTESIAN_POINT('Ctrl Pts',(-21.6350303363852,-51.9196388888135,
-28.4748675102343));
#21395=CARTESIAN_POINT('Ctrl Pts',(-21.0038472270583,-52.457241839564,-28.4222180025035));
#21396=CARTESIAN_POINT('Ctrl Pts',(-20.0816104930917,-52.6531276695732,
-28.3695684947727));
#21397=CARTESIAN_POINT('Ctrl Pts',(-19.2864021333348,-52.4184945199041,
-28.3169189870418));
#21398=CARTESIAN_POINT('Ctrl Pts',(-18.491193773578,-52.183861370235,-28.264269479311));
#21399=CARTESIAN_POINT('Ctrl Pts',(-17.8230137880308,-51.5187092408875,
-28.2116199715802));
#21400=CARTESIAN_POINT('Ctrl Pts',(-17.5847714126778,-50.7245747282924,
-28.1589704638494));
#21401=CARTESIAN_POINT('Ctrl Pts',(-17.5148031262748,-50.4913490859714,
-28.1435080767302));
#21402=CARTESIAN_POINT('Ctrl Pts',(-17.4819174156229,-50.2469985760325,
-28.1280456896111));
#21403=CARTESIAN_POINT('Ctrl Pts',(-17.4839129917625,-50.00212360321,-28.112583302492));
#21404=CARTESIAN_POINT('Ctrl Pts',(-17.4864646543277,-49.9997146182113,
-28.387416697508));
#21405=CARTESIAN_POINT('Ctrl Pts',(-17.4869100416013,-50.4355001098706,
-28.4148637339886));
#21406=CARTESIAN_POINT('Ctrl Pts',(-17.5946602795742,-50.871491851351,-28.4423107704692));
#21407=CARTESIAN_POINT('Ctrl Pts',(-17.808434460022,-51.2471488088293,-28.4697578069498));
#21408=CARTESIAN_POINT('Ctrl Pts',(-18.2185007844534,-51.9677422288466,
-28.5224073146806));
#21409=CARTESIAN_POINT('Ctrl Pts',(-19.0186902030594,-52.4663292598182,
-28.5750568224114));
#21410=CARTESIAN_POINT('Ctrl Pts',(-19.846249011503,-52.5168830528463,-28.6277063301423));
#21411=CARTESIAN_POINT('Ctrl Pts',(-20.6738078199465,-52.5674368458744,
-28.6803558378731));
#21412=CARTESIAN_POINT('Ctrl Pts',(-21.5287360182276,-52.169957400959,-28.7330053456039));
#21413=CARTESIAN_POINT('Ctrl Pts',(-22.023464908259,-51.5046359802209,-28.7856548533348));
#21414=CARTESIAN_POINT('Ctrl Pts',(-22.5181937982904,-50.8393145594829,
-28.8383043610656));
#21415=CARTESIAN_POINT('Ctrl Pts',(-22.6527233800722,-49.9061511629222,
-28.8909538687964));
#21416=CARTESIAN_POINT('Ctrl Pts',(-22.3660667135347,-49.1281812258465,
-28.9436033765272));
#21417=CARTESIAN_POINT('Ctrl Pts',(-22.0794100469972,-48.3502112887709,
-28.996252884258));
#21418=CARTESIAN_POINT('Ctrl Pts',(-21.3715671321404,-47.7274348111802,
-29.0489023919889));
#21419=CARTESIAN_POINT('Ctrl Pts',(-20.5634277903475,-47.5421780387863,
-29.1015518997197));
#21420=CARTESIAN_POINT('Ctrl Pts',(-19.7552884485545,-47.3569212663924,
-29.1542014074505));
#21421=CARTESIAN_POINT('Ctrl Pts',(-18.8468526798254,-47.6091841991953,
-29.2068509151813));
#21422=CARTESIAN_POINT('Ctrl Pts',(-18.2499460255173,-48.1846072727033,
-29.2595004229121));
#21423=CARTESIAN_POINT('Ctrl Pts',(-17.7665348865127,-48.6506197075898,
-29.3021391811108));
#21424=CARTESIAN_POINT('Ctrl Pts',(-17.4874476178656,-49.3285845014614,
-29.3447779393094));
#21425=CARTESIAN_POINT('Ctrl Pts',(-17.4814020660648,-50.0021261701134,
-29.387416697508));
#21426=CARTESIAN_POINT('Origin',(-20.,-50.,-32.));
#21427=CARTESIAN_POINT('',(-17.4802499007281,-49.9981961378425,-30.387416697508));
#21428=CARTESIAN_POINT('',(-17.4853853786729,-49.9984092958285,-30.112583302492));
#21429=CARTESIAN_POINT('',(-17.4825,-50.,-32.));
#21430=CARTESIAN_POINT('Ctrl Pts',(-17.4853853786729,-49.9984092958285,
-30.112583302492));
#21431=CARTESIAN_POINT('Ctrl Pts',(-17.4835836611168,-49.6905590780416,
-30.0931731157143));
#21432=CARTESIAN_POINT('Ctrl Pts',(-17.5359688547378,-49.3833006303856,
-30.0737629289367));
#21433=CARTESIAN_POINT('Ctrl Pts',(-17.6453244230335,-49.0978688621381,
-30.054352742159));
#21434=CARTESIAN_POINT('Ctrl Pts',(-17.9419478870084,-48.3236443654287,
-30.0017032344282));
#21435=CARTESIAN_POINT('Ctrl Pts',(-18.657729850048,-47.7100092668519,-29.9490537266973));
#21436=CARTESIAN_POINT('Ctrl Pts',(-19.4681814439702,-47.5351457069169,
-29.8964042189665));
#21437=CARTESIAN_POINT('Ctrl Pts',(-20.2786330378925,-47.3602821469818,
-29.8437547112357));
#21438=CARTESIAN_POINT('Ctrl Pts',(-21.1837542626973,-47.6241901256886,
-29.7911052035049));
#21439=CARTESIAN_POINT('Ctrl Pts',(-21.7732221751288,-48.2072309740829,
-29.7384556957741));
#21440=CARTESIAN_POINT('Ctrl Pts',(-22.3626900875602,-48.7902718224772,
-29.6858061880432));
#21441=CARTESIAN_POINT('Ctrl Pts',(-22.6365046876183,-49.6924455405591,
-29.6331566803124));
#21442=CARTESIAN_POINT('Ctrl Pts',(-22.470536290213,-50.5047653924361,-29.5805071725816));
#21443=CARTESIAN_POINT('Ctrl Pts',(-22.3045678928078,-51.317085244313,-29.5278576648508));
#21444=CARTESIAN_POINT('Ctrl Pts',(-21.6988164979394,-52.0395512299852,
-29.4752081571199));
#21445=CARTESIAN_POINT('Ctrl Pts',(-20.9278902889251,-52.3446443812263,
-29.4225586493891));
#21446=CARTESIAN_POINT('Ctrl Pts',(-20.1569640799107,-52.6497375324674,
-29.3699091416583));
#21447=CARTESIAN_POINT('Ctrl Pts',(-19.2208630567505,-52.5374578492774,
-29.3172596339275));
#21448=CARTESIAN_POINT('Ctrl Pts',(-18.5439543831779,-52.0587056186674,
-29.2646101261966));
#21449=CARTESIAN_POINT('Ctrl Pts',(-17.892423912988,-51.5979024437465,-29.2139345182951));
#21450=CARTESIAN_POINT('Ctrl Pts',(-17.481015183552,-50.7975906908716,-29.1632589103935));
#21451=CARTESIAN_POINT('Ctrl Pts',(-17.4785834014225,-49.9994390864922,
-29.112583302492));
#21452=CARTESIAN_POINT('Ctrl Pts',(-17.4814020660648,-50.0021261701134,
-29.387416697508));
#21453=CARTESIAN_POINT('Ctrl Pts',(-17.4799826883104,-50.160260628743,-29.3974274470402));
#21454=CARTESIAN_POINT('Ctrl Pts',(-17.4936138858681,-50.3181512763535,
-29.4074381965724));
#21455=CARTESIAN_POINT('Ctrl Pts',(-17.5231849738733,-50.4729978797759,
-29.4174489461046));
#21456=CARTESIAN_POINT('Ctrl Pts',(-17.6787081164242,-51.2873821991274,
-29.4700984538354));
#21457=CARTESIAN_POINT('Ctrl Pts',(-18.2751319414129,-52.0175676236174,
-29.5227479615662));
#21458=CARTESIAN_POINT('Ctrl Pts',(-19.0420767774903,-52.3325356948411,
-29.5753974692971));
#21459=CARTESIAN_POINT('Ctrl Pts',(-19.8090216135677,-52.6475037660647,
-29.6280469770279));
#21460=CARTESIAN_POINT('Ctrl Pts',(-20.7464874607337,-52.5472544840221,
-29.6806964847587));
#21461=CARTESIAN_POINT('Ctrl Pts',(-21.4294884330411,-52.0772343362577,
-29.7333459924896));
#21462=CARTESIAN_POINT('Ctrl Pts',(-22.1124894053484,-51.6072141884932,
-29.7859955002204));
#21463=CARTESIAN_POINT('Ctrl Pts',(-22.5410255027971,-50.767423175007,-29.8386450079512));
#21464=CARTESIAN_POINT('Ctrl Pts',(-22.5208264022779,-49.9385677812172,
-29.891294515682));
#21465=CARTESIAN_POINT('Ctrl Pts',(-22.5006273017587,-49.1097123874274,
-29.9439440234128));
#21466=CARTESIAN_POINT('Ctrl Pts',(-22.0316930032716,-48.2917926133339,
-29.9965935311437));
#21467=CARTESIAN_POINT('Ctrl Pts',(-21.3266077400392,-47.85559995057,-30.0492430388745));
#21468=CARTESIAN_POINT('Ctrl Pts',(-20.6215224768069,-47.4194072878061,
-30.1018925466053));
#21469=CARTESIAN_POINT('Ctrl Pts',(-19.6802862488292,-47.3649417363718,
-30.1545420543361));
#21470=CARTESIAN_POINT('Ctrl Pts',(-18.9295941868573,-47.716894425762,-30.207191562067));
#21471=CARTESIAN_POINT('Ctrl Pts',(-18.1789021248854,-48.0688471151522,
-30.2598410697978));
#21472=CARTESIAN_POINT('Ctrl Pts',(-17.6187542289192,-48.8272180453669,
-30.3124905775286));
#21473=CARTESIAN_POINT('Ctrl Pts',(-17.5030850295308,-49.6482112875982,
-30.3651400852594));
#21474=CARTESIAN_POINT('Ctrl Pts',(-17.4867713733357,-49.7640018486382,
-30.3725656226756));
#21475=CARTESIAN_POINT('Ctrl Pts',(-17.4792990573488,-49.8810380603009,
-30.3799911600918));
#21476=CARTESIAN_POINT('Ctrl Pts',(-17.4802499007281,-49.9981961378425,
-30.387416697508));
#21477=CARTESIAN_POINT('Origin',(-20.,-50.,-32.));
#21478=CARTESIAN_POINT('',(-17.4864434588916,-49.999628681025,-31.387416697508));
#21479=CARTESIAN_POINT('',(-17.4840572259774,-50.0020935757321,-31.112583302492));
#21480=CARTESIAN_POINT('',(-17.4825,-50.,-32.));
#21481=CARTESIAN_POINT('Ctrl Pts',(-17.4840572259774,-50.0020935757321,
-31.112583302492));
#21482=CARTESIAN_POINT('Ctrl Pts',(-17.4887252217618,-49.4184779588706,
-31.0757368287659));
#21483=CARTESIAN_POINT('Ctrl Pts',(-17.6911788800261,-48.8319402420143,
-31.0388903550399));
#21484=CARTESIAN_POINT('Ctrl Pts',(-18.0625522849953,-48.3861121432124,
-31.0020438813138));
#21485=CARTESIAN_POINT('Ctrl Pts',(-18.5932035245498,-47.7490734374465,
-30.949394373583));
#21486=CARTESIAN_POINT('Ctrl Pts',(-19.468742053114,-47.3993247593714,-30.8967448658521));
#21487=CARTESIAN_POINT('Ctrl Pts',(-20.2922557929138,-47.4954193536299,
-30.8440953581213));
#21488=CARTESIAN_POINT('Ctrl Pts',(-21.1157695327135,-47.5915139478884,
-30.7914458503905));
#21489=CARTESIAN_POINT('Ctrl Pts',(-21.8872584837488,-48.1334518144805,
-30.7387963426597));
#21490=CARTESIAN_POINT('Ctrl Pts',(-22.2569798619555,-48.8755536627342,
-30.6861468349289));
#21491=CARTESIAN_POINT('Ctrl Pts',(-22.6267012401623,-49.6176555109878,
-30.6334973271981));
#21492=CARTESIAN_POINT('Ctrl Pts',(-22.5946550455406,-50.559921340903,-30.5808478194672));
#21493=CARTESIAN_POINT('Ctrl Pts',(-22.1753689331017,-51.2751892673478,
-30.5281983117364));
#21494=CARTESIAN_POINT('Ctrl Pts',(-21.7560828206629,-51.9904571937926,
-30.4755488040056));
#21495=CARTESIAN_POINT('Ctrl Pts',(-20.9495567904068,-52.478727216767,-30.4228992962747));
#21496=CARTESIAN_POINT('Ctrl Pts',(-20.12141715346,-52.5186495463858,-30.3702497885439));
#21497=CARTESIAN_POINT('Ctrl Pts',(-19.2932775165132,-52.5585718760047,
-30.3176002808131));
#21498=CARTESIAN_POINT('Ctrl Pts',(-18.4435242728756,-52.150146512268,-30.2649507730823));
#21499=CARTESIAN_POINT('Ctrl Pts',(-17.9573801335119,-51.4785268829787,
-30.2123012653515));
#21500=CARTESIAN_POINT('Ctrl Pts',(-17.6504617638204,-51.0545118944526,
-30.1790619443983));
#21501=CARTESIAN_POINT('Ctrl Pts',(-17.4884707620747,-50.5255928985278,
-30.1458226234451));
#21502=CARTESIAN_POINT('Ctrl Pts',(-17.4853853786729,-49.9984092958285,
-30.112583302492));
#21503=CARTESIAN_POINT('Ctrl Pts',(-17.4802499007281,-49.9981961378425,
-30.387416697508));
#21504=CARTESIAN_POINT('Ctrl Pts',(-17.4860408503046,-50.7117274452609,
-30.4326406678226));
#21505=CARTESIAN_POINT('Ctrl Pts',(-17.8042645925932,-51.4297790158306,
-30.4778646381373));
#21506=CARTESIAN_POINT('Ctrl Pts',(-18.3404527356926,-51.8984842757991,
-30.5230886084519));
#21507=CARTESIAN_POINT('Ctrl Pts',(-18.9646801440534,-52.4441484675212,
-30.5757381161827));
#21508=CARTESIAN_POINT('Ctrl Pts',(-19.8843254635857,-52.6518612967176,
-30.6283876239135));
#21509=CARTESIAN_POINT('Ctrl Pts',(-20.6824814735535,-52.4274593109222,
-30.6810371316444));
#21510=CARTESIAN_POINT('Ctrl Pts',(-21.4806374835213,-52.2030573251268,
-30.7336866393752));
#21511=CARTESIAN_POINT('Ctrl Pts',(-22.1573041839245,-51.5465405243398,
-30.786336147106));
#21512=CARTESIAN_POINT('Ctrl Pts',(-22.4057250160791,-50.7555308166698,
-30.8389856548368));
#21513=CARTESIAN_POINT('Ctrl Pts',(-22.6541458482338,-49.9645211089998,
-30.8916351625677));
#21514=CARTESIAN_POINT('Ctrl Pts',(-22.4743208121398,-49.0390184944469,
-30.9442846702985));
#21515=CARTESIAN_POINT('Ctrl Pts',(-21.9477708533448,-48.3985855093739,
-30.9969341780293));
#21516=CARTESIAN_POINT('Ctrl Pts',(-21.4212208945498,-47.7581525243009,
-31.0495836857601));
#21517=CARTESIAN_POINT('Ctrl Pts',(-20.5479460130537,-47.4027891687077,
-31.1022331934909));
#21518=CARTESIAN_POINT('Ctrl Pts',(-19.7238320966554,-47.4935940159087,
-31.1548827012218));
#21519=CARTESIAN_POINT('Ctrl Pts',(-18.8997181802571,-47.5843988631096,
-31.2075322089526));
#21520=CARTESIAN_POINT('Ctrl Pts',(-18.1247652289565,-48.1213719131045,
-31.2601817166834));
#21521=CARTESIAN_POINT('Ctrl Pts',(-17.7502863786615,-48.8610845993269,
-31.3128312244143));
#21522=CARTESIAN_POINT('Ctrl Pts',(-17.5734522959595,-49.2103871413211,
-31.3376930487788));
#21523=CARTESIAN_POINT('Ctrl Pts',(-17.4859182820506,-49.6048977589854,
-31.3625548731434));
#21524=CARTESIAN_POINT('Ctrl Pts',(-17.4864434588916,-49.999628681025,-31.387416697508));
#21525=CARTESIAN_POINT('Origin',(-20.,-50.,-32.));
#21526=CARTESIAN_POINT('',(-17.4815611182796,-50.0021533196962,-32.387416697508));
#21527=CARTESIAN_POINT('',(-17.4785348819534,-49.9995340142102,-32.112583302492));
#21528=CARTESIAN_POINT('',(-17.4825,-50.,-32.));
#21529=CARTESIAN_POINT('Ctrl Pts',(-17.4785348819534,-49.9995340142102,
-32.112583302492));
#21530=CARTESIAN_POINT('Ctrl Pts',(-17.4784687956751,-49.97381126057,-32.1109500495483));
#21531=CARTESIAN_POINT('Ctrl Pts',(-17.4788287321595,-49.9480904010419,
-32.1093167966047));
#21532=CARTESIAN_POINT('Ctrl Pts',(-17.4796204177225,-49.9223828375818,
-32.1076835436611));
#21533=CARTESIAN_POINT('Ctrl Pts',(-17.5051411769714,-49.093674359568,-32.0550340359302));
#21534=CARTESIAN_POINT('Ctrl Pts',(-17.9793175952482,-48.2787826016234,
-32.0023845281994));
#21535=CARTESIAN_POINT('Ctrl Pts',(-18.6871890040388,-47.847126350306,-31.9497350204686));
#21536=CARTESIAN_POINT('Ctrl Pts',(-19.3950604128295,-47.4154700989886,
-31.8970855127378));
#21537=CARTESIAN_POINT('Ctrl Pts',(-20.336626812134,-47.3670493542984,-31.844436005007));
#21538=CARTESIAN_POINT('Ctrl Pts',(-21.0850433930516,-47.7238149245155,
-31.7917864972761));
#21539=CARTESIAN_POINT('Ctrl Pts',(-21.8334599739691,-48.0805804947325,
-31.7391369895453));
#21540=CARTESIAN_POINT('Ctrl Pts',(-22.3887267364997,-48.8425323798569,
-31.6864874818145));
#21541=CARTESIAN_POINT('Ctrl Pts',(-22.4991219376876,-49.664251279627,-31.6338379740837));
#21542=CARTESIAN_POINT('Ctrl Pts',(-22.6095171388755,-50.4859701793971,
-31.5811884663529));
#21543=CARTESIAN_POINT('Ctrl Pts',(-22.2750407787207,-51.3674560938129,
-31.5285389586221));
#21544=CARTESIAN_POINT('Ctrl Pts',(-21.6473226287802,-51.909100788165,-31.4758894508912));
#21545=CARTESIAN_POINT('Ctrl Pts',(-21.0196044788396,-52.4507454825172,
-31.4232399431604));
#21546=CARTESIAN_POINT('Ctrl Pts',(-20.0986445391132,-52.6525489568057,
-31.3705904354295));
#21547=CARTESIAN_POINT('Ctrl Pts',(-19.3019459934108,-52.4230266747496,
-31.3179409276987));
#21548=CARTESIAN_POINT('Ctrl Pts',(-18.5052474477083,-52.1935043926934,
-31.2652914199679));
#21549=CARTESIAN_POINT('Ctrl Pts',(-17.8328102960298,-51.5326563542926,
-31.2126419122371));
#21550=CARTESIAN_POINT('Ctrl Pts',(-17.5894736954629,-50.7400679683638,
-31.1599924045063));
#21551=CARTESIAN_POINT('Ctrl Pts',(-17.5164349010069,-50.5021682850724,
-31.1441893705015));
#21552=CARTESIAN_POINT('Ctrl Pts',(-17.482055175614,-50.2523996839241,-31.1283863364968));
#21553=CARTESIAN_POINT('Ctrl Pts',(-17.4840572259774,-50.0020935757321,
-31.112583302492));
#21554=CARTESIAN_POINT('Ctrl Pts',(-17.4864434588916,-49.999628681025,-31.387416697508));
#21555=CARTESIAN_POINT('Ctrl Pts',(-17.4870304410677,-50.4408134354357,
-31.4152043808742));
#21556=CARTESIAN_POINT('Ctrl Pts',(-17.5976226663159,-50.8822733983299,
-31.4429920642405));
#21557=CARTESIAN_POINT('Ctrl Pts',(-17.8164875791883,-51.2611951379893,
-31.4707797476067));
#21558=CARTESIAN_POINT('Ctrl Pts',(-18.2311723792997,-51.9791406679796,
-31.5234292553375));
#21559=CARTESIAN_POINT('Ctrl Pts',(-19.0345467288119,-52.4725794055107,
-31.5760787630683));
#21560=CARTESIAN_POINT('Ctrl Pts',(-19.8624130831367,-52.5178184025531,
-31.6287282707992));
#21561=CARTESIAN_POINT('Ctrl Pts',(-20.6902794374616,-52.5630573995955,
-31.68137777853));
#21562=CARTESIAN_POINT('Ctrl Pts',(-21.5426377965991,-52.1600966561492,
-31.7340272862608));
#21563=CARTESIAN_POINT('Ctrl Pts',(-22.0330844600882,-51.4916122975072,
-31.7866767939917));
#21564=CARTESIAN_POINT('Ctrl Pts',(-22.5235311235772,-50.8231279388651,
-31.8393263017225));
#21565=CARTESIAN_POINT('Ctrl Pts',(-22.6520660914177,-49.8891199650273,
-31.8919758094533));
#21566=CARTESIAN_POINT('Ctrl Pts',(-22.3604199905464,-49.1130066876489,
-31.9446253171841));
#21567=CARTESIAN_POINT('Ctrl Pts',(-22.0687738896751,-48.3368934102704,
-31.9972748249149));
#21568=CARTESIAN_POINT('Ctrl Pts',(-21.3569467200919,-47.7186748293514,
-32.0499243326458));
#21569=CARTESIAN_POINT('Ctrl Pts',(-20.5476345045051,-47.5386109374172,
-32.1025738403766));
#21570=CARTESIAN_POINT('Ctrl Pts',(-19.7383222889183,-47.3585470454831,
-32.1552233481074));
#21571=CARTESIAN_POINT('Ctrl Pts',(-18.8315250273277,-47.6166378425338,
-32.2078728558382));
#21572=CARTESIAN_POINT('Ctrl Pts',(-18.2383254687796,-48.1958817904649,
-32.2605223635691));
#21573=CARTESIAN_POINT('Ctrl Pts',(-17.76175461295,-48.6612408421056,-32.302820474882));
#21574=CARTESIAN_POINT('Ctrl Pts',(-17.4875910678703,-49.3338837640615,
-32.345118586195));
#21575=CARTESIAN_POINT('Ctrl Pts',(-17.4815611182796,-50.0021533196962,
-32.387416697508));
#21576=CARTESIAN_POINT('Origin',(-20.,-50.,-32.));
#21577=CARTESIAN_POINT('',(-17.4801090985914,-49.9982532978734,-33.387416697508));
#21578=CARTESIAN_POINT('',(-17.485278158989,-49.9983487243454,-33.112583302492));
#21579=CARTESIAN_POINT('',(-17.4825,-50.,-32.));
#21580=CARTESIAN_POINT('Ctrl Pts',(-17.485278158989,-49.9983487243454,-33.112583302492));
#21581=CARTESIAN_POINT('Ctrl Pts',(-17.4834356301179,-49.6959336765475,
-33.0935137626));
#21582=CARTESIAN_POINT('Ctrl Pts',(-17.5339467999326,-49.3941133640789,
-33.0744442227079));
#21583=CARTESIAN_POINT('Ctrl Pts',(-17.6395803816627,-49.1130068275169,
-33.0553746828159));
#21584=CARTESIAN_POINT('Ctrl Pts',(-17.931226436545,-48.3368936725219,-33.0027251750851));
#21585=CARTESIAN_POINT('Ctrl Pts',(-18.6430534938817,-47.7186751890883,
-32.9500756673542));
#21586=CARTESIAN_POINT('Ctrl Pts',(-19.45236558185,-47.5386113255479,-32.8974261596234));
#21587=CARTESIAN_POINT('Ctrl Pts',(-20.2616776698183,-47.3585474620076,
-32.8447766518926));
#21588=CARTESIAN_POINT('Ctrl Pts',(-21.1684747884181,-47.6166382183606,
-32.7921271441618));
#21589=CARTESIAN_POINT('Ctrl Pts',(-21.761674253426,-48.1958820749521,-32.7394776364309));
#21590=CARTESIAN_POINT('Ctrl Pts',(-22.3548737184339,-48.7751259315435,
-32.6868281287001));
#21591=CARTESIAN_POINT('Ctrl Pts',(-22.63447552985,-49.6755228883735,-32.6341786209693));
#21592=CARTESIAN_POINT('Ctrl Pts',(-22.4737264583211,-50.4888916772308,
-32.5815291132385));
#21593=CARTESIAN_POINT('Ctrl Pts',(-22.3129773867922,-51.3022604660881,
-32.5288796055077));
#21594=CARTESIAN_POINT('Ctrl Pts',(-21.7118774323183,-52.0286010869729,
-32.4762300977768));
#21595=CARTESIAN_POINT('Ctrl Pts',(-20.9429261184457,-52.3386380647326,
-32.423580590046));
#21596=CARTESIAN_POINT('Ctrl Pts',(-20.1739748045732,-52.6486750424923,
-32.3709310823152));
#21597=CARTESIAN_POINT('Ctrl Pts',(-19.2371721313021,-52.5424083771271,
-32.3182815745844));
#21598=CARTESIAN_POINT('Ctrl Pts',(-18.5572033447772,-52.0680124454029,
-32.2656320668536));
#21599=CARTESIAN_POINT('Ctrl Pts',(-17.8983280322473,-51.6083328630869,
-32.2146158120664));
#21600=CARTESIAN_POINT('Ctrl Pts',(-17.4805991515588,-50.8030094089147,
-32.1635995572792));
#21601=CARTESIAN_POINT('Ctrl Pts',(-17.4785348819534,-49.9995340142102,
-32.112583302492));
#21602=CARTESIAN_POINT('Ctrl Pts',(-17.4815611182796,-50.0021533196962,
-32.387416697508));
#21603=CARTESIAN_POINT('Ctrl Pts',(-17.480085440131,-50.1656954465103,-32.3977680939259));
#21604=CARTESIAN_POINT('Ctrl Pts',(-17.4946683427963,-50.3289756514404,
-32.4081194903437));
#21605=CARTESIAN_POINT('Ctrl Pts',(-17.5262731516027,-50.4888917543231,
-32.4184708867615));
#21606=CARTESIAN_POINT('Ctrl Pts',(-17.6870222484798,-51.3022606714387,
-32.4711203944923));
#21607=CARTESIAN_POINT('Ctrl Pts',(-18.2881222977398,-52.0286014068583,
-32.5237699022232));
#21608=CARTESIAN_POINT('Ctrl Pts',(-19.0570737328665,-52.3386384335071,
-32.576419409954));
#21609=CARTESIAN_POINT('Ctrl Pts',(-19.8260251679932,-52.6486754601558,
-32.6290689176848));
#21610=CARTESIAN_POINT('Ctrl Pts',(-20.7628279889865,-52.5424087780336,
-32.6817184254156));
#21611=CARTESIAN_POINT('Ctrl Pts',(-21.4427968827342,-52.068012771503,-32.7343679331465));
#21612=CARTESIAN_POINT('Ctrl Pts',(-22.1227657764818,-51.5936167649724,
-32.7870174408773));
#21613=CARTESIAN_POINT('Ctrl Pts',(-22.5459007429837,-50.7510914340334,
-32.8396669486081));
#21614=CARTESIAN_POINT('Ctrl Pts',(-22.5203799797104,-49.9223828253425,
-32.8923164563389));
#21615=CARTESIAN_POINT('Ctrl Pts',(-22.4948592164371,-49.0936742166515,
-32.9449659640698));
#21616=CARTESIAN_POINT('Ctrl Pts',(-22.0206827233885,-48.2787823302085,
-32.9976154718006));
#21617=CARTESIAN_POINT('Ctrl Pts',(-21.3128112029753,-47.8471260108243,
-33.0502649795314));
#21618=CARTESIAN_POINT('Ctrl Pts',(-20.604939682562,-47.41546969144,-33.1029144872622));
#21619=CARTESIAN_POINT('Ctrl Pts',(-19.663373134784,-47.3670489391145,-33.155563994993));
#21620=CARTESIAN_POINT('Ctrl Pts',(-18.9149564358503,-47.7238145655892,
-33.2082135027239));
#21621=CARTESIAN_POINT('Ctrl Pts',(-18.1665397369167,-48.0805801920638,
-33.2608630104547));
#21622=CARTESIAN_POINT('Ctrl Pts',(-17.6112728868275,-48.8425321973387,
-33.3135125181855));
#21623=CARTESIAN_POINT('Ctrl Pts',(-17.5008776682317,-49.6642512266837,
-33.3661620259163));
#21624=CARTESIAN_POINT('Ctrl Pts',(-17.4860221059945,-49.7748275572271,
-33.3732469164469));
#21625=CARTESIAN_POINT('Ctrl Pts',(-17.4792224123127,-49.8864861669174,
-33.3803318069775));
#21626=CARTESIAN_POINT('Ctrl Pts',(-17.4801090985914,-49.9982532978734,
-33.387416697508));
#21627=CARTESIAN_POINT('Origin',(-20.,-50.,-32.));
#21628=CARTESIAN_POINT('',(-17.4864167202486,-49.9995432846338,-34.387416697508));
#21629=CARTESIAN_POINT('',(-17.4841987514942,-50.0020603003561,-34.112583302492));
#21630=CARTESIAN_POINT('',(-17.4825,-50.,-32.));
#21631=CARTESIAN_POINT('Ctrl Pts',(-17.4841987514942,-50.0020603003561,
-34.112583302492));
#21632=CARTESIAN_POINT('Ctrl Pts',(-17.4887312218023,-49.4237578373463,
-34.0760774756515));
#21633=CARTESIAN_POINT('Ctrl Pts',(-17.6871331895373,-48.8426456017127,
-34.0395716488111));
#21634=CARTESIAN_POINT('Ctrl Pts',(-18.0522294537946,-48.3985857618973,
-34.0030658219707));
#21635=CARTESIAN_POINT('Ctrl Pts',(-18.5787793295592,-47.7581528778126,
-33.9504163142399));
#21636=CARTESIAN_POINT('Ctrl Pts',(-19.4520540733505,-47.4027895782559,
-33.8977668065091));
#21637=CARTESIAN_POINT('Ctrl Pts',(-20.2761678597962,-47.493594411138,-33.8451172987782));
#21638=CARTESIAN_POINT('Ctrl Pts',(-21.1002816462419,-47.58439924402,-33.7924677910474));
#21639=CARTESIAN_POINT('Ctrl Pts',(-21.875234475342,-48.1213722093409,-33.7398182833166));
#21640=CARTESIAN_POINT('Ctrl Pts',(-22.2497132665864,-48.8610847789196,
-33.6871687755858));
#21641=CARTESIAN_POINT('Ctrl Pts',(-22.6241920578308,-49.6007973484984,
-33.6345192678549));
#21642=CARTESIAN_POINT('Ctrl Pts',(-22.5981968112194,-50.543249522335,-33.5818697601241));
#21643=CARTESIAN_POINT('Ctrl Pts',(-22.1835120764988,-51.2611949391142,
-33.5292202523933));
#21644=CARTESIAN_POINT('Ctrl Pts',(-21.7688273417781,-51.9791403558935,
-33.4765707446625));
#21645=CARTESIAN_POINT('Ctrl Pts',(-20.9654531189481,-52.4725790156154,
-33.4239212369317));
#21646=CARTESIAN_POINT('Ctrl Pts',(-20.1375868951676,-52.5178180055241,
-33.3712717292008));
#21647=CARTESIAN_POINT('Ctrl Pts',(-19.309720671387,-52.5630569954329,-33.31862222147));
#21648=CARTESIAN_POINT('Ctrl Pts',(-18.4573624466559,-52.1600963155286,
-33.2659727137392));
#21649=CARTESIAN_POINT('Ctrl Pts',(-17.9669158605042,-51.4916120622984,
-33.2133232060083));
#21650=CARTESIAN_POINT('Ctrl Pts',(-17.6541079863296,-51.0652513859749,
-33.1797432381696));
#21651=CARTESIAN_POINT('Ctrl Pts',(-17.4885227081802,-50.5308779639869,
-33.1461632703308));
#21652=CARTESIAN_POINT('Ctrl Pts',(-17.485278158989,-49.9983487243454,-33.112583302492));
#21653=CARTESIAN_POINT('Ctrl Pts',(-17.4801090985914,-49.9982532978734,
-33.387416697508));
#21654=CARTESIAN_POINT('Ctrl Pts',(-17.4858115890802,-50.7170543175381,
-33.4329813147083));
#21655=CARTESIAN_POINT('Ctrl Pts',(-17.8094290744944,-51.4403438659751,
-33.4785459319085));
#21656=CARTESIAN_POINT('Ctrl Pts',(-18.3526771114574,-51.9091010892068,
-33.5241105491088));
#21657=CARTESIAN_POINT('Ctrl Pts',(-18.9803953603814,-52.4507458689696,
-33.5767600568396));
#21658=CARTESIAN_POINT('Ctrl Pts',(-19.9013554453319,-52.65254937508,-33.6294095645704));
#21659=CARTESIAN_POINT('Ctrl Pts',(-20.6980541166638,-52.4230270568311,
-33.6820590723013));
#21660=CARTESIAN_POINT('Ctrl Pts',(-21.4947527879958,-52.1935047385821,
-33.7347085800321));
#21661=CARTESIAN_POINT('Ctrl Pts',(-22.1671900457094,-51.5326565959736,
-33.7873580877629));
#21662=CARTESIAN_POINT('Ctrl Pts',(-22.4105266846474,-50.7400680850634,
-33.8400075954937));
#21663=CARTESIAN_POINT('Ctrl Pts',(-22.6538633235855,-49.9474795741532,
-33.8926571032246));
#21664=CARTESIAN_POINT('Ctrl Pts',(-22.468099343748,-49.0231506949411,-33.9453066109554));
#21665=CARTESIAN_POINT('Ctrl Pts',(-21.9374480205163,-48.3861118887221,
-33.9979561186862));
#21666=CARTESIAN_POINT('Ctrl Pts',(-21.4067966972846,-47.749073082503,-34.050605626417));
#21667=CARTESIAN_POINT('Ctrl Pts',(-20.5312580306586,-47.3993243492769,
-34.1032551341478));
#21668=CARTESIAN_POINT('Ctrl Pts',(-19.7077441610009,-47.4954189586884,
-34.1559046418787));
#21669=CARTESIAN_POINT('Ctrl Pts',(-18.8842302913432,-47.5915135680998,
-34.2085541496095));
#21670=CARTESIAN_POINT('Ctrl Pts',(-18.1127412186538,-48.1334515201489,
-34.2612036573403));
#21671=CARTESIAN_POINT('Ctrl Pts',(-17.7430197821465,-48.8755534854229,
-34.3138531650712));
#21672=CARTESIAN_POINT('Ctrl Pts',(-17.5708243457006,-49.22118281383,-34.3383743425501));
#21673=CARTESIAN_POINT('Ctrl Pts',(-17.4857792242903,-49.610231161691,-34.3628955200291));
#21674=CARTESIAN_POINT('Ctrl Pts',(-17.4864167202486,-49.9995432846338,
-34.387416697508));
#21675=CARTESIAN_POINT('Origin',(-20.,-50.,-32.));
#21676=CARTESIAN_POINT('',(-17.4817210057717,-50.002176808168,-35.387416697508));
#21677=CARTESIAN_POINT('',(-17.478494824499,-49.9996299858999,-35.112583302492));
#21678=CARTESIAN_POINT('',(-17.4825,-50.,-32.));
#21679=CARTESIAN_POINT('Ctrl Pts',(-17.478494824499,-49.9996299858999,-35.112583302492));
#21680=CARTESIAN_POINT('Ctrl Pts',(-17.4784526521761,-49.9792730852633,
-35.111290696434));
#21681=CARTESIAN_POINT('Ctrl Pts',(-17.4786780841199,-49.9589171423125,
-35.109998090376));
#21682=CARTESIAN_POINT('Ctrl Pts',(-17.4791739952253,-49.9385677909044,
-35.108705484318));
#21683=CARTESIAN_POINT('Ctrl Pts',(-17.4993730925594,-49.1097125278149,
-35.0560559765871));
#21684=CARTESIAN_POINT('Ctrl Pts',(-17.9683073171013,-48.2917928826973,
-35.0034064688563));
#21685=CARTESIAN_POINT('Ctrl Pts',(-18.6733924691504,-47.8556002887155,
-34.9507569611255));
#21686=CARTESIAN_POINT('Ctrl Pts',(-19.3784776211995,-47.4194076947338,
-34.8981074533947));
#21687=CARTESIAN_POINT('Ctrl Pts',(-20.3197137007558,-47.3649421518879,
-34.8454579456639));
#21688=CARTESIAN_POINT('Ctrl Pts',(-21.0704056443528,-47.7168947857795,
-34.792808437933));
#21689=CARTESIAN_POINT('Ctrl Pts',(-21.8210975879499,-48.0688474196711,
-34.7401589302022));
#21690=CARTESIAN_POINT('Ctrl Pts',(-22.3812453955877,-48.8272182303001,
-34.6875094224714));
#21691=CARTESIAN_POINT('Ctrl Pts',(-22.4969145767365,-49.6482113430708,
-34.6348599147406));
#21692=CARTESIAN_POINT('Ctrl Pts',(-22.6125837578853,-50.4692044558415,
-34.5822104070098));
#21693=CARTESIAN_POINT('Ctrl Pts',(-22.2837743125452,-51.352819870754,-34.5295608992789));
#21694=CARTESIAN_POINT('Ctrl Pts',(-21.6595470026173,-51.8984839764315,
-34.4769113915481));
#21695=CARTESIAN_POINT('Ctrl Pts',(-21.0353196926895,-52.4441480821091,
-34.4242618838173));
#21696=CARTESIAN_POINT('Ctrl Pts',(-20.1156745181739,-52.6518608785517,
-34.3716123760864));
#21697=CARTESIAN_POINT('Ctrl Pts',(-19.3175186340655,-52.4274589281418,
-34.3189628683556));
#21698=CARTESIAN_POINT('Ctrl Pts',(-18.5193627499571,-52.2030569777319,
-34.2663133606248));
#21699=CARTESIAN_POINT('Ctrl Pts',(-17.8426961562558,-51.5465402804695,
-34.213663852894));
#21700=CARTESIAN_POINT('Ctrl Pts',(-17.5942753632741,-50.755530697532,-34.1610143451632));
#21701=CARTESIAN_POINT('Ctrl Pts',(-17.5181032169182,-50.5129869998117,
-34.1448706642728));
#21702=CARTESIAN_POINT('Ctrl Pts',(-17.482194393269,-50.2577983901072,-34.1287269833824));
#21703=CARTESIAN_POINT('Ctrl Pts',(-17.4841987514942,-50.0020603003561,
-34.112583302492));
#21704=CARTESIAN_POINT('Ctrl Pts',(-17.4864167202486,-49.9995432846338,
-34.387416697508));
#21705=CARTESIAN_POINT('Ctrl Pts',(-17.487147994139,-50.446124611105,-34.4155450277599));
#21706=CARTESIAN_POINT('Ctrl Pts',(-17.6006244490009,-50.8930530251216,
-34.4436733580117));
#21707=CARTESIAN_POINT('Ctrl Pts',(-17.8246307238694,-51.2751894684295,
-34.4718016882636));
#21708=CARTESIAN_POINT('Ctrl Pts',(-18.2439169024245,-51.9904575076633,
-34.5244511959944));
#21709=CARTESIAN_POINT('Ctrl Pts',(-19.0504430598599,-52.4787276076318,
-34.5771007037253));
#21710=CARTESIAN_POINT('Ctrl Pts',(-19.8785828273941,-52.5186499435459,
-34.6297502114561));
#21711=CARTESIAN_POINT('Ctrl Pts',(-20.7067225949284,-52.5585722794599,
-34.6823997191869));
#21712=CARTESIAN_POINT('Ctrl Pts',(-21.5564759725616,-52.1501468513196,
-34.7350492269177));
#21713=CARTESIAN_POINT('Ctrl Pts',(-22.0426201885842,-51.4785271161241,
-34.7876987346485));
#21714=CARTESIAN_POINT('Ctrl Pts',(-22.5287644046068,-50.8069073809286,
-34.8403482423794));
#21715=CARTESIAN_POINT('Ctrl Pts',(-22.6512994590187,-49.872093338678,-34.8929977501102));
#21716=CARTESIAN_POINT('Ctrl Pts',(-22.3546759482698,-49.097868719883,-34.945647257841));
#21717=CARTESIAN_POINT('Ctrl Pts',(-22.058052437521,-48.323644101088,-34.9982967655718));
#21718=CARTESIAN_POINT('Ctrl Pts',(-21.3422703616113,-47.7100089057485,
-35.0509462733027));
#21719=CARTESIAN_POINT('Ctrl Pts',(-20.5318186398909,-47.5351453182397,
-35.1035957810335));
#21720=CARTESIAN_POINT('Ctrl Pts',(-19.7213669181704,-47.3602817307308,
-35.1562452887643));
#21721=CARTESIAN_POINT('Ctrl Pts',(-18.8162455506391,-47.6241897510527,
-35.2088947964951));
#21722=CARTESIAN_POINT('Ctrl Pts',(-18.2267775452558,-48.2072306913854,
-35.261544304226));
#21723=CARTESIAN_POINT('Ctrl Pts',(-17.7570184927424,-48.6718678849328,
-35.3035017686533));
#21724=CARTESIAN_POINT('Ctrl Pts',(-17.4877252255933,-49.3391806685967,
-35.3454592330807));
#21725=CARTESIAN_POINT('Ctrl Pts',(-17.4817210057717,-50.002176808168,-35.387416697508));
#21726=CARTESIAN_POINT('Origin',(-20.,-50.,-32.));
#21727=CARTESIAN_POINT('',(-17.4799717713781,-49.9983136769593,-36.387416697508));
#21728=CARTESIAN_POINT('',(-17.4851667329155,-49.9982906274316,-36.112583302492));
#21729=CARTESIAN_POINT('',(-17.4825,-50.,-32.));
#21730=CARTESIAN_POINT('Ctrl Pts',(-17.4851667329155,-49.9982906274316,
-36.112583302492));
#21731=CARTESIAN_POINT('Ctrl Pts',(-17.4832880584752,-49.7013108562046,
-36.0938544094856));
#21732=CARTESIAN_POINT('Ctrl Pts',(-17.5319619332951,-49.4049268457409,
-36.0751255164792));
#21733=CARTESIAN_POINT('Ctrl Pts',(-17.6339336595649,-49.1281813633219,
-36.0563966234728));
#21734=CARTESIAN_POINT('Ctrl Pts',(-17.9205902809002,-48.3502115489225,
-36.003747115742));
#21735=CARTESIAN_POINT('Ctrl Pts',(-18.6284330841387,-47.7274351695357,
-35.9510976080112));
#21736=CARTESIAN_POINT('Ctrl Pts',(-19.436572298498,-47.5421784263544,-35.8984481002803));
#21737=CARTESIAN_POINT('Ctrl Pts',(-20.2447115128574,-47.3569216831732,
-35.8457985925495));
#21738=CARTESIAN_POINT('Ctrl Pts',(-21.1531471383375,-47.6091845761975,
-35.7931490848186));
#21739=CARTESIAN_POINT('Ctrl Pts',(-21.7500536985207,-48.1846075589684,
-35.7404995770878));
#21740=CARTESIAN_POINT('Ctrl Pts',(-22.346960258704,-48.7600305417393,-35.687850069357));
#21741=CARTESIAN_POINT('Ctrl Pts',(-22.6323377535904,-49.6586136142567,
-35.6352005616262));
#21742=CARTESIAN_POINT('Ctrl Pts',(-22.4768146355635,-50.4729978051899,
-35.5825510538954));
#21743=CARTESIAN_POINT('Ctrl Pts',(-22.3212915175367,-51.287381996123,-35.5299015461646));
#21744=CARTESIAN_POINT('Ctrl Pts',(-21.7248677865967,-52.0175673054719,
-35.4772520384337));
#21745=CARTESIAN_POINT('Ctrl Pts',(-20.9579230714571,-52.332535327029,-35.4246025307029));
#21746=CARTESIAN_POINT('Ctrl Pts',(-20.1909783563175,-52.6475033485861,
-35.3719530229721));
#21747=CARTESIAN_POINT('Ctrl Pts',(-19.2535126569782,-52.5472540823515,
-35.3193035152413));
#21748=CARTESIAN_POINT('Ctrl Pts',(-18.5705117923717,-52.0772340087034,
-35.2666540075105));
#21749=CARTESIAN_POINT('Ctrl Pts',(-17.9042793856912,-51.618753469246,-35.2152971058376));
#21750=CARTESIAN_POINT('Ctrl Pts',(-17.4801703851418,-50.8084358381416,
-35.1639402041648));
#21751=CARTESIAN_POINT('Ctrl Pts',(-17.478494824499,-49.9996299858999,-35.112583302492));
#21752=CARTESIAN_POINT('Ctrl Pts',(-17.4817210057717,-50.002176808168,-35.387416697508));
#21753=CARTESIAN_POINT('Ctrl Pts',(-17.4801909471942,-50.1711284722182,
-35.3981087408115));
#21754=CARTESIAN_POINT('Ctrl Pts',(-17.495758511786,-50.3397998194272,-35.4088007841149));
#21755=CARTESIAN_POINT('Ctrl Pts',(-17.5294633202138,-50.5047654720315,
-35.4194928274184));
#21756=CARTESIAN_POINT('Ctrl Pts',(-17.6954317437902,-51.3170854520013,
-35.4721423351492));
#21757=CARTESIAN_POINT('Ctrl Pts',(-18.3011832341783,-52.0395515515973,
-35.5247918428801));
#21758=CARTESIAN_POINT('Ctrl Pts',(-19.0721095647582,-52.3446447509478,
-35.5774413506109));
#21759=CARTESIAN_POINT('Ctrl Pts',(-19.8430358953381,-52.6497379502984,
-35.6300908583417));
#21760=CARTESIAN_POINT('Ctrl Pts',(-20.7791370661099,-52.5374582494034,
-35.6827403660725));
#21761=CARTESIAN_POINT('Ctrl Pts',(-21.4560458464227,-52.0587059433,-35.7353898738033));
#21762=CARTESIAN_POINT('Ctrl Pts',(-22.1329546267354,-51.5799536371965,
-35.7880393815342));
#21763=CARTESIAN_POINT('Ctrl Pts',(-22.5506710165893,-50.7347287258845,
-35.840688889265));
#21764=CARTESIAN_POINT('Ctrl Pts',(-22.5198296427718,-49.9062010696257,
-35.8933383969958));
#21765=CARTESIAN_POINT('Ctrl Pts',(-22.4889882689544,-49.077673413367,-35.9459879047267));
#21766=CARTESIAN_POINT('Ctrl Pts',(-22.0095891314657,-48.2658430121615,
-35.9986374124575));
#21767=CARTESIAN_POINT('Ctrl Pts',(-21.2989605391671,-47.8387408332513,
-36.0512869201883));
#21768=CARTESIAN_POINT('Ctrl Pts',(-20.5883319468686,-47.4116386543412,
-36.1039364279191));
#21769=CARTESIAN_POINT('Ctrl Pts',(-19.6464738997602,-47.3692646977264,
-36.1565859356499));
#21770=CARTESIAN_POINT('Ctrl Pts',(-18.9003634208124,-47.7308285518507,
-36.2092354433807));
#21771=CARTESIAN_POINT('Ctrl Pts',(-18.1542529418645,-48.092392405975,-36.2618849511116));
#21772=CARTESIAN_POINT('Ctrl Pts',(-17.6038900310774,-48.8578940708383,
-36.3145344588424));
#21773=CARTESIAN_POINT('Ctrl Pts',(-17.4987733448449,-49.6803050083411,
-36.3671839665732));
#21774=CARTESIAN_POINT('Ctrl Pts',(-17.4853082133811,-49.7856533767842,
-36.3739282102182));
#21775=CARTESIAN_POINT('Ctrl Pts',(-17.4791490558524,-49.8919355603607,
-36.3806724538631));
#21776=CARTESIAN_POINT('Ctrl Pts',(-17.4799717713781,-49.9983136769593,
-36.387416697508));
#21777=CARTESIAN_POINT('Origin',(-20.,-50.,-32.));
#21778=CARTESIAN_POINT('',(-17.4863844696326,-49.9994585735565,-37.387416697508));
#21779=CARTESIAN_POINT('',(-17.4843373872682,-50.0020238412825,-37.112583302492));
#21780=CARTESIAN_POINT('',(-17.4825,-50.,-32.));
#21781=CARTESIAN_POINT('Ctrl Pts',(-17.4843373872682,-50.0020238412825,
-37.112583302492));
#21782=CARTESIAN_POINT('Ctrl Pts',(-17.4887305158478,-49.429037789462,-37.0764181225372));
#21783=CARTESIAN_POINT('Ctrl Pts',(-17.6831296450892,-48.8533549285412,
-37.0402529425824));
#21784=CARTESIAN_POINT('Ctrl Pts',(-18.0419869290546,-48.4111254070499,
-37.0040877626276));
#21785=CARTESIAN_POINT('Ctrl Pts',(-18.5644137321291,-47.7673247501846,
-36.9514382548968));
#21786=CARTESIAN_POINT('Ctrl Pts',(-19.4353886851995,-47.4063614792004,
-36.898788747166));
#21787=CARTESIAN_POINT('Ctrl Pts',(-20.2600685400885,-47.4918728064946,
-36.8461392394351));
#21788=CARTESIAN_POINT('Ctrl Pts',(-21.0847483949774,-47.5773841337888,
-36.7934897317043));
#21789=CARTESIAN_POINT('Ctrl Pts',(-21.8631331516847,-48.1093700593613,
-36.7408402239735));
#21790=CARTESIAN_POINT('Ctrl Pts',(-22.2423539164814,-48.8466628523593,
-36.6881907162427));
#21791=CARTESIAN_POINT('Ctrl Pts',(-22.6215746812781,-49.5839556453572,
-36.6355412085118));
#21792=CARTESIAN_POINT('Ctrl Pts',(-22.6016314541642,-50.5265553057806,
-36.582891700781));
#21793=CARTESIAN_POINT('Ctrl Pts',(-22.1915651943947,-51.2471486121684,
-36.5302421930502));
#21794=CARTESIAN_POINT('Ctrl Pts',(-21.7814989346252,-51.9677419185562,
-36.4775926853194));
#21795=CARTESIAN_POINT('Ctrl Pts',(-20.9813096422002,-52.4663288709085,
-36.4249431775885));
#21796=CARTESIAN_POINT('Ctrl Pts',(-20.1537509642527,-52.5168826559653,
-36.3722936698577));
#21797=CARTESIAN_POINT('Ctrl Pts',(-19.3261922863052,-52.5674364410221,
-36.3196441621269));
#21798=CARTESIAN_POINT('Ctrl Pts',(-18.4712642228353,-52.1699570587834,
-36.2669946543961));
#21799=CARTESIAN_POINT('Ctrl Pts',(-17.9765354108164,-51.5046357429582,
-36.2143451466653));
#21800=CARTESIAN_POINT('Ctrl Pts',(-17.6577953855276,-51.0759877081572,
-36.1804245319408));
#21801=CARTESIAN_POINT('Ctrl Pts',(-17.4885692720755,-50.5361620540716,
-36.1465039172164));
#21802=CARTESIAN_POINT('Ctrl Pts',(-17.4851667329155,-49.9982906274316,
-36.112583302492));
#21803=CARTESIAN_POINT('Ctrl Pts',(-17.4799717713781,-49.9983136769593,
-36.387416697508));
#21804=CARTESIAN_POINT('Ctrl Pts',(-17.4855716541017,-50.7223853138266,
-36.4333219615939));
#21805=CARTESIAN_POINT('Ctrl Pts',(-17.8146388682811,-51.4509014884862,
-36.4792272256798));
#21806=CARTESIAN_POINT('Ctrl Pts',(-18.364969405791,-51.9196391915133,-36.5251324897657));
#21807=CARTESIAN_POINT('Ctrl Pts',(-18.9961526146475,-52.4572422270403,
-36.5777819974965));
#21808=CARTESIAN_POINT('Ctrl Pts',(-19.9183894940382,-52.6531280879523,
-36.6304315052273));
#21809=CARTESIAN_POINT('Ctrl Pts',(-20.7135979791903,-52.4184949012781,
-36.6830810129582));
#21810=CARTESIAN_POINT('Ctrl Pts',(-21.5088064643423,-52.1838617146039,
-36.735730520689));
#21811=CARTESIAN_POINT('Ctrl Pts',(-22.1769865552557,-51.5187094803435,
-36.7883800284198));
#21812=CARTESIAN_POINT('Ctrl Pts',(-22.4152289681752,-50.724574842535,-36.8410295361506));
#21813=CARTESIAN_POINT('Ctrl Pts',(-22.6534713810948,-49.9304402047265,
-36.8936790438815));
#21814=CARTESIAN_POINT('Ctrl Pts',(-22.4617761160207,-49.0073231633699,
-36.9463285516123));
#21815=CARTESIAN_POINT('Ctrl Pts',(-21.9270453071541,-48.3737048044754,
-36.9989780593431));
#21816=CARTESIAN_POINT('Ctrl Pts',(-21.3923144982876,-47.7400864455809,
-37.0516275670739));
#21817=CARTESIAN_POINT('Ctrl Pts',(-20.5145481456286,-47.3959667691485,
-37.1042770748047));
#21818=CARTESIAN_POINT('Ctrl Pts',(-19.6916682754265,-47.4973471716827,
-37.1569265825355));
#21819=CARTESIAN_POINT('Ctrl Pts',(-18.8687884052244,-47.598727574217,-37.2095760902664));
#21820=CARTESIAN_POINT('Ctrl Pts',(-18.1007950174792,-48.1456080557178,
-37.2622255979972));
#21821=CARTESIAN_POINT('Ctrl Pts',(-17.7358462391789,-48.8900687176614,
-37.314875105728));
#21822=CARTESIAN_POINT('Ctrl Pts',(-17.5682348885884,-49.2319798691139,
-37.3390556363214));
#21823=CARTESIAN_POINT('Ctrl Pts',(-17.4856386516788,-49.6155670561907,
-37.3632361669147));
#21824=CARTESIAN_POINT('Ctrl Pts',(-17.4863844696326,-49.9994585735565,
-37.387416697508));
#21825=CARTESIAN_POINT('Origin',(-20.,-50.,-32.));
#21826=CARTESIAN_POINT('',(-17.4818816223345,-50.0021988885187,-38.387416697508));
#21827=CARTESIAN_POINT('',(-17.4784634893366,-49.9997267145485,-38.112583302492));
#21828=CARTESIAN_POINT('',(-17.4825,-50.,-32.));
#21829=CARTESIAN_POINT('Ctrl Pts',(-17.4784634893366,-49.9997267145485,
-38.112583302492));
#21830=CARTESIAN_POINT('Ctrl Pts',(-17.4784401902979,-49.9847350675764,
-38.1116313433196));
#21831=CARTESIAN_POINT('Ctrl Pts',(-17.478562451161,-49.9697438107687,-38.1106793841472));
#21832=CARTESIAN_POINT('Ctrl Pts',(-17.4788314347168,-49.9547551871231,
-38.1097274249749));
#21833=CARTESIAN_POINT('Ctrl Pts',(-17.493707967459,-49.1257872235762,-38.057077917244));
#21834=CARTESIAN_POINT('Ctrl Pts',(-17.9573808053747,-48.3048735931184,
-38.0044284095132));
#21835=CARTESIAN_POINT('Ctrl Pts',(-18.659650665377,-47.8641626851468,-37.9517789017824));
#21836=CARTESIAN_POINT('Ctrl Pts',(-19.3619205253793,-47.4234517771752,
-37.8991293940516));
#21837=CARTESIAN_POINT('Ctrl Pts',(-20.3027874074683,-47.3629435916899,
-37.8464798863208));
#21838=CARTESIAN_POINT('Ctrl Pts',(-21.055723745345,-47.7100687559622,-37.7938303785899));
#21839=CARTESIAN_POINT('Ctrl Pts',(-21.8086600832218,-48.0571939202345,
-37.7411808708591));
#21840=CARTESIAN_POINT('Ctrl Pts',(-22.3736658768864,-48.8119524342645,
-37.6885313631283));
#21841=CARTESIAN_POINT('Ctrl Pts',(-22.4946042778578,-49.6321859220406,
-37.6358818553975));
#21842=CARTESIAN_POINT('Ctrl Pts',(-22.6155426788291,-50.4524194098166,
-37.5832323476666));
#21843=CARTESIAN_POINT('Ctrl Pts',(-22.2924136871073,-51.3381278713388,
-37.5305828399358));
#21844=CARTESIAN_POINT('Ctrl Pts',(-21.6717029494111,-51.8877888851473,
-37.477933332205));
#21845=CARTESIAN_POINT('Ctrl Pts',(-21.0509922117148,-52.4374498989559,
-37.4252838244742));
#21846=CARTESIAN_POINT('Ctrl Pts',(-20.132699728044,-52.6510634650507,-37.3726343167434));
#21847=CARTESIAN_POINT('Ctrl Pts',(-19.3331194154503,-52.4317911011418,
-37.3199848090125));
#21848=CARTESIAN_POINT('Ctrl Pts',(-18.5335391028565,-52.212518737233,-37.2673353012817));
#21849=CARTESIAN_POINT('Ctrl Pts',(-17.8526709613398,-51.5603604433206,
-37.2146857935509));
#21850=CARTESIAN_POINT('Ctrl Pts',(-17.5991762171207,-50.7709622749911,
-37.1620362858201));
#21851=CARTESIAN_POINT('Ctrl Pts',(-17.5198081349998,-50.5238052033796,
-37.145551958044));
#21852=CARTESIAN_POINT('Ctrl Pts',(-17.4823349702594,-50.2631946663995,
-37.129067630268));
#21853=CARTESIAN_POINT('Ctrl Pts',(-17.4843373872682,-50.0020238412825,
-37.112583302492));
#21854=CARTESIAN_POINT('Ctrl Pts',(-17.4863844696326,-49.9994585735565,
-37.387416697508));
#21855=CARTESIAN_POINT('Ctrl Pts',(-17.4872625593087,-50.4514337189728,
-37.4158856746455));
#21856=CARTESIAN_POINT('Ctrl Pts',(-17.6036657291937,-50.9038307136114,
-37.444354651783));
#21857=CARTESIAN_POINT('Ctrl Pts',(-17.8328635601392,-51.2891312519096,
-37.4728236289205));
#21858=CARTESIAN_POINT('Ctrl Pts',(-18.2567338282551,-52.001692281828,-37.5254731366513));
#21859=CARTESIAN_POINT('Ctrl Pts',(-19.0663785333421,-52.4847734992787,
-37.5781226443822));
#21860=CARTESIAN_POINT('Ctrl Pts',(-19.8947575738855,-52.5193775844509,
-37.630772152113));
#21861=CARTESIAN_POINT('Ctrl Pts',(-20.7231366144289,-52.5539816696232,
-37.6834216598438));
#21862=CARTESIAN_POINT('Ctrl Pts',(-21.5702499904287,-52.1401086225171,
-37.7360711675746));
#21863=CARTESIAN_POINT('Ctrl Pts',(-22.0520717080468,-51.4653810891725,
-37.7887206753054));
#21864=CARTESIAN_POINT('Ctrl Pts',(-22.5338934256649,-50.7906535558279,
-37.8413701830363));
#21865=CARTESIAN_POINT('Ctrl Pts',(-22.6504234849012,-49.8550715362449,
-37.8940196907671));
#21866=CARTESIAN_POINT('Ctrl Pts',(-22.3488348086601,-49.0827677205198,
-37.9466691984979));
#21867=CARTESIAN_POINT('Ctrl Pts',(-22.047246132419,-48.3104639047946,-37.9993187062287));
#21868=CARTESIAN_POINT('Ctrl Pts',(-21.3275387207004,-47.7014382929273,
-38.0519682139596));
#21869=CARTESIAN_POINT('Ctrl Pts',(-20.5159808782079,-47.5317817744353,
-38.1046177216904));
#21870=CARTESIAN_POINT('Ctrl Pts',(-19.7044230357155,-47.3621252559433,
-38.1572672294212));
#21871=CARTESIAN_POINT('Ctrl Pts',(-18.801014762449,-47.6318378308265,-38.209916737152));
#21872=CARTESIAN_POINT('Ctrl Pts',(-18.2153026720781,-48.2186526109762,
-38.2625662448829));
#21873=CARTESIAN_POINT('Ctrl Pts',(-17.7523263927637,-48.6825005117228,
-38.3041830624246));
#21874=CARTESIAN_POINT('Ctrl Pts',(-17.4878503825531,-49.3444775574439,
-38.3457998799663));
#21875=CARTESIAN_POINT('Ctrl Pts',(-17.4818816223345,-50.0021988885187,
-38.387416697508));
#21876=CARTESIAN_POINT('Origin',(-20.,-50.,-32.));
#21877=CARTESIAN_POINT('',(-17.4798421274757,-49.9984351524252,-39.387416697508));
#21878=CARTESIAN_POINT('',(-17.4850545138796,-49.9982392692185,-39.112583302492));
#21879=CARTESIAN_POINT('',(-17.4825,-50.,-32.));
#21880=CARTESIAN_POINT('',(-21.913465996665,-48.364012796625,-40.));
#21881=CARTESIAN_POINT('Ctrl Pts',(-17.4798421274757,-49.9984351524252,
-39.387416697508));
#21882=CARTESIAN_POINT('Ctrl Pts',(-17.4853147276126,-50.7276238536423,
-39.4336626084795));
#21883=CARTESIAN_POINT('Ctrl Pts',(-17.8198670584883,-51.4610375097699,
-39.4799085194511));
#21884=CARTESIAN_POINT('Ctrl Pts',(-18.3773138107771,-51.9298785803434,
-39.5261544304226));
#21885=CARTESIAN_POINT('Ctrl Pts',(-19.0119493164378,-52.4636393183443,
-39.5788039381534));
#21886=CARTESIAN_POINT('Ctrl Pts',(-19.9354805710936,-52.6544848107208,
-39.6314534458842));
#21887=CARTESIAN_POINT('Ctrl Pts',(-20.7291492614058,-52.4142811819356,
-39.6841029536151));
#21888=CARTESIAN_POINT('Ctrl Pts',(-21.522817951718,-52.1740775531505,-39.7367524613459));
#21889=CARTESIAN_POINT('Ctrl Pts',(-22.1866240776865,-51.5028248032037,
-39.7894019690767));
#21890=CARTESIAN_POINT('Ctrl Pts',(-22.4195849355037,-50.7085554156277,
-39.8420514768075));
#21891=CARTESIAN_POINT('Ctrl Pts',(-22.6525457933209,-49.9142860280518,
-39.8947009845383));
#21892=CARTESIAN_POINT('Ctrl Pts',(-22.4546613829867,-48.9970000028465,
-39.9473504922692));
#21893=CARTESIAN_POINT('Ctrl Pts',(-21.913465996665,-48.364012796625,-40.));
#21894=CARTESIAN_POINT('',(-18.0829275241642,-48.361458825814,-40.));
#21895=CARTESIAN_POINT('Origin',(-20.,-50.,-40.));
#21896=CARTESIAN_POINT('Ctrl Pts',(-18.0829200279321,-48.3614535172687,
-40.));
#21897=CARTESIAN_POINT('Ctrl Pts',(-18.6057519481588,-47.7526827191803,
-39.9490537266973));
#21898=CARTESIAN_POINT('Ctrl Pts',(-19.4454475058209,-47.4126382937553,
-39.8981074533947));
#21899=CARTESIAN_POINT('Ctrl Pts',(-20.2440955071633,-47.4904273239402,
-39.847161180092));
#21900=CARTESIAN_POINT('Ctrl Pts',(-21.0694438868393,-47.5708169948738,
-39.7945116723612));
#21901=CARTESIAN_POINT('Ctrl Pts',(-21.8509542298921,-48.0974451260636,
-39.7418621646304));
#21902=CARTESIAN_POINT('Ctrl Pts',(-22.2348330746457,-48.8322008546483,
-39.6892126568995));
#21903=CARTESIAN_POINT('Ctrl Pts',(-22.6187119193993,-49.566956583233,-39.6365631491687));
#21904=CARTESIAN_POINT('Ctrl Pts',(-22.6049592658536,-50.5098399092124,
-39.5839136414379));
#21905=CARTESIAN_POINT('Ctrl Pts',(-22.199562657414,-51.2330949537652,-39.5312641337071));
#21906=CARTESIAN_POINT('Ctrl Pts',(-21.7941660489743,-51.9563499983181,
-39.4786146259763));
#21907=CARTESIAN_POINT('Ctrl Pts',(-20.9971254856407,-52.4599767614444,
-39.4259651182454));
#21908=CARTESIAN_POINT('Ctrl Pts',(-20.1698912582501,-52.515821381016,-39.3733156105146));
#21909=CARTESIAN_POINT('Ctrl Pts',(-19.3426570308596,-52.5716660005875,
-39.3206661027838));
#21910=CARTESIAN_POINT('Ctrl Pts',(-18.485229139412,-52.1797284766043,-39.268016595053));
#21911=CARTESIAN_POINT('Ctrl Pts',(-17.9862471478564,-51.517608519283,-39.2153670873222));
#21912=CARTESIAN_POINT('Ctrl Pts',(-17.661538460383,-51.0867390571978,-39.1811058257121));
#21913=CARTESIAN_POINT('Ctrl Pts',(-17.488619258549,-50.5414566457736,-39.146844564102));
#21914=CARTESIAN_POINT('Ctrl Pts',(-17.4850545138796,-49.9982392692185,
-39.112583302492));
#21915=CARTESIAN_POINT('Origin',(-20.,-50.,-42.2084234471774));
#21916=CARTESIAN_POINT('',(-16.9217888153016,-49.9991816123293,-25.7915765528225));
#21917=CARTESIAN_POINT('',(-16.9314304880168,-49.9996668086012,-25.7084234471775));
#21918=CARTESIAN_POINT('',(-16.9265,-49.9999999999998,-42.2084234471774));
#21919=CARTESIAN_POINT('',(-20.7937992825329,-52.9692229537457,-25.));
#21920=CARTESIAN_POINT('Ctrl Pts',(-16.9314304880168,-49.9996668086012,
-25.7084234471775));
#21921=CARTESIAN_POINT('Ctrl Pts',(-16.9311124941626,-49.5044898991504,
-25.6828803290416));
#21922=CARTESIAN_POINT('Ctrl Pts',(-17.2773642933051,-47.9891814869228,
-25.6046877031749));
#21923=CARTESIAN_POINT('Ctrl Pts',(-19.6484750587118,-46.3913836024568,
-25.4738455695774));
#21924=CARTESIAN_POINT('Ctrl Pts',(-22.8319253439964,-47.7313330083366,
-25.3158970463849));
#21925=CARTESIAN_POINT('Ctrl Pts',(-23.4429084618352,-51.1345418770559,
-25.1579485231925));
#21926=CARTESIAN_POINT('Ctrl Pts',(-21.7760378723045,-52.706628901368,-25.0526495077308));
#21927=CARTESIAN_POINT('Ctrl Pts',(-20.7937992825329,-52.9692229537457,
-25.));
#21928=CARTESIAN_POINT('',(-19.2062007174672,-52.9692229537457,-25.));
#21929=CARTESIAN_POINT('Origin',(-20.,-50.,-25.));
#21930=CARTESIAN_POINT('Ctrl Pts',(-16.9217888153016,-49.9991816123293,
-25.7915765528225));
#21931=CARTESIAN_POINT('Ctrl Pts',(-16.9216327964757,-49.9546737426535,
-25.7892620061076));
#21932=CARTESIAN_POINT('Ctrl Pts',(-16.942593390011,-48.897887811184,-25.7342979516619));
#21933=CARTESIAN_POINT('Ctrl Pts',(-18.1518496079148,-46.8799270552508,
-25.6266843894854));
#21934=CARTESIAN_POINT('Ctrl Pts',(-21.6024144605454,-46.7464740570925,
-25.468735866293));
#21935=CARTESIAN_POINT('Ctrl Pts',(-23.6000558022285,-49.5638703006617,
-25.3107873431004));
#21936=CARTESIAN_POINT('Ctrl Pts',(-22.3474160567079,-52.7401230784006,
-25.1545420543362));
#21937=CARTESIAN_POINT('Ctrl Pts',(-20.1513508010164,-53.2252259242231,
-25.0509462733027));
#21938=CARTESIAN_POINT('Ctrl Pts',(-19.2043345174297,-52.9742970828256,
-25.));
#21939=CARTESIAN_POINT('Origin',(-20.,-50.,-42.2084234471774));
#21940=CARTESIAN_POINT('',(-16.9301482556011,-49.9981345312788,-26.7915765528225));
#21941=CARTESIAN_POINT('',(-16.9249665978426,-50.0025583315037,-26.7084234471774));
#21942=CARTESIAN_POINT('',(-16.9265,-49.9999999999998,-42.2084234471774));
#21943=CARTESIAN_POINT('Ctrl Pts',(-16.9249665978426,-50.0025583315037,
-26.7084234471774));
#21944=CARTESIAN_POINT('Ctrl Pts',(-16.9323545095395,-49.1738259014586,
-26.6654440420932));
#21945=CARTESIAN_POINT('Ctrl Pts',(-17.703989360689,-47.3177697473349,-26.5698151292781));
#21946=CARTESIAN_POINT('Ctrl Pts',(-20.8329798277681,-46.4704999500574,
-26.4215367087322));
#21947=CARTESIAN_POINT('Ctrl Pts',(-23.4108310490853,-48.7680163172086,
-26.2635881855398));
#21948=CARTESIAN_POINT('Ctrl Pts',(-22.8961088969807,-52.1826319253429,
-26.1056396623473));
#21949=CARTESIAN_POINT('Ctrl Pts',(-19.7557254019559,-53.6181282017024,
-25.9476911391548));
#21950=CARTESIAN_POINT('Ctrl Pts',(-17.3086034982695,-52.0718620980463,
-25.8152857340982));
#21951=CARTESIAN_POINT('Ctrl Pts',(-16.931767943501,-50.5251491774573,-25.7355298367724));
#21952=CARTESIAN_POINT('Ctrl Pts',(-16.9314304880168,-49.9996668086012,
-25.7084234471775));
#21953=CARTESIAN_POINT('Ctrl Pts',(-16.9301482556011,-49.9981345312788,
-26.7915765528225));
#21954=CARTESIAN_POINT('Ctrl Pts',(-16.9280041631807,-49.6156590014734,
-26.7718257191592));
#21955=CARTESIAN_POINT('Ctrl Pts',(-17.1709938395466,-48.2162502496147,
-26.6994253777651));
#21956=CARTESIAN_POINT('Ctrl Pts',(-19.2579268207016,-46.4502608973225,
-26.5743755286402));
#21957=CARTESIAN_POINT('Ctrl Pts',(-22.5667151646459,-47.4380997591695,
-26.4164270054477));
#21958=CARTESIAN_POINT('Ctrl Pts',(-23.5483399170972,-50.748751349135,-26.2584784822553));
#21959=CARTESIAN_POINT('Ctrl Pts',(-21.312794804531,-53.3805016203859,-26.1005299590628));
#21960=CARTESIAN_POINT('Ctrl Pts',(-17.9371758478695,-52.9536638884015,
-25.9448959825852));
#21961=CARTESIAN_POINT('Ctrl Pts',(-16.9251817913301,-50.9671041306423,
-25.8419115138385));
#21962=CARTESIAN_POINT('Ctrl Pts',(-16.9217888153016,-49.9991816123293,
-25.7915765528225));
#21963=CARTESIAN_POINT('Origin',(-20.,-50.,-42.2084234471774));
#21964=CARTESIAN_POINT('',(-16.928225056676,-50.0025926095194,-27.7915765528225));
#21965=CARTESIAN_POINT('',(-16.9239287305948,-49.9977320013947,-27.7084234471775));
#21966=CARTESIAN_POINT('',(-16.9265,-49.9999999999998,-42.2084234471774));
#21967=CARTESIAN_POINT('Ctrl Pts',(-16.9239287305948,-49.9977320013947,
-27.7084234471775));
#21968=CARTESIAN_POINT('Ctrl Pts',(-16.9226896332749,-49.8481151515914,
-27.7006572628756));
#21969=CARTESIAN_POINT('Ctrl Pts',(-17.0003510257386,-48.6854876981218,
-27.640241570843));
#21970=CARTESIAN_POINT('Ctrl Pts',(-18.4816794190144,-46.7066668978831,
-27.5271763710795));
#21971=CARTESIAN_POINT('Ctrl Pts',(-21.9276633145204,-46.9282819155376,
-27.369227847887));
#21972=CARTESIAN_POINT('Ctrl Pts',(-23.6258941273587,-49.9349295156179,
-27.2112793246946));
#21973=CARTESIAN_POINT('Ctrl Pts',(-22.0366357822403,-53.0005761032442,
-27.0533308015021));
#21974=CARTESIAN_POINT('Ctrl Pts',(-18.6008241624394,-53.3456884935447,
-26.8953822783096));
#21975=CARTESIAN_POINT('Ctrl Pts',(-17.0233222448715,-51.3888911243564,
-26.7804131602014));
#21976=CARTESIAN_POINT('Ctrl Pts',(-16.9233043630045,-50.1890180474854,
-26.718093549824));
#21977=CARTESIAN_POINT('Ctrl Pts',(-16.9249665978426,-50.0025583315037,
-26.7084234471774));
#21978=CARTESIAN_POINT('Ctrl Pts',(-16.928225056676,-50.0025926095194,-27.7915765528225));
#21979=CARTESIAN_POINT('Ctrl Pts',(-16.9340843879266,-49.2836004587027,
-27.7543894322109));
#21980=CARTESIAN_POINT('Ctrl Pts',(-17.5432834505634,-47.5377126858431,
-27.6645528038683));
#21981=CARTESIAN_POINT('Ctrl Pts',(-20.4434363389617,-46.4007362339102,
-27.522066667795));
#21982=CARTESIAN_POINT('Ctrl Pts',(-23.2562593438794,-48.403719623335,-27.3641181446025));
#21983=CARTESIAN_POINT('Ctrl Pts',(-23.1167310200335,-51.8540021340239,
-27.2061696214101));
#21984=CARTESIAN_POINT('Ctrl Pts',(-20.1513575038949,-53.623316794304,-27.0482210982176));
#21985=CARTESIAN_POINT('Ctrl Pts',(-17.4367210524572,-52.2970305039663,
-26.9100234086884));
#21986=CARTESIAN_POINT('Ctrl Pts',(-16.9337196389114,-50.635218413832,-26.8244752268901));
#21987=CARTESIAN_POINT('Ctrl Pts',(-16.9301482556011,-49.9981345312788,
-26.7915765528225));
#21988=CARTESIAN_POINT('Origin',(-20.,-50.,-42.2084234471774));
#21989=CARTESIAN_POINT('',(-16.9217184048747,-49.9993152064879,-28.7915765528225));
#21990=CARTESIAN_POINT('',(-16.9313402641813,-49.9996515904955,-28.7084234471775));
#21991=CARTESIAN_POINT('',(-16.9265,-49.9999999999998,-42.2084234471774));
#21992=CARTESIAN_POINT('Ctrl Pts',(-16.9313402641813,-49.9996515904955,
-28.7084234471775));
#21993=CARTESIAN_POINT('Ctrl Pts',(-16.9308409783865,-49.5111295368377,
-28.6832209759272));
#21994=CARTESIAN_POINT('Ctrl Pts',(-17.2704954611012,-48.0027107711033,
-28.6053689969462));
#21995=CARTESIAN_POINT('Ctrl Pts',(-19.6259746610823,-46.3928619507583,
-28.4748675102343));
#21996=CARTESIAN_POINT('Ctrl Pts',(-22.8159749872838,-47.7149125425452,
-28.3169189870419));
#21997=CARTESIAN_POINT('Ctrl Pts',(-23.4528164464309,-51.1087824216521,
-28.1589704638493));
#21998=CARTESIAN_POINT('Ctrl Pts',(-20.9590942265365,-53.4973530261498,
-28.0010219406569));
#21999=CARTESIAN_POINT('Ctrl Pts',(-17.7611610467444,-52.7534485267535,
-27.8508396017662));
#22000=CARTESIAN_POINT('Ctrl Pts',(-16.9310898799582,-50.8624167937153,
-27.7533067706064));
#22001=CARTESIAN_POINT('Ctrl Pts',(-16.9239287305948,-49.9977320013947,
-27.7084234471775));
#22002=CARTESIAN_POINT('Ctrl Pts',(-16.9217184048747,-49.9993152064879,
-28.7915765528225));
#22003=CARTESIAN_POINT('Ctrl Pts',(-16.9216027631545,-49.9613596580176,
-28.7896026529933));
#22004=CARTESIAN_POINT('Ctrl Pts',(-16.9393663574583,-48.9111326917697,
-28.7349792454332));
#22005=CARTESIAN_POINT('Ctrl Pts',(-18.1318616862451,-46.8917215466485,
-28.6277063301423));
#22006=CARTESIAN_POINT('Ctrl Pts',(-21.5814746967481,-46.7365243250642,
-28.4697578069498));
#22007=CARTESIAN_POINT('Ctrl Pts',(-23.5972126982202,-49.5402212417787,
-28.3118092837573));
#22008=CARTESIAN_POINT('Ctrl Pts',(-22.3514673502323,-52.7607855790929,
-28.1538607605649));
#22009=CARTESIAN_POINT('Ctrl Pts',(-18.9737180729577,-53.4782295892619,
-27.9959122373724));
#22010=CARTESIAN_POINT('Ctrl Pts',(-17.1026437687264,-51.6156340543063,
-27.8751508347916));
#22011=CARTESIAN_POINT('Ctrl Pts',(-16.9257887495201,-50.3015492049395,
-27.8070389399417));
#22012=CARTESIAN_POINT('Ctrl Pts',(-16.928225056676,-50.0025926095194,-27.7915765528225));
#22013=CARTESIAN_POINT('Origin',(-20.,-50.,-42.2084234471774));
#22014=CARTESIAN_POINT('',(-16.9300226261573,-49.9980579824143,-29.7915765528225));
#22015=CARTESIAN_POINT('',(-16.9251595829395,-50.0025957433342,-29.7084234471775));
#22016=CARTESIAN_POINT('',(-16.9265,-49.9999999999998,-42.2084234471774));
#22017=CARTESIAN_POINT('Ctrl Pts',(-16.9251595829395,-50.0025957433342,
-29.7084234471775));
#22018=CARTESIAN_POINT('Ctrl Pts',(-16.9325403191697,-49.1802996882788,
-29.6657846889788));
#22019=CARTESIAN_POINT('Ctrl Pts',(-17.6939854946978,-47.3305806954569,
-29.5704964230493));
#22020=CARTESIAN_POINT('Ctrl Pts',(-20.810310380068,-46.4652104819412,-29.4225586493892));
#22021=CARTESIAN_POINT('Ctrl Pts',(-23.4028289883847,-48.7461679840765,
-29.2646101261966));
#22022=CARTESIAN_POINT('Ctrl Pts',(-22.9101060454574,-52.163936841271,-29.1066616030042));
#22023=CARTESIAN_POINT('Ctrl Pts',(-19.7788784576719,-53.6197299780505,
-28.9487130798117));
#22024=CARTESIAN_POINT('Ctrl Pts',(-17.3157682680493,-52.0849998655991,
-28.8159670278695));
#22025=CARTESIAN_POINT('Ctrl Pts',(-16.9318840170255,-50.5316820606504,
-28.7358704836581));
#22026=CARTESIAN_POINT('Ctrl Pts',(-16.9313402641813,-49.9996515904955,
-28.7084234471775));
#22027=CARTESIAN_POINT('Ctrl Pts',(-16.9300226261573,-49.9980579824143,
-29.7915765528225));
#22028=CARTESIAN_POINT('Ctrl Pts',(-16.9278229920328,-49.6222178059028,
-29.7721663660449));
#22029=CARTESIAN_POINT('Ctrl Pts',(-17.1652526647347,-48.2296053591559,
-29.7001066715364));
#22030=CARTESIAN_POINT('Ctrl Pts',(-19.2351493773684,-46.4550967253995,
-29.5753974692971));
#22031=CARTESIAN_POINT('Ctrl Pts',(-22.5502120400548,-47.4216760770047,
-29.4174489461046));
#22032=CARTESIAN_POINT('Ctrl Pts',(-23.5530750072187,-50.7259433133794,
-29.2595004229121));
#22033=CARTESIAN_POINT('Ctrl Pts',(-21.3344729272248,-53.3720198261462,
-29.1015518997197));
#22034=CARTESIAN_POINT('Ctrl Pts',(-17.9487915178527,-52.9659277200364,
-28.9455772763565));
#22035=CARTESIAN_POINT('Ctrl Pts',(-16.9246872558677,-50.9737418027382,
-28.8422521607241));
#22036=CARTESIAN_POINT('Ctrl Pts',(-16.9217184048747,-49.9993152064879,
-28.7915765528225));
#22037=CARTESIAN_POINT('Origin',(-20.,-50.,-42.2084234471774));
#22038=CARTESIAN_POINT('',(-16.9284011455975,-50.0025559503523,-30.7915765528225));
#22039=CARTESIAN_POINT('',(-16.9237529572543,-49.9977977476302,-30.7084234471775));
#22040=CARTESIAN_POINT('',(-16.9265,-49.9999999999998,-42.2084234471774));
#22041=CARTESIAN_POINT('Ctrl Pts',(-16.9237529572543,-49.9977977476302,
-30.7084234471775));
#22042=CARTESIAN_POINT('Ctrl Pts',(-16.9225921162906,-49.8547648374716,
-30.7009979097613));
#22043=CARTESIAN_POINT('Ctrl Pts',(-16.9963970139262,-48.6987851336448,
-30.6409228646142));
#22044=CARTESIAN_POINT('Ctrl Pts',(-18.4605641466087,-46.7164840335274,
-30.5281983117364));
#22045=CARTESIAN_POINT('Ctrl Pts',(-21.9079002499127,-46.9159674960896,
-30.370249788544));
#22046=CARTESIAN_POINT('Ctrl Pts',(-23.6254012227827,-49.9116494333404,
-30.2123012653514));
#22047=CARTESIAN_POINT('Ctrl Pts',(-22.0558611685522,-52.9874361423172,
-30.054352742159));
#22048=CARTESIAN_POINT('Ctrl Pts',(-18.6223343189813,-53.3546053598246,
-29.8964042189665));
#22049=CARTESIAN_POINT('Ctrl Pts',(-17.0275920921308,-51.402205940021,-29.7810944539727));
#22050=CARTESIAN_POINT('Ctrl Pts',(-16.9234267298995,-50.1956548331446,
-29.7184341967097));
#22051=CARTESIAN_POINT('Ctrl Pts',(-16.9251595829395,-50.0025957433342,
-29.7084234471775));
#22052=CARTESIAN_POINT('Ctrl Pts',(-16.9284011455975,-50.0025559503523,
-30.7915765528225));
#22053=CARTESIAN_POINT('Ctrl Pts',(-16.9341000870249,-49.2900464772943,
-30.7547300790965));
#22054=CARTESIAN_POINT('Ctrl Pts',(-17.534439658132,-47.5507753552286,-30.6652340976396));
#22055=CARTESIAN_POINT('Ctrl Pts',(-20.4203163327858,-46.3979630926968,
-30.5230886084519));
#22056=CARTESIAN_POINT('Ctrl Pts',(-23.2459424988316,-48.3828441647573,
-30.3651400852595));
#22057=CARTESIAN_POINT('Ctrl Pts',(-23.1285713220653,-51.8339512490605,
-30.207191562067));
#22058=CARTESIAN_POINT('Ctrl Pts',(-20.1746196787779,-53.6222705129474,
-30.0492430388745));
#22059=CARTESIAN_POINT('Ctrl Pts',(-17.4448109217873,-52.3102153453405,
-29.9107047024597));
#22060=CARTESIAN_POINT('Ctrl Pts',(-16.9337894288924,-50.6416722040218,
-29.8248158737757));
#22061=CARTESIAN_POINT('Ctrl Pts',(-16.9300226261573,-49.9980579824143,
-29.7915765528225));
#22062=CARTESIAN_POINT('Origin',(-20.,-50.,-42.2084234471774));
#22063=CARTESIAN_POINT('',(-16.9216591696857,-49.9994310993742,-31.7915765528225));
#22064=CARTESIAN_POINT('',(-16.9313143876478,-49.999546673736,-31.7084234471775));
#22065=CARTESIAN_POINT('',(-16.9265,-49.9999999999998,-42.2084234471774));
#22066=CARTESIAN_POINT('Ctrl Pts',(-16.9313143876478,-49.999546673736,-31.7084234471775));
#22067=CARTESIAN_POINT('Ctrl Pts',(-16.9306732233893,-49.5176378400166,
-31.6835616228129));
#22068=CARTESIAN_POINT('Ctrl Pts',(-17.2638485165257,-48.0160365216701,
-31.6060502907175));
#22069=CARTESIAN_POINT('Ctrl Pts',(-19.6028209425392,-46.3953379291391,
-31.4758894508912));
#22070=CARTESIAN_POINT('Ctrl Pts',(-22.8012443962967,-47.696878274818,-31.3179409276987));
#22071=CARTESIAN_POINT('Ctrl Pts',(-23.459864751929,-51.0865890424386,-31.1599924045063));
#22072=CARTESIAN_POINT('Ctrl Pts',(-20.9815309640172,-53.4911225723918,
-31.0020438813138));
#22073=CARTESIAN_POINT('Ctrl Pts',(-17.7716227612056,-52.7661266417806,
-30.8515208955375));
#22074=CARTESIAN_POINT('Ctrl Pts',(-16.9308228613352,-50.8689153140057,
-30.7536474174921));
#22075=CARTESIAN_POINT('Ctrl Pts',(-16.9237529572543,-49.9977977476302,
-30.7084234471775));
#22076=CARTESIAN_POINT('Ctrl Pts',(-16.9216591696857,-49.9994310993742,
-31.7915765528225));
#22077=CARTESIAN_POINT('Ctrl Pts',(-16.9215784879871,-49.9680273721396,
-31.7899432998789));
#22078=CARTESIAN_POINT('Ctrl Pts',(-16.936183371105,-48.9243706066136,-31.7356605392045));
#22079=CARTESIAN_POINT('Ctrl Pts',(-18.1119419466013,-46.9037809366621,
-31.6287282707992));
#22080=CARTESIAN_POINT('Ctrl Pts',(-21.5604873228824,-46.7264369539744,
-31.4707797476067));
#22081=CARTESIAN_POINT('Ctrl Pts',(-23.5941863035827,-49.5171330241987,
-31.3128312244142));
#22082=CARTESIAN_POINT('Ctrl Pts',(-22.3691458750596,-52.7456298956467,
-31.1548827012218));
#22083=CARTESIAN_POINT('Ctrl Pts',(-18.9960729359346,-53.4847476452704,
-30.9969341780293));
#22084=CARTESIAN_POINT('Ctrl Pts',(-17.1077658789735,-51.6289846027671,
-30.8758321285629));
#22085=CARTESIAN_POINT('Ctrl Pts',(-16.9259569343593,-50.3081431692316,
-30.8073795868273));
#22086=CARTESIAN_POINT('Ctrl Pts',(-16.9284011455975,-50.0025559503523,
-30.7915765528225));
#22087=CARTESIAN_POINT('Origin',(-20.,-50.,-42.2084234471774));
#22088=CARTESIAN_POINT('',(-16.929891726575,-49.9979840334756,-32.7915765528225));
#22089=CARTESIAN_POINT('',(-16.9253537624756,-50.0026288890115,-32.7084234471775));
#22090=CARTESIAN_POINT('',(-16.9265,-49.9999999999998,-42.2084234471774));
#22091=CARTESIAN_POINT('Ctrl Pts',(-16.9253537624756,-50.0026288890115,
-32.7084234471775));
#22092=CARTESIAN_POINT('Ctrl Pts',(-16.9327154506849,-49.1867693143368,
-32.6661253358645));
#22093=CARTESIAN_POINT('Ctrl Pts',(-17.6840555158499,-47.3434039731563,
-32.5711777168206));
#22094=CARTESIAN_POINT('Ctrl Pts',(-20.7875967978108,-46.460080349377,-32.423580590046));
#22095=CARTESIAN_POINT('Ctrl Pts',(-23.3947079863477,-48.724344272064,-32.2656320668535));
#22096=CARTESIAN_POINT('Ctrl Pts',(-22.9239406890394,-52.1452064459554,
-32.1076835436611));
#22097=CARTESIAN_POINT('Ctrl Pts',(-19.8021252966153,-53.6210751788038,
-31.9497350204686));
#22098=CARTESIAN_POINT('Ctrl Pts',(-17.3228655042439,-52.0982946435502,
-31.8166483216408));
#22099=CARTESIAN_POINT('Ctrl Pts',(-16.9320310071983,-50.5381688555359,
-31.7362111305437));
#22100=CARTESIAN_POINT('Ctrl Pts',(-16.9313143876478,-49.999546673736,-31.7084234471775));
#22101=CARTESIAN_POINT('Ctrl Pts',(-16.929891726575,-49.9979840334756,-32.7915765528225));
#22102=CARTESIAN_POINT('Ctrl Pts',(-16.9276422677924,-49.6287794061046,
-32.7725070129305));
#22103=CARTESIAN_POINT('Ctrl Pts',(-17.1595661457499,-48.2429604363447,
-32.7007879653077));
#22104=CARTESIAN_POINT('Ctrl Pts',(-19.2124033263834,-46.4600809075787,
-32.576419409954));
#22105=CARTESIAN_POINT('Ctrl Pts',(-22.533604054109,-47.405354321264,-32.4184708867615));
#22106=CARTESIAN_POINT('Ctrl Pts',(-23.5576630420582,-50.7031140592781,
-32.2605223635691));
#22107=CARTESIAN_POINT('Ctrl Pts',(-21.3560971512034,-53.3633816639922,
-32.1025738403766));
#22108=CARTESIAN_POINT('Ctrl Pts',(-17.9604781864533,-52.9781979806717,
-31.9462585701277));
#22109=CARTESIAN_POINT('Ctrl Pts',(-16.9241793415355,-50.9803572664544,
-31.8425928076097));
#22110=CARTESIAN_POINT('Ctrl Pts',(-16.9216591696857,-49.9994310993742,
-31.7915765528225));
#22111=CARTESIAN_POINT('Origin',(-20.,-50.,-42.2084234471774));
#22112=CARTESIAN_POINT('',(-16.9285739275939,-50.0025153259756,-33.7915765528225));
#22113=CARTESIAN_POINT('',(-16.9235810583994,-49.9978675316839,-33.7084234471775));
#22114=CARTESIAN_POINT('',(-16.9265,-49.9999999999998,-42.2084234471774));
#22115=CARTESIAN_POINT('Ctrl Pts',(-16.9235810583994,-49.9978675316839,
-33.7084234471775));
#22116=CARTESIAN_POINT('Ctrl Pts',(-16.92249854389,-49.861416180346,-33.7013385566469));
#22117=CARTESIAN_POINT('Ctrl Pts',(-16.992489904441,-48.7120794050224,-33.6416041583855));
#22118=CARTESIAN_POINT('Ctrl Pts',(-18.4395124310478,-46.7264364377739,
-33.5292202523933));
#22119=CARTESIAN_POINT('Ctrl Pts',(-21.8880583511222,-46.9037804484265,
-33.3712717292008));
#22120=CARTESIAN_POINT('Ctrl Pts',(-23.6247591869331,-49.8883725592297,
-33.2133232060084));
#22121=CARTESIAN_POINT('Ctrl Pts',(-22.0750011100191,-52.9741738755843,
-33.0553746828159));
#22122=CARTESIAN_POINT('Ctrl Pts',(-18.6439026349568,-53.3633821943561,
-32.8974261596234));
#22123=CARTESIAN_POINT('Ctrl Pts',(-17.0319088216555,-51.4155254718575,
-32.781775747744));
#22124=CARTESIAN_POINT('Ctrl Pts',(-16.9235521748729,-50.2022899522738,
-32.7187748435953));
#22125=CARTESIAN_POINT('Ctrl Pts',(-16.9253537624756,-50.0026288890115,
-32.7084234471775));
#22126=CARTESIAN_POINT('Ctrl Pts',(-16.9285739275939,-50.0025153259756,
-33.7915765528225));
#22127=CARTESIAN_POINT('Ctrl Pts',(-16.9341074121984,-49.2964924381661,
-33.7550707259821));
#22128=CARTESIAN_POINT('Ctrl Pts',(-17.5256620424174,-47.5638501786645,
-33.6659153914109));
#22129=CARTESIAN_POINT('Ctrl Pts',(-20.3971789948304,-46.3953384975499,
-33.5241105491088));
#22130=CARTESIAN_POINT('Ctrl Pts',(-23.2354918292762,-48.3620353105553,
-33.3661620259163));
#22131=CARTESIAN_POINT('Ctrl Pts',(-23.1402826251531,-51.8138248910362,
-33.2082135027239));
#22132=CARTESIAN_POINT('Ctrl Pts',(-20.1978746721824,-53.6210746078049,
-33.0502649795314));
#22133=CARTESIAN_POINT('Ctrl Pts',(-17.4529646811151,-52.3233915865314,
-32.9113859962309));
#22134=CARTESIAN_POINT('Ctrl Pts',(-16.9338528475042,-50.6481244974432,
-32.8251565206613));
#22135=CARTESIAN_POINT('Ctrl Pts',(-16.929891726575,-49.9979840334756,-32.7915765528225));
#22136=CARTESIAN_POINT('Origin',(-20.,-50.,-42.2084234471774));
#22137=CARTESIAN_POINT('',(-16.9216102653814,-49.9995482667975,-34.7915765528225));
#22138=CARTESIAN_POINT('',(-16.931281743668,-49.9994424172085,-34.7084234471775));
#22139=CARTESIAN_POINT('',(-16.9265,-49.9999999999998,-42.2084234471774));
#22140=CARTESIAN_POINT('Ctrl Pts',(-16.931281743668,-49.9994424172085,-34.7084234471775));
#22141=CARTESIAN_POINT('Ctrl Pts',(-16.9305034541633,-49.5241491461598,
-34.6839022696985));
#22142=CARTESIAN_POINT('Ctrl Pts',(-17.2572599119806,-48.029365460058,-34.6067315844887));
#22143=CARTESIAN_POINT('Ctrl Pts',(-19.5796836009353,-46.3979625246999,
-34.4769113915481));
#22144=CARTESIAN_POINT('Ctrl Pts',(-22.7863983082339,-47.678938967485,-34.3189628683557));
#22145=CARTESIAN_POINT('Ctrl Pts',(-23.4667704139307,-51.0643508565711,
-34.1610143451631));
#22146=CARTESIAN_POINT('Ctrl Pts',(-21.0039272223724,-53.4847481947722,
-34.0030658219707));
#22147=CARTESIAN_POINT('Ctrl Pts',(-17.7821553008139,-52.7787839729962,
-33.8522021893088));
#22148=CARTESIAN_POINT('Ctrl Pts',(-16.9305429668472,-50.8754186474492,
-33.7539880643777));
#22149=CARTESIAN_POINT('Ctrl Pts',(-16.9235810583994,-49.9978675316839,
-33.7084234471775));
#22150=CARTESIAN_POINT('Ctrl Pts',(-16.9216102653814,-49.9995482667975,
-34.7915765528225));
#22151=CARTESIAN_POINT('Ctrl Pts',(-16.9215587791314,-49.9746954627831,
-34.7902839467645));
#22152=CARTESIAN_POINT('Ctrl Pts',(-16.9330440427449,-48.9376047691407,
-34.7363418329757));
#22153=CARTESIAN_POINT('Ctrl Pts',(-18.0921000509396,-46.9159679824036,
-34.6297502114561));
#22154=CARTESIAN_POINT('Ctrl Pts',(-21.5394356106412,-46.7164845512972,
-34.4718016882636));
#22155=CARTESIAN_POINT('Ctrl Pts',(-23.5910117219915,-49.4940647139208,
-34.3138531650712));
#22156=CARTESIAN_POINT('Ctrl Pts',(-22.386726720697,-52.7303610131065,-34.1559046418786));
#22157=CARTESIAN_POINT('Ctrl Pts',(-19.0184691907583,-53.491122021885,-33.9979561186862));
#22158=CARTESIAN_POINT('Ctrl Pts',(-17.1129401986479,-51.642336206118,-33.8765134223342));
#22159=CARTESIAN_POINT('Ctrl Pts',(-16.9261268987933,-50.3147342013879,
-33.8077202337129));
#22160=CARTESIAN_POINT('Ctrl Pts',(-16.9285739275939,-50.0025153259756,
-33.7915765528225));
#22161=CARTESIAN_POINT('Origin',(-20.,-50.,-42.2084234471774));
#22162=CARTESIAN_POINT('',(-16.929755691605,-49.9979131056248,-35.7915765528225));
#22163=CARTESIAN_POINT('',(-16.9255489617634,-50.0026575650068,-35.7084234471774));
#22164=CARTESIAN_POINT('',(-16.9265,-49.9999999999998,-42.2084234471774));
#22165=CARTESIAN_POINT('Ctrl Pts',(-16.9255489617634,-50.0026575650068,
-35.7084234471774));
#22166=CARTESIAN_POINT('Ctrl Pts',(-16.9328792376806,-49.193236061542,-35.6664659827501));
#22167=CARTESIAN_POINT('Ctrl Pts',(-17.6741948420038,-47.3562447964742,
-35.5718590105919));
#22168=CARTESIAN_POINT('Ctrl Pts',(-20.764850743239,-46.4550961664119,-35.4246025307029));
#22169=CARTESIAN_POINT('Ctrl Pts',(-23.38644702166,-48.7025731549433,-35.2666540075105));
#22170=CARTESIAN_POINT('Ctrl Pts',(-22.9376547796718,-52.1263876044256,
-35.108705484318));
#22171=CARTESIAN_POINT('Ctrl Pts',(-19.8253802936868,-53.6222710841349,
-34.9507569611255));
#22172=CARTESIAN_POINT('Ctrl Pts',(-17.330023063912,-52.1115844029815,-34.817329615412));
#22173=CARTESIAN_POINT('Ctrl Pts',(-16.9321745223381,-50.5446530257126,
-34.7365517774293));
#22174=CARTESIAN_POINT('Ctrl Pts',(-16.931281743668,-49.9994424172085,-34.7084234471775));
#22175=CARTESIAN_POINT('Ctrl Pts',(-16.929755691605,-49.9979131056248,-35.7915765528225));
#22176=CARTESIAN_POINT('Ctrl Pts',(-16.927462104359,-49.6353441575151,-35.7728476598161));
#22177=CARTESIAN_POINT('Ctrl Pts',(-17.1539340252026,-48.2563157484261,
-35.7014692590789));
#22178=CARTESIAN_POINT('Ctrl Pts',(-19.1896897477077,-46.4652110393336,
-35.5774413506109));
#22179=CARTESIAN_POINT('Ctrl Pts',(-22.5168916085772,-47.3891395418682,
-35.4194928274184));
#22180=CARTESIAN_POINT('Ctrl Pts',(-23.5621043957074,-50.6802558160081,
-35.261544304226));
#22181=CARTESIAN_POINT('Ctrl Pts',(-21.3776654637779,-53.3546048308447,
-35.1035957810335));
#22182=CARTESIAN_POINT('Ctrl Pts',(-17.9722381641981,-52.9904404798302,
-34.946939863899));
#22183=CARTESIAN_POINT('Ctrl Pts',(-16.923655880331,-50.9869821444003,-34.8429334544954));
#22184=CARTESIAN_POINT('Ctrl Pts',(-16.9216102653814,-49.9995482667975,
-34.7915765528225));
#22185=CARTESIAN_POINT('Origin',(-20.,-50.,-42.2084234471774));
#22186=CARTESIAN_POINT('',(-16.9287431816361,-50.0024708147691,-36.7915765528225));
#22187=CARTESIAN_POINT('',(-16.9234134019188,-49.9979412457337,-36.7084234471775));
#22188=CARTESIAN_POINT('',(-16.9265,-49.9999999999998,-42.2084234471774));
#22189=CARTESIAN_POINT('Ctrl Pts',(-16.9234134019188,-49.9979412457337,
-36.7084234471775));
#22190=CARTESIAN_POINT('Ctrl Pts',(-16.9224089863605,-49.8680690942478,
-36.7016792035325));
#22191=CARTESIAN_POINT('Ctrl Pts',(-16.9886295015825,-48.7253704503755,
-36.6422854521568));
#22192=CARTESIAN_POINT('Ctrl Pts',(-18.4185250538729,-46.7365238104494,
-36.5302421930502));
#22193=CARTESIAN_POINT('Ctrl Pts',(-21.868138608337,-46.8917210565137,-36.3722936698577));
#22194=CARTESIAN_POINT('Ctrl Pts',(-23.6239677035562,-49.865100287622,-36.2143451466653));
#22195=CARTESIAN_POINT('Ctrl Pts',(-22.0940554999228,-52.9607889846439,
-36.0563966234728));
#22196=CARTESIAN_POINT('Ctrl Pts',(-18.6655268623454,-53.3720203578719,
-35.8984481002803));
#22197=CARTESIAN_POINT('Ctrl Pts',(-17.0362742450073,-51.4288476172636,
-35.7824570415152));
#22198=CARTESIAN_POINT('Ctrl Pts',(-16.9236809835954,-50.2089228835601,
-35.7191154904809));
#22199=CARTESIAN_POINT('Ctrl Pts',(-16.9255489617634,-50.0026575650068,
-35.7084234471774));
#22200=CARTESIAN_POINT('Ctrl Pts',(-16.9287431816361,-50.0024708147691,
-36.7915765528225));
#22201=CARTESIAN_POINT('Ctrl Pts',(-16.9341065503311,-49.3029384889418,
-36.7554113728678));
#22202=CARTESIAN_POINT('Ctrl Pts',(-17.5169503973051,-47.5769368622601,
-36.6665966851822));
#22203=CARTESIAN_POINT('Ctrl Pts',(-20.3740252799296,-46.3928625195443,
-36.5251324897657));
#22204=CARTESIAN_POINT('Ctrl Pts',(-23.2249077622416,-48.3412939899481,
-36.3671839665732));
#22205=CARTESIAN_POINT('Ctrl Pts',(-23.1518644551494,-51.7936237492067,
-36.2092354433807));
#22206=CARTESIAN_POINT('Ctrl Pts',(-20.2211215074614,-53.6197294072659,
-36.0512869201883));
#22207=CARTESIAN_POINT('Ctrl Pts',(-17.4611825776843,-52.3365584976905,
-35.9120672900022));
#22208=CARTESIAN_POINT('Ctrl Pts',(-16.933909695223,-50.654575600075,-35.825497167547));
#22209=CARTESIAN_POINT('Ctrl Pts',(-16.929755691605,-49.9979131056248,-35.7915765528225));
#22210=CARTESIAN_POINT('Origin',(-20.,-50.,-42.2084234471774));
#22211=CARTESIAN_POINT('',(-16.9215720097223,-49.9996663583571,-37.7915765528225));
#22212=CARTESIAN_POINT('',(-16.9312423703737,-49.999338997349,-37.7084234471775));
#22213=CARTESIAN_POINT('',(-16.9265,-49.9999999999998,-42.2084234471774));
#22214=CARTESIAN_POINT('Ctrl Pts',(-16.9312423703737,-49.999338997349,-37.7084234471775));
#22215=CARTESIAN_POINT('Ctrl Pts',(-16.9303318355252,-49.53066349442,-37.6842429165841));
#22216=CARTESIAN_POINT('Ctrl Pts',(-17.2507294124538,-48.0426973366553,
-37.60741287826));
#22217=CARTESIAN_POINT('Ctrl Pts',(-19.5565635911389,-46.4007356661223,
-37.477933332205));
#22218=CARTESIAN_POINT('Ctrl Pts',(-22.7714373367961,-47.6610953390299,
-37.3199848090126));
#22219=CARTESIAN_POINT('Ctrl Pts',(-23.4735331428005,-51.0420687967573,
-37.1620362858201));
#22220=CARTESIAN_POINT('Ctrl Pts',(-21.0262820888715,-53.4782301377694,
-37.0040877626276));
#22221=CARTESIAN_POINT('Ctrl Pts',(-17.792758810687,-52.7914201594648,-36.8528834830801));
#22222=CARTESIAN_POINT('Ctrl Pts',(-16.9302500412638,-50.8819270157086,
-36.7543287112634));
#22223=CARTESIAN_POINT('Ctrl Pts',(-16.9234134019188,-49.9979412457337,
-36.7084234471775));
#22224=CARTESIAN_POINT('Ctrl Pts',(-16.9215720097223,-49.9996663583571,
-37.7915765528225));
#22225=CARTESIAN_POINT('Ctrl Pts',(-16.9215435649973,-49.9813637458573,
-37.7906245936502));
#22226=CARTESIAN_POINT('Ctrl Pts',(-16.9299480198382,-48.9508349433177,
-37.737023126747));
#22227=CARTESIAN_POINT('Ctrl Pts',(-18.0723369901302,-46.9282824012858,
-37.630772152113));
#22228=CARTESIAN_POINT('Ctrl Pts',(-21.5183203411933,-46.7066674164727,
-37.4728236289205));
#22229=CARTESIAN_POINT('Ctrl Pts',(-23.5876891278802,-49.4710173186029,
-37.3148751057281));
#22230=CARTESIAN_POINT('Ctrl Pts',(-22.4042091405233,-52.7149795309031,
-37.1569265825355));
#22231=CARTESIAN_POINT('Ctrl Pts',(-19.0409059247592,-53.4973524747668,
-36.9989780593431));
#22232=CARTESIAN_POINT('Ctrl Pts',(-17.1181669524113,-51.6556887349243,
-36.8771947161054));
#22233=CARTESIAN_POINT('Ctrl Pts',(-16.9262985227775,-50.3213222670024,
-36.8080608805986));
#22234=CARTESIAN_POINT('Ctrl Pts',(-16.9287431816361,-50.0024708147691,
-36.7915765528225));
#22235=CARTESIAN_POINT('Origin',(-20.,-50.,-42.2084234471774));
#22236=CARTESIAN_POINT('',(-16.9296186885438,-49.9978504047438,-38.7915765528225));
#22237=CARTESIAN_POINT('',(-16.9257450511401,-50.0026845218917,-38.7084234471775));
#22238=CARTESIAN_POINT('',(-16.9265,-49.9999999999998,-42.2084234471774));
#22239=CARTESIAN_POINT('Ctrl Pts',(-16.9257450511401,-50.0026845218917,
-38.7084234471775));
#22240=CARTESIAN_POINT('Ctrl Pts',(-16.9330320360583,-49.1997027895944,
-38.6668066296358));
#22241=CARTESIAN_POINT('Ctrl Pts',(-17.6644030329328,-47.369098904382,-38.5725403043632));
#22242=CARTESIAN_POINT('Ctrl Pts',(-20.7420732981751,-46.4502603278007,
-38.4256244713598));
#22243=CARTESIAN_POINT('Ctrl Pts',(-23.3780463626243,-48.6808544307687,
-38.2676759481674));
#22244=CARTESIAN_POINT('Ctrl Pts',(-22.95124778817,-52.107481644896,-38.1097274249748));
#22245=CARTESIAN_POINT('Ctrl Pts',(-19.8486424720205,-53.6233173671768,
-37.9517789017825));
#22246=CARTESIAN_POINT('Ctrl Pts',(-17.3372411809546,-52.1248689915217,
-37.8180109091832));
#22247=CARTESIAN_POINT('Ctrl Pts',(-16.9323143896863,-50.5511346714054,
-37.7368924243149));
#22248=CARTESIAN_POINT('Ctrl Pts',(-16.9312423703737,-49.999338997349,-37.7084234471775));
#22249=CARTESIAN_POINT('Ctrl Pts',(-16.9296186885438,-49.9978504047438,
-38.7915765528226));
#22250=CARTESIAN_POINT('Ctrl Pts',(-16.9272829236679,-49.6419124103458,
-38.7731883067018));
#22251=CARTESIAN_POINT('Ctrl Pts',(-17.1483416537186,-48.2696528264275,
-38.7021505528502));
#22252=CARTESIAN_POINT('Ctrl Pts',(-19.1670203242729,-46.4705005646606,
-38.5784632912678));
#22253=CARTESIAN_POINT('Ctrl Pts',(-22.5000699934528,-47.373025546768,-38.4205147680754));
#22254=CARTESIAN_POINT('Ctrl Pts',(-23.5664015975527,-50.657372972797,-38.2625662448828));
#22255=CARTESIAN_POINT('Ctrl Pts',(-21.3991756129266,-53.3456879568638,
-38.1046177216904));
#22256=CARTESIAN_POINT('Ctrl Pts',(-17.9840722489439,-53.0026556344016,
-37.9476211576703));
#22257=CARTESIAN_POINT('Ctrl Pts',(-16.9231167425166,-50.9936167565737,
-37.843274101381));
#22258=CARTESIAN_POINT('Ctrl Pts',(-16.9215720097223,-49.9996663583571,
-37.7915765528225));
#22259=CARTESIAN_POINT('Origin',(-20.,-50.,-42.2084234471774));
#22260=CARTESIAN_POINT('',(-16.9296932342852,-50.0033456701988,-39.7915765528225));
#22261=CARTESIAN_POINT('',(-16.9232551256392,-49.9980895495447,-39.7084234471775));
#22262=CARTESIAN_POINT('',(-16.9265,-49.9999999999998,-42.2084234471774));
#22263=CARTESIAN_POINT('',(-19.2062007174672,-52.9692229537457,-40.));
#22264=CARTESIAN_POINT('Ctrl Pts',(-19.2062007174672,-52.9692229537457,
-40.));
#22265=CARTESIAN_POINT('Ctrl Pts',(-18.2239621276955,-52.7066289013681,
-39.9473504922692));
#22266=CARTESIAN_POINT('Ctrl Pts',(-17.1241887959713,-51.6693975435551,
-39.8778760098767));
#22267=CARTESIAN_POINT('Ctrl Pts',(-16.9273403835209,-50.3288691193977,
-39.8084015274842));
#22268=CARTESIAN_POINT('Ctrl Pts',(-16.9296932342852,-50.0033456701988,
-39.7915765528225));
#22269=CARTESIAN_POINT('',(-20.7956622540211,-52.9742863856178,-40.));
#22270=CARTESIAN_POINT('Origin',(-20.,-50.,-40.));
#22271=CARTESIAN_POINT('Ctrl Pts',(-20.7956661367394,-52.9742969385866,
-40.));
#22272=CARTESIAN_POINT('Ctrl Pts',(-19.8486502888634,-53.2252253736959,
-39.9490537266974));
#22273=CARTESIAN_POINT('Ctrl Pts',(-17.7883286491776,-52.7701106788771,
-39.8518615424231));
#22274=CARTESIAN_POINT('Ctrl Pts',(-16.9299363715263,-50.888322508111,-39.754669358149));
#22275=CARTESIAN_POINT('Ctrl Pts',(-16.9232551256392,-49.9980895495447,
-39.7084234471775));
#22276=CARTESIAN_POINT('Origin',(0.,0.,-48.));
#22277=CARTESIAN_POINT('',(-7.26252539463726,0.000110654559175658,-46.6717617050839));
#22278=CARTESIAN_POINT('',(-7.26321021083306,-0.000162629342338461,-47.0782382949161));
#22279=CARTESIAN_POINT('',(-7.263,-8.89460970220723E-16,-48.));
#22280=CARTESIAN_POINT('',(5.46288453460432,-4.78623668048091,-48.));
#22281=CARTESIAN_POINT('Ctrl Pts',(-7.26321021083306,-0.000162629342338461,
-47.0782382949161));
#22282=CARTESIAN_POINT('Ctrl Pts',(-7.26225254003205,0.986861826811056,
-47.1106847833874));
#22283=CARTESIAN_POINT('Ctrl Pts',(-7.05946423163692,1.97426720615771,-47.1431312718588));
#22284=CARTESIAN_POINT('Ctrl Pts',(-6.66813922368638,2.88023829893362,-47.1755777603301));
#22285=CARTESIAN_POINT('Ctrl Pts',(-6.19466067823692,3.97640610449594,-47.2148359622192));
#22286=CARTESIAN_POINT('Ctrl Pts',(-5.44517436528813,4.95335841680263,-47.2540941641082));
#22287=CARTESIAN_POINT('Ctrl Pts',(-4.50904795872082,5.694592197166,-47.2933523659972));
#22288=CARTESIAN_POINT('Ctrl Pts',(-3.5729215521535,6.43582597752937,-47.3326105678863));
#22289=CARTESIAN_POINT('Ctrl Pts',(-2.45015505196766,6.94134122594944,-47.3718687697753));
#22290=CARTESIAN_POINT('Ctrl Pts',(-1.27463114363028,7.15088143827442,-47.4111269716644));
#22291=CARTESIAN_POINT('Ctrl Pts',(-0.0991072352929019,7.36042165059941,
-47.4503851735534));
#22292=CARTESIAN_POINT('Ctrl Pts',(1.129174081196,7.27398682682932,-47.4896433754424));
#22293=CARTESIAN_POINT('Ctrl Pts',(2.26375827103325,6.90183984862936,-47.5289015773315));
#22294=CARTESIAN_POINT('Ctrl Pts',(3.3983424608705,6.52969287042939,-47.5681597792205));
#22295=CARTESIAN_POINT('Ctrl Pts',(4.4392295240561,5.87183373779956,-47.6074179811096));
#22296=CARTESIAN_POINT('Ctrl Pts',(5.26228985868794,5.00679499485275,-47.6466761829986));
#22297=CARTESIAN_POINT('Ctrl Pts',(6.08535019331978,4.14175625190593,-47.6859343848877));
#22298=CARTESIAN_POINT('Ctrl Pts',(6.69058379939787,3.06953789864212,-47.7251925867767));
#22299=CARTESIAN_POINT('Ctrl Pts',(7.00585036078105,1.91780922016447,-47.7644507886658));
#22300=CARTESIAN_POINT('Ctrl Pts',(7.32111692216422,0.766080541686827,-47.8037089905548));
#22301=CARTESIAN_POINT('Ctrl Pts',(7.3464164388525,-0.465158462004661,-47.8429671924438));
#22302=CARTESIAN_POINT('Ctrl Pts',(7.07862576269182,-1.62865261403763,-47.8822253943329));
#22303=CARTESIAN_POINT('Ctrl Pts',(6.81083508653114,-2.7921467660706,-47.9214835962219));
#22304=CARTESIAN_POINT('Ctrl Pts',(6.2499542175215,-3.88789606644505,-47.960741798111));
#22305=CARTESIAN_POINT('Ctrl Pts',(5.46288453460432,-4.78623668048091,-48.));
#22306=CARTESIAN_POINT('',(-5.46328272950459,-4.78643225728875,-48.));
#22307=CARTESIAN_POINT('Origin',(0.,0.,-48.));
#22308=CARTESIAN_POINT('Ctrl Pts',(-5.46328272950459,-4.78643225728875,
-48.));
#22309=CARTESIAN_POINT('Ctrl Pts',(-4.76265400353559,-5.58484241293595,
-47.9650783907933));
#22310=CARTESIAN_POINT('Ctrl Pts',(-3.88494971070624,-6.2285788144042,-47.9301567815866));
#22311=CARTESIAN_POINT('Ctrl Pts',(-2.91187904120844,-6.65437822564185,
-47.8952351723799));
#22312=CARTESIAN_POINT('Ctrl Pts',(-1.81797169663776,-7.1330537400391,-47.8559769704909));
#22313=CARTESIAN_POINT('Ctrl Pts',(-0.603542001115805,-7.33630431601018,
-47.8167187686018));
#22314=CARTESIAN_POINT('Ctrl Pts',(0.586609853467524,-7.23987447027158,
-47.7774605667127));
#22315=CARTESIAN_POINT('Ctrl Pts',(1.77676170805086,-7.14344462453298,-47.7382023648237));
#22316=CARTESIAN_POINT('Ctrl Pts',(2.94263572169557,-6.74733435708469,-47.6989441629347));
#22317=CARTESIAN_POINT('Ctrl Pts',(3.94520772278473,-6.09878584913582,-47.6596859610456));
#22318=CARTESIAN_POINT('Ctrl Pts',(4.94777972387388,-5.45023734118695,-47.6204277591566));
#22319=CARTESIAN_POINT('Ctrl Pts',(5.78704971240747,-4.54925059273749,-47.5811695572675));
#22320=CARTESIAN_POINT('Ctrl Pts',(6.36294479614214,-3.50325510007056,-47.5419113553785));
#22321=CARTESIAN_POINT('Ctrl Pts',(6.9388398798768,-2.45725960740365,-47.5026531534894));
#22322=CARTESIAN_POINT('Ctrl Pts',(7.25136005881256,-1.26625537051926,-47.4633949516004));
#22323=CARTESIAN_POINT('Ctrl Pts',(7.26323910849272,-0.0722609117331363,
-47.4241367497114));
#22324=CARTESIAN_POINT('Ctrl Pts',(7.27511815817288,1.12173354705299,-47.3848785478223));
#22325=CARTESIAN_POINT('Ctrl Pts',(6.98635607859744,2.31871822774086,-47.3456203459333));
#22326=CARTESIAN_POINT('Ctrl Pts',(6.43138560219337,3.37596501114632,-47.3063621440442));
#22327=CARTESIAN_POINT('Ctrl Pts',(5.87641512578929,4.43321179455178,-47.2671039421552));
#22328=CARTESIAN_POINT('Ctrl Pts',(5.05523625255658,5.35072068067483,-47.2278457402662));
#22329=CARTESIAN_POINT('Ctrl Pts',(4.06576665043739,6.01908670620214,-47.1885875383771));
#22330=CARTESIAN_POINT('Ctrl Pts',(3.07629704831819,6.68745273172946,-47.1493293364881));
#22331=CARTESIAN_POINT('Ctrl Pts',(1.91853671731251,7.10667589666103,-47.1100711345991));
#22332=CARTESIAN_POINT('Ctrl Pts',(0.730537929376382,7.22676802273927,-47.07081293271));
#22333=CARTESIAN_POINT('Ctrl Pts',(-0.45746085855973,7.3468601488175,-47.031554730821));
#22334=CARTESIAN_POINT('Ctrl Pts',(-1.67569810342629,7.16782123604241,-46.9922965289319));
#22335=CARTESIAN_POINT('Ctrl Pts',(-2.77891042070149,6.71099986948637,-46.9530383270428));
#22336=CARTESIAN_POINT('Ctrl Pts',(-3.8821227379767,6.25417850293032,-46.9137801251538));
#22337=CARTESIAN_POINT('Ctrl Pts',(-4.87031012766054,5.51957468259332,-46.8745219232648));
#22338=CARTESIAN_POINT('Ctrl Pts',(-5.62564041196335,4.59478314278975,-46.8352637213757));
#22339=CARTESIAN_POINT('Ctrl Pts',(-6.38097069626616,3.66999160298619,-46.7960055194867));
#22340=CARTESIAN_POINT('Ctrl Pts',(-6.90344387518794,2.55501234371607,-46.7567473175976));
#22341=CARTESIAN_POINT('Ctrl Pts',(-7.13075990222278,1.38279622732194,-46.7174891157086));
#22342=CARTESIAN_POINT('Ctrl Pts',(-7.21901809040275,0.927669187060691,
-46.7022466455004));
#22343=CARTESIAN_POINT('Ctrl Pts',(-7.26278209805939,0.463913837991132,
-46.6870041752921));
#22344=CARTESIAN_POINT('Ctrl Pts',(-7.26252539463726,0.000110654559175658,
-46.6717617050839));
#22345=CARTESIAN_POINT('Origin',(0.,0.,-48.));
#22346=CARTESIAN_POINT('',(-7.26337486577337,0.000131920041138065,-45.1717617050839));
#22347=CARTESIAN_POINT('',(-7.26244595120635,-6.5281985395238E-5,-45.5782382949161));
#22348=CARTESIAN_POINT('',(-7.263,-8.89460970220723E-16,-48.));
#22349=CARTESIAN_POINT('Ctrl Pts',(-7.26244595120635,-6.5281985395238E-5,
-45.5782382949161));
#22350=CARTESIAN_POINT('Ctrl Pts',(-7.26222960724132,0.672113855431829,
-45.6003281588299));
#22351=CARTESIAN_POINT('Ctrl Pts',(-7.1696578432929,1.34435139215194,-45.6224180227437));
#22352=CARTESIAN_POINT('Ctrl Pts',(-6.98553937325194,1.99050304088456,-45.6445078866575));
#22353=CARTESIAN_POINT('Ctrl Pts',(-6.65832323029251,3.13884655154996,-45.6837660885465));
#22354=CARTESIAN_POINT('Ctrl Pts',(-6.04196091327337,4.20479895246961,-45.7230242904355));
#22355=CARTESIAN_POINT('Ctrl Pts',(-5.20994789013978,5.06125534521791,-45.7622824923246));
#22356=CARTESIAN_POINT('Ctrl Pts',(-4.37793486700618,5.91771173796621,-45.8015406942136));
#22357=CARTESIAN_POINT('Ctrl Pts',(-3.33027113775813,6.56467212254317,-45.8407988961027));
#22358=CARTESIAN_POINT('Ctrl Pts',(-2.19188084772556,6.92499249435054,-45.8800570979917));
#22359=CARTESIAN_POINT('Ctrl Pts',(-1.05349055769298,7.28531286615791,-45.9193152998808));
#22360=CARTESIAN_POINT('Ctrl Pts',(0.175626293124121,7.35899322519568,-45.9585735017698));
#22361=CARTESIAN_POINT('Ctrl Pts',(1.34890896305861,7.13724787896668,-45.9978317036589));
#22362=CARTESIAN_POINT('Ctrl Pts',(2.52219163299309,6.91550253273769,-46.0370899055479));
#22363=CARTESIAN_POINT('Ctrl Pts',(3.63964012204496,6.39833148124193,-46.076348107437));
#22364=CARTESIAN_POINT('Ctrl Pts',(4.56800910299865,5.64740254855039,-46.115606309326));
#22365=CARTESIAN_POINT('Ctrl Pts',(5.49637808395232,4.89647361585885,-46.154864511215));
#22366=CARTESIAN_POINT('Ctrl Pts',(6.23566755680782,3.91178680197153,-46.194122713104));
#22367=CARTESIAN_POINT('Ctrl Pts',(6.69772413224052,2.8107568596051,-46.2333809149931));
#22368=CARTESIAN_POINT('Ctrl Pts',(7.15978070767323,1.70972691723866,-46.2726391168821));
#22369=CARTESIAN_POINT('Ctrl Pts',(7.34460438568313,0.492353846393101,-46.3118973187712));
#22370=CARTESIAN_POINT('Ctrl Pts',(7.23015666890219,-0.696201984692038,
-46.3511555206602));
#22371=CARTESIAN_POINT('Ctrl Pts',(7.11570895212125,-1.88475781577716,-46.3904137225493));
#22372=CARTESIAN_POINT('Ctrl Pts',(6.70198984054947,-3.04449640710186,-46.4296719244383));
#22373=CARTESIAN_POINT('Ctrl Pts',(6.03833147527558,-4.03712965529138,-46.4689301263274));
#22374=CARTESIAN_POINT('Ctrl Pts',(5.37467311000168,-5.02976290348091,-46.5081883282164));
#22375=CARTESIAN_POINT('Ctrl Pts',(4.46107549102567,-5.85529080853525,-46.5474465301055));
#22376=CARTESIAN_POINT('Ctrl Pts',(3.40647665113655,-6.41527700380401,-46.5867047319945));
#22377=CARTESIAN_POINT('Ctrl Pts',(2.35187781124742,-6.97526319907276,-46.6259629338835));
#22378=CARTESIAN_POINT('Ctrl Pts',(1.15627775044517,-7.26970768455593,-46.6652211357726));
#22379=CARTESIAN_POINT('Ctrl Pts',(-0.0377594013239463,-7.26350039167212,
-46.7044793376616));
#22380=CARTESIAN_POINT('Ctrl Pts',(-1.23179655309304,-7.25729309878831,
-46.7437375395507));
#22381=CARTESIAN_POINT('Ctrl Pts',(-2.42427079582901,-6.95043402753753,
-46.7829957414397));
#22382=CARTESIAN_POINT('Ctrl Pts',(-3.47299058508026,-6.37951388512164,
-46.8222539433288));
#22383=CARTESIAN_POINT('Ctrl Pts',(-4.52171037433153,-5.80859374270573,
-46.8615121452178));
#22384=CARTESIAN_POINT('Ctrl Pts',(-5.42667571009807,-4.9736125291247,-46.9007703471068));
#22385=CARTESIAN_POINT('Ctrl Pts',(-6.0799780911766,-3.97413272045434,-46.9400285489959));
#22386=CARTESIAN_POINT('Ctrl Pts',(-6.73328047225512,-2.97465291178399,
-46.9792867508849));
#22387=CARTESIAN_POINT('Ctrl Pts',(-7.13491989864563,-1.8106745080243,-47.018544952774));
#22388=CARTESIAN_POINT('Ctrl Pts',(-7.23700422286582,-0.620993656735478,
-47.057803154663));
#22389=CARTESIAN_POINT('Ctrl Pts',(-7.25471693326944,-0.414571441056566,
-47.0646148680807));
#22390=CARTESIAN_POINT('Ctrl Pts',(-7.26341126121947,-0.207375429504603,
-47.0714265814984));
#22391=CARTESIAN_POINT('Ctrl Pts',(-7.26321021083306,-0.000162629342338461,
-47.0782382949161));
#22392=CARTESIAN_POINT('Ctrl Pts',(-7.26252539463726,0.000110654559175658,
-46.6717617050839));
#22393=CARTESIAN_POINT('Ctrl Pts',(-7.26212093785149,-0.730648379498221,
-46.6477459734031));
#22394=CARTESIAN_POINT('Ctrl Pts',(-7.15243715971961,-1.46152616008496,
-46.6237302417223));
#22395=CARTESIAN_POINT('Ctrl Pts',(-6.93532594245516,-2.15896185620489,
-46.5997145100415));
#22396=CARTESIAN_POINT('Ctrl Pts',(-6.58041708050481,-3.29905084981948,
-46.5604563081524));
#22397=CARTESIAN_POINT('Ctrl Pts',(-5.93844048145624,-4.34977586353051,
-46.5211981062634));
#22398=CARTESIAN_POINT('Ctrl Pts',(-5.08594588155711,-5.18584773014426,
-46.4819399043743));
#22399=CARTESIAN_POINT('Ctrl Pts',(-4.23345128165796,-6.021919596758,-46.4426817024853));
#22400=CARTESIAN_POINT('Ctrl Pts',(-3.17043868090825,-6.64333831627446,
-46.4034235005962));
#22401=CARTESIAN_POINT('Ctrl Pts',(-2.02366243310959,-6.97600548798374,
-46.3641652987072));
#22402=CARTESIAN_POINT('Ctrl Pts',(-0.876886185310941,-7.30867265969301,
-46.3249070968182));
#22403=CARTESIAN_POINT('Ctrl Pts',(0.353653709536664,-7.35258828359512,
-46.2856488949291));
#22404=CARTESIAN_POINT('Ctrl Pts',(1.52122682474423,-7.10251583237715,-46.2463906930401));
#22405=CARTESIAN_POINT('Ctrl Pts',(2.68879993995179,-6.85244338115917,-46.2071324911511));
#22406=CARTESIAN_POINT('Ctrl Pts',(3.79340627551931,-6.30838285482113,-46.167874289262));
#22407=CARTESIAN_POINT('Ctrl Pts',(4.70333181059907,-5.53520840479315,-46.128616087373));
#22408=CARTESIAN_POINT('Ctrl Pts',(5.61325734567882,-4.76203395476518,-46.0893578854839));
#22409=CARTESIAN_POINT('Ctrl Pts',(6.3285020802708,-3.75974558104729,-46.0500996835949));
#22410=CARTESIAN_POINT('Ctrl Pts',(6.76377973869342,-2.64785684107879,-46.0108414817058));
#22411=CARTESIAN_POINT('Ctrl Pts',(7.19905739711604,-1.53596810111027,-45.9715832798168));
#22412=CARTESIAN_POINT('Ctrl Pts',(7.35436797936928,-0.314478994891145,
-45.9323250779277));
#22413=CARTESIAN_POINT('Ctrl Pts',(7.21119214461735,0.870959274325189,-45.8930668760387));
#22414=CARTESIAN_POINT('Ctrl Pts',(7.06801630986543,2.05639754354152,-45.8538086741497));
#22415=CARTESIAN_POINT('Ctrl Pts',(6.62635405810834,3.20578497575507,-45.8145504722606));
#22416=CARTESIAN_POINT('Ctrl Pts',(5.93886950080655,4.18206782069874,-45.7752922703716));
#22417=CARTESIAN_POINT('Ctrl Pts',(5.25138494350475,5.15835066564242,-45.7360340684826));
#22418=CARTESIAN_POINT('Ctrl Pts',(4.31807808065826,5.96152892331622,-45.6967758665935));
#22419=CARTESIAN_POINT('Ctrl Pts',(3.25023706632267,6.49583106437886,-45.6575176647045));
#22420=CARTESIAN_POINT('Ctrl Pts',(2.1823960519871,7.03013320544148,-45.6182594628154));
#22421=CARTESIAN_POINT('Ctrl Pts',(0.980020886162445,7.29555922989294,-45.5790012609263));
#22422=CARTESIAN_POINT('Ctrl Pts',(-0.213516387111539,7.26045955548486,
-45.5397430590373));
#22423=CARTESIAN_POINT('Ctrl Pts',(-1.40705366038551,7.22535988107679,-45.5004848571483));
#22424=CARTESIAN_POINT('Ctrl Pts',(-2.59175304110882,6.88973450780919,-45.4612266552593));
#22425=CARTESIAN_POINT('Ctrl Pts',(-3.62635015802862,6.29360363668561,-45.4219684533702));
#22426=CARTESIAN_POINT('Ctrl Pts',(-4.66094727494843,5.69747276556203,-45.3827102514812));
#22427=CARTESIAN_POINT('Ctrl Pts',(-5.54544212806474,4.84083639658247,-45.3434520495921));
#22428=CARTESIAN_POINT('Ctrl Pts',(-6.1743669410577,3.82584044120064,-45.3041938477031));
#22429=CARTESIAN_POINT('Ctrl Pts',(-6.80329175405065,2.81084448581881,-45.264935645814));
#22430=CARTESIAN_POINT('Ctrl Pts',(-7.17664652692027,1.63748894403472,-45.225677443925));
#22431=CARTESIAN_POINT('Ctrl Pts',(-7.24991217904467,0.44568553991911,-45.1864192420359));
#22432=CARTESIAN_POINT('Ctrl Pts',(-7.25903039257842,0.29736067534915,-45.1815333963853));
#22433=CARTESIAN_POINT('Ctrl Pts',(-7.26350057604359,0.148750074933102,
-45.1766475507346));
#22434=CARTESIAN_POINT('Ctrl Pts',(-7.26337486577337,0.000131920041138065,
-45.1717617050839));
#22435=CARTESIAN_POINT('Origin',(0.,0.,-48.));
#22436=CARTESIAN_POINT('',(-7.26332735433935,-0.000142917180729311,-43.6717617050839));
#22437=CARTESIAN_POINT('',(-7.26276508042368,0.000167022802991385,-44.0782382949161));
#22438=CARTESIAN_POINT('',(-7.263,-8.89460970220723E-16,-48.));
#22439=CARTESIAN_POINT('Ctrl Pts',(-7.26276508042368,0.000167022802991385,
-44.0782382949161));
#22440=CARTESIAN_POINT('Ctrl Pts',(-7.26307825553427,0.357156309383415,
-44.0899715342723));
#22441=CARTESIAN_POINT('Ctrl Pts',(-7.23721492674339,0.714100615384112,
-44.1017047736286));
#22442=CARTESIAN_POINT('Ctrl Pts',(-7.18478680450647,1.0670994630721,-44.1134380129848));
#22443=CARTESIAN_POINT('Ctrl Pts',(-7.00936774545981,2.24819699363302,-44.1526962148739));
#22444=CARTESIAN_POINT('Ctrl Pts',(-6.53655524196093,3.3851250319695,-44.1919544167629));
#22445=CARTESIAN_POINT('Ctrl Pts',(-5.82272778302649,4.34231549464923,-44.2312126186519));
#22446=CARTESIAN_POINT('Ctrl Pts',(-5.10890032409204,5.29950595732896,-44.270470820541));
#22447=CARTESIAN_POINT('Ctrl Pts',(-4.15405790972205,6.07695884435194,-44.30972902243));
#22448=CARTESIAN_POINT('Ctrl Pts',(-3.07205660796225,6.58197013725935,-44.3489872243191));
#22449=CARTESIAN_POINT('Ctrl Pts',(-1.99005530620244,7.08698143016676,-44.3882454262081));
#22450=CARTESIAN_POINT('Ctrl Pts',(-0.780895117052828,7.3195511289586,-44.4275036280971));
#22451=CARTESIAN_POINT('Ctrl Pts',(0.411242864572872,7.25194746234682,-44.4667618299862));
#22452=CARTESIAN_POINT('Ctrl Pts',(1.60338084619856,7.18434379573504,-44.5060200318752));
#22453=CARTESIAN_POINT('Ctrl Pts',(2.77849662030031,6.81656676371965,-44.5452782337643));
#22454=CARTESIAN_POINT('Ctrl Pts',(3.79646857149504,6.19247035325541,-44.5845364356533));
#22455=CARTESIAN_POINT('Ctrl Pts',(4.81444052268977,5.56837394279117,-44.6237946375423));
#22456=CARTESIAN_POINT('Ctrl Pts',(5.67526865097746,4.68795815387806,-44.6630528394314));
#22457=CARTESIAN_POINT('Ctrl Pts',(6.2763072166269,3.65620437240841,-44.7023110413205));
#22458=CARTESIAN_POINT('Ctrl Pts',(6.87734578227633,2.62445059093877,-44.7415692432095));
#22459=CARTESIAN_POINT('Ctrl Pts',(7.21859478528751,1.44135881691259,-44.7808274450985));
#22460=CARTESIAN_POINT('Ctrl Pts',(7.25936345918091,0.248001729448511,-44.8200856469876));
#22461=CARTESIAN_POINT('Ctrl Pts',(7.30013213307431,-0.945355358015584,
-44.8593438488766));
#22462=CARTESIAN_POINT('Ctrl Pts',(7.04042047784991,-2.14897775891758,-44.8986020507657));
#22463=CARTESIAN_POINT('Ctrl Pts',(6.51119669040129,-3.21934470804107,-44.9378602526547));
#22464=CARTESIAN_POINT('Ctrl Pts',(5.98197290295268,-4.28971165716457,-44.9771184545437));
#22465=CARTESIAN_POINT('Ctrl Pts',(5.18323698327985,-5.22682315450957,-45.0163766564328));
#22466=CARTESIAN_POINT('Ctrl Pts',(4.2102307533317,-5.91893737879056,-45.0556348583218));
#22467=CARTESIAN_POINT('Ctrl Pts',(3.23722452338356,-6.61105160307155,-45.0948930602109));
#22468=CARTESIAN_POINT('Ctrl Pts',(2.08994798316011,-7.05816855428853,-45.1341512620999));
#22469=CARTESIAN_POINT('Ctrl Pts',(0.905203178600487,-7.20697369883143,
-45.173409463989));
#22470=CARTESIAN_POINT('Ctrl Pts',(-0.279541625959134,-7.35577884337434,
-45.212667665878));
#22471=CARTESIAN_POINT('Ctrl Pts',(-1.50175469485492,-7.20627218124317,
-45.251925867767));
#22472=CARTESIAN_POINT('Ctrl Pts',(-2.61569849879883,-6.77628098988389,
-45.2911840696561));
#22473=CARTESIAN_POINT('Ctrl Pts',(-3.72964230274274,-6.34628979852462,
-45.3304422715451));
#22474=CARTESIAN_POINT('Ctrl Pts',(-4.73531684173477,-5.63581407793723,
-45.3697004734342));
#22475=CARTESIAN_POINT('Ctrl Pts',(-5.51280479011146,-4.72957144318576,
-45.4089586753232));
#22476=CARTESIAN_POINT('Ctrl Pts',(-6.29029273848814,-3.82332880843428,
-45.4482168772123));
#22477=CARTESIAN_POINT('Ctrl Pts',(-6.83959409624948,-2.72131925951872,
-45.4874750791013));
#22478=CARTESIAN_POINT('Ctrl Pts',(-7.09520979068029,-1.55494717485536,
-45.5267332809903));
#22479=CARTESIAN_POINT('Ctrl Pts',(-7.20699526282622,-1.04487108397895,
-45.5439016189656));
#22480=CARTESIAN_POINT('Ctrl Pts',(-7.26261409467365,-0.522485820931676,
-45.5610699569408));
#22481=CARTESIAN_POINT('Ctrl Pts',(-7.26244595120635,-6.5281985395238E-5,
-45.5782382949161));
#22482=CARTESIAN_POINT('Ctrl Pts',(-7.26337486577337,0.000131920041138065,
-45.1717617050839));
#22483=CARTESIAN_POINT('Ctrl Pts',(-7.26249048290506,-1.04540994285732,
-45.1373893488456));
#22484=CARTESIAN_POINT('Ctrl Pts',(-7.03414397040485,-2.09132569542317,
-45.1030169926072));
#22485=CARTESIAN_POINT('Ctrl Pts',(-6.5964883600218,-3.04075706370068,-45.0686446363688));
#22486=CARTESIAN_POINT('Ctrl Pts',(-6.09662235749536,-4.12514499675771,
-45.0293864344798));
#22487=CARTESIAN_POINT('Ctrl Pts',(-5.3237138210633,-5.08366959642465,-44.9901282325907));
#22488=CARTESIAN_POINT('Ctrl Pts',(-4.36992489768557,-5.80203572834054,
-44.9508700307017));
#22489=CARTESIAN_POINT('Ctrl Pts',(-3.41613597430784,-6.52040186025644,
-44.9116118288126));
#22490=CARTESIAN_POINT('Ctrl Pts',(-2.28146666398445,-6.9986095244213,-44.8723536269236));
#22491=CARTESIAN_POINT('Ctrl Pts',(-1.10121571786165,-7.17963690913996,
-44.8330954250346));
#22492=CARTESIAN_POINT('Ctrl Pts',(0.0790352282611506,-7.36066429385862,
-44.7938372231455));
#22493=CARTESIAN_POINT('Ctrl Pts',(1.30486781018336,-7.24451139913107,-44.7545790212565));
#22494=CARTESIAN_POINT('Ctrl Pts',(2.43011290537809,-6.84502837623527,-44.7153208193674));
#22495=CARTESIAN_POINT('Ctrl Pts',(3.55535800057282,-6.44554535333947,-44.6760626174784));
#22496=CARTESIAN_POINT('Ctrl Pts',(4.58001560904007,-5.76273220227542,-44.6368044155893));
#22497=CARTESIAN_POINT('Ctrl Pts',(5.38190485083829,-4.87800803411333,-44.5975462137003));
#22498=CARTESIAN_POINT('Ctrl Pts',(6.18379409263651,-3.99328386595124,-44.5582880118113));
#22499=CARTESIAN_POINT('Ctrl Pts',(6.7629149677657,-2.90664868069111,-44.5190298099222));
#22500=CARTESIAN_POINT('Ctrl Pts',(7.05021270365494,-1.74767360727724,-44.4797716080332));
#22501=CARTESIAN_POINT('Ctrl Pts',(7.33751043954418,-0.58869853386337,-44.4405134061441));
#22502=CARTESIAN_POINT('Ctrl Pts',(7.33298503619347,0.642616427704244,-44.4012552042551));
#22503=CARTESIAN_POINT('Ctrl Pts',(7.03717610581953,1.79944843216851,-44.361997002366));
#22504=CARTESIAN_POINT('Ctrl Pts',(6.74136717544558,2.95628043663279,-44.322738800477));
#22505=CARTESIAN_POINT('Ctrl Pts',(6.15427471804838,4.03862948399371,-44.283480598588));
#22506=CARTESIAN_POINT('Ctrl Pts',(5.34590404316654,4.91743552734621,-44.2442223966989));
#22507=CARTESIAN_POINT('Ctrl Pts',(4.53753336828468,5.79624157069871,-44.2049641948099));
#22508=CARTESIAN_POINT('Ctrl Pts',(3.50788447591818,6.47150461004279,-44.1657059929209));
#22509=CARTESIAN_POINT('Ctrl Pts',(2.37973341014317,6.86270581483713,-44.1264477910318));
#22510=CARTESIAN_POINT('Ctrl Pts',(1.25158234436817,7.25390701963147,-44.0871895891428));
#22511=CARTESIAN_POINT('Ctrl Pts',(0.0249291051846681,7.36104638987607,
-44.0479313872537));
#22512=CARTESIAN_POINT('Ctrl Pts',(-1.15395932914251,7.17134855316878,-44.0086731853647));
#22513=CARTESIAN_POINT('Ctrl Pts',(-2.33284776346969,6.98165071646149,-43.9694149834756));
#22514=CARTESIAN_POINT('Ctrl Pts',(-3.46397139294055,6.49511567280232,-43.9301567815866));
#22515=CARTESIAN_POINT('Ctrl Pts',(-4.41245425583934,5.76975819636112,-43.8908985796975));
#22516=CARTESIAN_POINT('Ctrl Pts',(-5.36093711873811,5.04440071991993,-43.8516403778085));
#22517=CARTESIAN_POINT('Ctrl Pts',(-6.12677921506481,4.08022081069672,-43.8123821759195));
#22518=CARTESIAN_POINT('Ctrl Pts',(-6.618661005051,2.9921879460636,-43.7731239740304));
#22519=CARTESIAN_POINT('Ctrl Pts',(-7.04199720731669,2.05577657603305,-43.7393365510482));
#22520=CARTESIAN_POINT('Ctrl Pts',(-7.26240774709746,1.02762584652013,-43.7055491280661));
#22521=CARTESIAN_POINT('Ctrl Pts',(-7.26332735433935,-0.000142917180729311,
-43.6717617050839));
#22522=CARTESIAN_POINT('Origin',(0.,0.,-48.));
#22523=CARTESIAN_POINT('',(-7.26249686403911,-9.76851341781633E-5,-42.1717617050839));
#22524=CARTESIAN_POINT('',(-7.26357703776439,4.20713134600785E-5,-42.5782382949161));
#22525=CARTESIAN_POINT('',(-7.263,-8.89460970220723E-16,-48.));
#22526=CARTESIAN_POINT('Ctrl Pts',(-7.26357703776439,4.20713134600785E-5,
-42.5782382949161));
#22527=CARTESIAN_POINT('Ctrl Pts',(-7.26359058067385,0.0419126988576804,
-42.5796149097148));
#22528=CARTESIAN_POINT('Ctrl Pts',(-7.26323593189466,0.0837830962705636,
-42.5809915245135));
#22529=CARTESIAN_POINT('Ctrl Pts',(-7.26251165209856,0.125647098779436,
-42.5823681393121));
#22530=CARTESIAN_POINT('Ctrl Pts',(-7.2418566929288,1.31952171348383,-42.6216263412012));
#22531=CARTESIAN_POINT('Ctrl Pts',(-6.92059109431216,2.50819553037637,-42.6608845430902));
#22532=CARTESIAN_POINT('Ctrl Pts',(-6.33702278780508,3.5499302637007,-42.7001427449793));
#22533=CARTESIAN_POINT('Ctrl Pts',(-5.75345448129799,4.59166499702504,-42.7394009468683));
#22534=CARTESIAN_POINT('Ctrl Pts',(-4.90758346690044,5.48646064678117,-42.7786591487574));
#22535=CARTESIAN_POINT('Ctrl Pts',(-3.90027198776768,6.12762116255026,-42.8179173506464));
#22536=CARTESIAN_POINT('Ctrl Pts',(-2.89296050863493,6.76878167831935,-42.8571755525354));
#22537=CARTESIAN_POINT('Ctrl Pts',(-1.72420856476698,7.1563070601014,-42.8964337544245));
#22538=CARTESIAN_POINT('Ctrl Pts',(-0.533378944040606,7.24398851409589,
-42.9356919563135));
#22539=CARTESIAN_POINT('Ctrl Pts',(0.657450676685749,7.33166996809038,-42.9749501582026));
#22540=CARTESIAN_POINT('Ctrl Pts',(1.87035797427052,7.11950749429731,-43.0142083600916));
#22541=CARTESIAN_POINT('Ctrl Pts',(2.96071504600573,6.63279949242055,-43.0534665619806));
#22542=CARTESIAN_POINT('Ctrl Pts',(4.05107211774098,6.14609149054378,-43.0927247638697));
#22543=CARTESIAN_POINT('Ctrl Pts',(5.01887896362666,5.38483796058329,-43.1319829657587));
#22544=CARTESIAN_POINT('Ctrl Pts',(5.74873362786153,4.43981129848928,-43.1712411676478));
#22545=CARTESIAN_POINT('Ctrl Pts',(6.47858829209638,3.49478463639531,-43.2104993695368));
#22546=CARTESIAN_POINT('Ctrl Pts',(6.97049077468044,2.3659848421678,-43.2497575714259));
#22547=CARTESIAN_POINT('Ctrl Pts',(7.16578628432451,1.18801078180539,-43.2890157733149));
#22548=CARTESIAN_POINT('Ctrl Pts',(7.36108179396858,0.0100367214429617,
-43.328273975204));
#22549=CARTESIAN_POINT('Ctrl Pts',(7.25977033067266,-1.21711160505437,-43.367532177093));
#22550=CARTESIAN_POINT('Ctrl Pts',(6.87393234319481,-2.34710818486907,-43.406790378982));
#22551=CARTESIAN_POINT('Ctrl Pts',(6.48809435571697,-3.47710476468377,-43.4460485808711));
#22552=CARTESIAN_POINT('Ctrl Pts',(5.8177298440572,-4.50994959781582,-43.4853067827601));
#22553=CARTESIAN_POINT('Ctrl Pts',(4.94277353493723,-5.32248555400794,-43.5245649846492));
#22554=CARTESIAN_POINT('Ctrl Pts',(4.06781722581725,-6.13502151020005,-43.5638231865382));
#22555=CARTESIAN_POINT('Ctrl Pts',(2.98826911923707,-6.72724858945223,-43.6030813884273));
#22556=CARTESIAN_POINT('Ctrl Pts',(1.83285527599125,-7.02854922637454,-43.6423395903163));
#22557=CARTESIAN_POINT('Ctrl Pts',(0.67744143274542,-7.32984986329684,-43.6815977922053));
#22558=CARTESIAN_POINT('Ctrl Pts',(-0.553838147166054,-7.34022405788928,
-43.7208559940944));
#22559=CARTESIAN_POINT('Ctrl Pts',(-1.71416483741916,-7.05843478403355,
-43.7601141959834));
#22560=CARTESIAN_POINT('Ctrl Pts',(-2.87449152767229,-6.77664551017782,
-43.7993723978725));
#22561=CARTESIAN_POINT('Ctrl Pts',(-3.96386532826705,-6.20269276787391,
-43.8386305997615));
#22562=CARTESIAN_POINT('Ctrl Pts',(-4.8523885558778,-5.40501507797021,-43.8778888016506));
#22563=CARTESIAN_POINT('Ctrl Pts',(-5.74091178348852,-4.60733738806652,
-43.9171470035396));
#22564=CARTESIAN_POINT('Ctrl Pts',(-6.42858443811523,-3.58593475056303,
-43.9564052054286));
#22565=CARTESIAN_POINT('Ctrl Pts',(-6.83340795813138,-2.46259992041862,
-43.9956634073177));
#22566=CARTESIAN_POINT('Ctrl Pts',(-7.11724042331498,-1.67500019287866,
-44.0231883698505));
#22567=CARTESIAN_POINT('Ctrl Pts',(-7.26203040409744,-0.837292815814653,
-44.0507133323833));
#22568=CARTESIAN_POINT('Ctrl Pts',(-7.26276508042368,0.000167022802991385,
-44.0782382949161));
#22569=CARTESIAN_POINT('Ctrl Pts',(-7.26332735433935,-0.000142917180729311,
-43.6717617050839));
#22570=CARTESIAN_POINT('Ctrl Pts',(-7.26347625494962,-0.166556782972505,
-43.666290926177));
#22571=CARTESIAN_POINT('Ctrl Pts',(-7.25787069293385,-0.332960634646776,
-43.6608201472702));
#22572=CARTESIAN_POINT('Ctrl Pts',(-7.24644034797737,-0.49896341304413,
-43.6553493683633));
#22573=CARTESIAN_POINT('Ctrl Pts',(-7.16441641727186,-1.69019608747572,
-43.6160911664742));
#22574=CARTESIAN_POINT('Ctrl Pts',(-6.78244707221516,-2.86077561629585,
-43.5768329645852));
#22575=CARTESIAN_POINT('Ctrl Pts',(-6.14607860095665,-3.87112128913753,
-43.5375747626962));
#22576=CARTESIAN_POINT('Ctrl Pts',(-5.50971012969813,-4.88146696197922,
-43.4983165608071));
#22577=CARTESIAN_POINT('Ctrl Pts',(-4.61894253223782,-5.73157877884247,
-43.4590583589181));
#22578=CARTESIAN_POINT('Ctrl Pts',(-3.5799915512606,-6.32008882036113,-43.419800157029));
#22579=CARTESIAN_POINT('Ctrl Pts',(-2.5410405702834,-6.90859886187978,-43.38054195514));
#22580=CARTESIAN_POINT('Ctrl Pts',(-1.3539062057893,-7.23550712805385,-43.3412837532509));
#22581=CARTESIAN_POINT('Ctrl Pts',(-0.160143178168928,-7.26183285175561,
-43.3020255513619));
#22582=CARTESIAN_POINT('Ctrl Pts',(1.03361984945147,-7.28815857545737,-43.2627673494729));
#22583=CARTESIAN_POINT('Ctrl Pts',(2.23401154019812,-7.01390175668682,-43.2235091475838));
#22584=CARTESIAN_POINT('Ctrl Pts',(3.29789636095449,-6.47176496766949,-43.1842509456948));
#22585=CARTESIAN_POINT('Ctrl Pts',(4.36178118171085,-5.92962817865217,-43.1449927438057));
#22586=CARTESIAN_POINT('Ctrl Pts',(5.28915913247692,-5.11961141938807,-43.1057345419167));
#22587=CARTESIAN_POINT('Ctrl Pts',(5.96944902678939,-4.13830164692163,-43.0664763400276));
#22588=CARTESIAN_POINT('Ctrl Pts',(6.64973892110183,-3.1569918744552,-43.0272181381386));
#22589=CARTESIAN_POINT('Ctrl Pts',(7.08294075896069,-2.00438908878645,-42.9879599362496));
#22590=CARTESIAN_POINT('Ctrl Pts',(7.21739925443971,-0.817930441030332,
-42.9487017343605));
#22591=CARTESIAN_POINT('Ctrl Pts',(7.35185774991875,0.368528206725825,-42.9094435324715));
#22592=CARTESIAN_POINT('Ctrl Pts',(7.18757290301792,1.58884271656934,-42.8701853305825));
#22593=CARTESIAN_POINT('Ctrl Pts',(6.7441341521892,2.6975019446937,-42.8309271286934));
#22594=CARTESIAN_POINT('Ctrl Pts',(6.30069540136048,3.80616117281805,-42.7916689268044));
#22595=CARTESIAN_POINT('Ctrl Pts',(5.57810274660387,4.80316511922327,-42.7524107249153));
#22596=CARTESIAN_POINT('Ctrl Pts',(4.66251863444579,5.56963034570489,-42.7131525230263));
#22597=CARTESIAN_POINT('Ctrl Pts',(3.74693452228772,6.33609557218649,-42.6738943211372));
#22598=CARTESIAN_POINT('Ctrl Pts',(2.63835895272819,6.87202207874449,-42.6346361192482));
#22599=CARTESIAN_POINT('Ctrl Pts',(1.46897924126767,7.11350561910762,-42.5953779173591));
#22600=CARTESIAN_POINT('Ctrl Pts',(0.299599529807162,7.35498915947074,-42.5561197154701));
#22601=CARTESIAN_POINT('Ctrl Pts',(-0.930584323554325,7.30202973363898,
-42.5168615135811));
#22602=CARTESIAN_POINT('Ctrl Pts',(-2.07488434768231,6.96094226007471,-42.477603311692));
#22603=CARTESIAN_POINT('Ctrl Pts',(-3.21918437181033,6.61985478651042,-42.438345109803));
#22604=CARTESIAN_POINT('Ctrl Pts',(-4.27760056670487,5.99063926521361,-42.3990869079139));
#22605=CARTESIAN_POINT('Ctrl Pts',(-5.12392665529544,5.14832378891459,-42.3598287060249));
#22606=CARTESIAN_POINT('Ctrl Pts',(-5.97025274388599,4.3060083126156,-42.3205705041358));
#22607=CARTESIAN_POINT('Ctrl Pts',(-6.60448872617259,3.25059288131442,-42.2813123022468));
#22608=CARTESIAN_POINT('Ctrl Pts',(-6.9510078661939,2.10792595896098,-42.2420541003578));
#22609=CARTESIAN_POINT('Ctrl Pts',(-7.15782376018353,1.4259385770681,-42.2186233019332));
#22610=CARTESIAN_POINT('Ctrl Pts',(-7.2621503245026,0.712870821985042,-42.1951925035086));
#22611=CARTESIAN_POINT('Ctrl Pts',(-7.26249686403911,-9.76851341781633E-5,
-42.1717617050839));
#22612=CARTESIAN_POINT('Origin',(0.,0.,-48.));
#22613=CARTESIAN_POINT('',(-7.26266111293989,0.000150415497278031,-40.6717617050839));
#22614=CARTESIAN_POINT('',(-7.26300930122575,-0.000177974604063658,-41.0782382949161));
#22615=CARTESIAN_POINT('',(-7.263,-8.89460970220723E-16,-48.));
#22616=CARTESIAN_POINT('Ctrl Pts',(-7.26300930122575,-0.000177974604063658,
-41.0782382949161));
#22617=CARTESIAN_POINT('Ctrl Pts',(-7.26209383406802,0.920961063102483,
-41.1085164870463));
#22618=CARTESIAN_POINT('Ctrl Pts',(-7.08613975434704,1.8424399406362,-41.1387946791764));
#22619=CARTESIAN_POINT('Ctrl Pts',(-6.74413418324784,2.69750195711643,-41.1690728713066));
#22620=CARTESIAN_POINT('Ctrl Pts',(-6.30069543037697,3.80616119034647,-41.2083310731957));
#22621=CARTESIAN_POINT('Ctrl Pts',(-5.57810277229263,4.80316514134317,-41.2475892750847));
#22622=CARTESIAN_POINT('Ctrl Pts',(-4.66251865591803,5.56963037135458,-41.2868474769738));
#22623=CARTESIAN_POINT('Ctrl Pts',(-3.74693453954343,6.33609560136598,-41.3261056788628));
#22624=CARTESIAN_POINT('Ctrl Pts',(-2.63835896487857,6.8720221103921,-41.3653638807518));
#22625=CARTESIAN_POINT('Ctrl Pts',(-1.46897924803272,7.11350565186732,-41.4046220826409));
#22626=CARTESIAN_POINT('Ctrl Pts',(-0.299599531186881,7.35498919334254,
-41.4438802845299));
#22627=CARTESIAN_POINT('Ctrl Pts',(0.930584327839943,7.30202976726688,-41.483138486419));
#22628=CARTESIAN_POINT('Ctrl Pts',(2.07488435723775,6.9609422921318,-41.522396688308));
#22629=CARTESIAN_POINT('Ctrl Pts',(3.21918438663557,6.61985481699672,-41.5616548901971));
#22630=CARTESIAN_POINT('Ctrl Pts',(4.27760058640437,5.99063929280222,-41.6009130920861));
#22631=CARTESIAN_POINT('Ctrl Pts',(5.1239266788925,5.14832381262414,-41.6401712939751));
#22632=CARTESIAN_POINT('Ctrl Pts',(5.97025277138064,4.30600833244604,-41.6794294958642));
#22633=CARTESIAN_POINT('Ctrl Pts',(6.6044887565881,3.25059289628436,-41.7186876977532));
#22634=CARTESIAN_POINT('Ctrl Pts',(6.95100789820523,2.10792596866861,-41.7579458996423));
#22635=CARTESIAN_POINT('Ctrl Pts',(7.29752703982237,0.965259041052854,-41.7972041015313));
#22636=CARTESIAN_POINT('Ctrl Pts',(7.35632933784919,-0.264659378016966,
-41.8364623034203));
#22637=CARTESIAN_POINT('Ctrl Pts',(7.12040316571293,-1.4351729679744,-41.8757205053094));
#22638=CARTESIAN_POINT('Ctrl Pts',(6.88447699357666,-2.60568655793184,-41.9149787071984));
#22639=CARTESIAN_POINT('Ctrl Pts',(6.35382235127733,-3.71679531877686,-41.9542369090875));
#22640=CARTESIAN_POINT('Ctrl Pts',(5.59171486435599,-4.63600987553299,-41.9934951109765));
#22641=CARTESIAN_POINT('Ctrl Pts',(4.82960737743465,-5.5552244322891,-42.0327533128656));
#22642=CARTESIAN_POINT('Ctrl Pts',(3.83604704589131,-6.28254478495629,-42.0720115147546));
#22643=CARTESIAN_POINT('Ctrl Pts',(2.72950668891924,-6.73124475304859,-42.1112697166436));
#22644=CARTESIAN_POINT('Ctrl Pts',(1.62296633194719,-7.17994472114088,-42.1505279185327));
#22645=CARTESIAN_POINT('Ctrl Pts',(0.403445949546412,-7.35002430465829,
-42.1897861204217));
#22646=CARTESIAN_POINT('Ctrl Pts',(-0.783638006780596,-7.22120309675805,
-42.2290443223108));
#22647=CARTESIAN_POINT('Ctrl Pts',(-1.9707219631076,-7.09238188885781,-42.2683025241998));
#22648=CARTESIAN_POINT('Ctrl Pts',(-3.12536949336084,-6.66465988953992,
-42.3075607260888));
#22649=CARTESIAN_POINT('Ctrl Pts',(-4.10989962967079,-5.98903896500356,
-42.3468189279779));
#22650=CARTESIAN_POINT('Ctrl Pts',(-5.09442976598076,-5.31341804046719,
-42.3860771298669));
#22651=CARTESIAN_POINT('Ctrl Pts',(-5.90884250834743,-4.38989819071233,
-42.425335331756));
#22652=CARTESIAN_POINT('Ctrl Pts',(-6.45602671966932,-3.32860055957678,
-42.4645935336451));
#22653=CARTESIAN_POINT('Ctrl Pts',(-6.98402355493559,-2.30451803138863,
-42.5024751207354));
#22654=CARTESIAN_POINT('Ctrl Pts',(-7.26320436495528,-1.15215084812863,
-42.5403567078257));
#22655=CARTESIAN_POINT('Ctrl Pts',(-7.26357703776439,4.20713134600785E-5,
-42.5782382949161));
#22656=CARTESIAN_POINT('Ctrl Pts',(-7.26249686403911,-9.76851341781633E-5,
-42.1717617050839));
#22657=CARTESIAN_POINT('Ctrl Pts',(-7.26273095000414,-0.481704842309011,
-42.1559343016195));
#22658=CARTESIAN_POINT('Ctrl Pts',(-7.2155195294283,-0.963266713190378,
-42.1401068981551));
#22659=CARTESIAN_POINT('Ctrl Pts',(-7.12040313292146,-1.43517296136506,
-42.1242794946906));
#22660=CARTESIAN_POINT('Ctrl Pts',(-6.88447696187169,-2.60568654593194,
-42.0850212928016));
#22661=CARTESIAN_POINT('Ctrl Pts',(-6.35382232201616,-3.71679530166001,
-42.0457630909126));
#22662=CARTESIAN_POINT('Ctrl Pts',(-5.59171483860454,-4.63600985418288,
-42.0065048890235));
#22663=CARTESIAN_POINT('Ctrl Pts',(-4.82960735519293,-5.55522440670574,
-41.9672466871345));
#22664=CARTESIAN_POINT('Ctrl Pts',(-3.83604702822523,-6.2825447560234,-41.9279884852454));
#22665=CARTESIAN_POINT('Ctrl Pts',(-2.72950667634911,-6.7312447220493,-41.8887302833564));
#22666=CARTESIAN_POINT('Ctrl Pts',(-1.62296632447299,-7.17994468807521,
-41.8494720814673));
#22667=CARTESIAN_POINT('Ctrl Pts',(-0.403445947688449,-7.35002427080935,
-41.8102138795783));
#22668=CARTESIAN_POINT('Ctrl Pts',(0.783638003171704,-7.22120306350237,
-41.7709556776892));
#22669=CARTESIAN_POINT('Ctrl Pts',(1.97072195403187,-7.09238185619539,-41.7316974758002));
#22670=CARTESIAN_POINT('Ctrl Pts',(3.12536947896766,-6.66465985884728,-41.6924392739112));
#22671=CARTESIAN_POINT('Ctrl Pts',(4.10989961074358,-5.98903893742233,-41.6531810720221));
#22672=CARTESIAN_POINT('Ctrl Pts',(5.0944297425195,-5.31341801599738,-41.6139228701331));
#22673=CARTESIAN_POINT('Ctrl Pts',(5.90884248113557,-4.38989817049558,-41.5746646682441));
#22674=CARTESIAN_POINT('Ctrl Pts',(6.45602668993751,-3.3286005442476,-41.535406466355));
#22675=CARTESIAN_POINT('Ctrl Pts',(7.00321089873946,-2.26730291799962,-41.496148264466));
#22676=CARTESIAN_POINT('Ctrl Pts',(7.28316657772729,-1.06822751100545,-41.4568900625769));
#22677=CARTESIAN_POINT('Ctrl Pts',(7.26251161865265,0.12564709820083,-41.4176318606879));
#22678=CARTESIAN_POINT('Ctrl Pts',(7.241856659578,1.31952170740711,-41.3783736587988));
#22679=CARTESIAN_POINT('Ctrl Pts',(6.92059106244087,2.50819551882549,-41.3391154569098));
#22680=CARTESIAN_POINT('Ctrl Pts',(6.33702275862127,3.54993024735234,-41.2998572550207));
#22681=CARTESIAN_POINT('Ctrl Pts',(5.75345445480167,4.59166497587919,-41.2605990531317));
#22682=CARTESIAN_POINT('Ctrl Pts',(4.90758344429959,5.48646062151451,-41.2213408512427));
#22683=CARTESIAN_POINT('Ctrl Pts',(3.9002719698058,6.12762113433086,-41.1820826493536));
#22684=CARTESIAN_POINT('Ctrl Pts',(2.89296049531201,6.76878164714721,-41.1428244474646));
#22685=CARTESIAN_POINT('Ctrl Pts',(1.72420855682651,7.15630702714459,-41.1035662455755));
#22686=CARTESIAN_POINT('Ctrl Pts',(0.533378941584264,7.24398848073528,-41.0643080436865));
#22687=CARTESIAN_POINT('Ctrl Pts',(-0.657450673658001,7.33166993432597,
-41.0250498417974));
#22688=CARTESIAN_POINT('Ctrl Pts',(-1.87035796565701,7.11950746150997,-40.9857916399084));
#22689=CARTESIAN_POINT('Ctrl Pts',(-2.96071503237084,6.63279946187463,-40.9465334380193));
#22690=CARTESIAN_POINT('Ctrl Pts',(-4.05107209908466,6.14609146223928,-40.9072752361303));
#22691=CARTESIAN_POINT('Ctrl Pts',(-5.0188789405133,5.38483793578459,-40.8680170342413));
#22692=CARTESIAN_POINT('Ctrl Pts',(-5.74873360138698,4.43981127804272,-40.8287588323522));
#22693=CARTESIAN_POINT('Ctrl Pts',(-6.47858826226065,3.49478462030085,-40.7895006304632));
#22694=CARTESIAN_POINT('Ctrl Pts',(-6.97049074257936,2.3659848312718,-40.7502424285742));
#22695=CARTESIAN_POINT('Ctrl Pts',(-7.16578625132404,1.18801077633428,-40.7109842266851));
#22696=CARTESIAN_POINT('Ctrl Pts',(-7.2308255886834,0.795709629973483,-40.697910052818));
#22697=CARTESIAN_POINT('Ctrl Pts',(-7.26296847415723,0.397954603469952,
-40.684835878951));
#22698=CARTESIAN_POINT('Ctrl Pts',(-7.26266111293989,0.000150415497278031,
-40.6717617050839));
#22699=CARTESIAN_POINT('Origin',(0.,0.,-48.));
#22700=CARTESIAN_POINT('',(-7.26352054254983,8.04286712641332E-5,-39.1717617050839));
#22701=CARTESIAN_POINT('',(-7.26240901964853,-7.93431878864936E-6,-39.5782382949161));
#22702=CARTESIAN_POINT('',(-7.263,-8.89460970220723E-16,-48.));
#22703=CARTESIAN_POINT('Ctrl Pts',(-7.26240901964853,-7.93431878864936E-6,
-39.5782382949161));
#22704=CARTESIAN_POINT('Ctrl Pts',(-7.26238545910871,0.606200286890817,
-39.5981598624887));
#22705=CARTESIAN_POINT('Ctrl Pts',(-7.18728432807362,1.2124142426494,-39.6180814300613));
#22706=CARTESIAN_POINT('Ctrl Pts',(-7.03717613822771,1.79944844045549,-39.638002997634));
#22707=CARTESIAN_POINT('Ctrl Pts',(-6.74136720649147,2.95628045024729,-39.677261199523));
#22708=CARTESIAN_POINT('Ctrl Pts',(-6.15427474639056,4.03862950259272,-39.716519401412));
#22709=CARTESIAN_POINT('Ctrl Pts',(-5.34590406778595,4.91743554999236,-39.7557776033011));
#22710=CARTESIAN_POINT('Ctrl Pts',(-4.53753338918133,5.79624159739201,-39.7950358051901));
#22711=CARTESIAN_POINT('Ctrl Pts',(-3.507884492073,6.47150463984588,-39.8342940070792));
#22712=CARTESIAN_POINT('Ctrl Pts',(-2.37973342110255,6.86270584644181,-39.8735522089682));
#22713=CARTESIAN_POINT('Ctrl Pts',(-1.2515823501321,7.25390705303775,-39.9128104108573));
#22714=CARTESIAN_POINT('Ctrl Pts',(-0.0249291052995126,7.36104642377576,
-39.9520686127463));
#22715=CARTESIAN_POINT('Ctrl Pts',(1.15395933445678,7.17134858619487,-39.9913268146353));
#22716=CARTESIAN_POINT('Ctrl Pts',(2.33284777421308,6.98165074861397,-40.0305850165244));
#22717=CARTESIAN_POINT('Ctrl Pts',(3.46397140889309,6.49511570271417,-40.0698432184134));
#22718=CARTESIAN_POINT('Ctrl Pts',(4.41245427615991,5.7697582229325,-40.1091014203025));
#22719=CARTESIAN_POINT('Ctrl Pts',(5.36093714342672,5.04440074315083,-40.1483596221915));
#22720=CARTESIAN_POINT('Ctrl Pts',(6.12677924328035,4.0802208294873,-40.1876178240806));
#22721=CARTESIAN_POINT('Ctrl Pts',(6.6186610355318,2.99218795984346,-40.2268760259696));
#22722=CARTESIAN_POINT('Ctrl Pts',(7.11054282778324,1.90415509019964,-40.2661342278586));
#22723=CARTESIAN_POINT('Ctrl Pts',(7.32846431243252,0.692269264575519,-40.3053924297477));
#22724=CARTESIAN_POINT('Ctrl Pts',(7.24644038134927,-0.498963415342015,
-40.3446506316367));
#22725=CARTESIAN_POINT('Ctrl Pts',(7.16441645026602,-1.69019609525955,-40.3839088335258));
#22726=CARTESIAN_POINT('Ctrl Pts',(6.78244710345024,-2.8607756294705,-40.4231670354148));
#22727=CARTESIAN_POINT('Ctrl Pts',(6.14607862926109,-3.8711213069651,-40.4624252373038));
#22728=CARTESIAN_POINT('Ctrl Pts',(5.50971015507191,-4.88146698445973,-40.5016834391929));
#22729=CARTESIAN_POINT('Ctrl Pts',(4.61894255350935,-5.73157880523801,-40.5409416410819));
#22730=CARTESIAN_POINT('Ctrl Pts',(3.57999156774745,-6.32008884946693,-40.580199842971));
#22731=CARTESIAN_POINT('Ctrl Pts',(2.54104058198559,-6.90859889369583,-40.61945804486));
#22732=CARTESIAN_POINT('Ctrl Pts',(1.3539062120244,-7.2355071613754,-40.6587162467491));
#22733=CARTESIAN_POINT('Ctrl Pts',(0.160143178906415,-7.26183288519839,
-40.6979744486381));
#22734=CARTESIAN_POINT('Ctrl Pts',(-1.03361985421157,-7.28815860902139,
-40.7372326505271));
#22735=CARTESIAN_POINT('Ctrl Pts',(-2.23401155048636,-7.01390178898781,
-40.7764908524162));
#22736=CARTESIAN_POINT('Ctrl Pts',(-3.2978963761422,-6.47176499747381,-40.8157490543052));
#22737=CARTESIAN_POINT('Ctrl Pts',(-4.36178120179806,-5.9296282059598,-40.8550072561943));
#22738=CARTESIAN_POINT('Ctrl Pts',(-5.28915915683497,-5.11961144296535,
-40.8942654580833));
#22739=CARTESIAN_POINT('Ctrl Pts',(-5.96944905428036,-4.1383016659797,-40.9335236599724));
#22740=CARTESIAN_POINT('Ctrl Pts',(-6.64973895172576,-3.15699188899405,
-40.9727818618614));
#22741=CARTESIAN_POINT('Ctrl Pts',(-7.08294079157965,-2.00438909801718,
-41.0120400637505));
#22742=CARTESIAN_POINT('Ctrl Pts',(-7.21739928767788,-0.817930444797065,
-41.0512982656395));
#22743=CARTESIAN_POINT('Ctrl Pts',(-7.24815562772976,-0.546537213020399,
-41.0602782753984));
#22744=CARTESIAN_POINT('Ctrl Pts',(-7.26328081360585,-0.273372540260897,
-41.0692582851572));
#22745=CARTESIAN_POINT('Ctrl Pts',(-7.26300930122575,-0.000177974604063658,
-41.0782382949161));
#22746=CARTESIAN_POINT('Ctrl Pts',(-7.26266111293989,0.000150415497278031,
-40.6717617050839));
#22747=CARTESIAN_POINT('Ctrl Pts',(-7.26204555169606,-0.796543594468861,
-40.6455776770619));
#22748=CARTESIAN_POINT('Ctrl Pts',(-7.13127452650012,-1.59343478733736,
-40.61939364904));
#22749=CARTESIAN_POINT('Ctrl Pts',(-6.8739323115384,-2.34710817406001,-40.593209621018));
#22750=CARTESIAN_POINT('Ctrl Pts',(-6.48809432583744,-3.47710474867077,
-40.5539514191289));
#22751=CARTESIAN_POINT('Ctrl Pts',(-5.81772981726488,-4.50994957704628,
-40.5146932172399));
#22752=CARTESIAN_POINT('Ctrl Pts',(-4.94277351217432,-5.32248552949644,
-40.4754350153508));
#22753=CARTESIAN_POINT('Ctrl Pts',(-4.06781720708377,-6.13502148194658,
-40.4361768134618));
#22754=CARTESIAN_POINT('Ctrl Pts',(-2.98826910547521,-6.72724855847138,
-40.3969186115728));
#22755=CARTESIAN_POINT('Ctrl Pts',(-1.8328552675504,-7.0285491940061,-40.3576604096837));
#22756=CARTESIAN_POINT('Ctrl Pts',(-0.677441429625552,-7.32984982954083,
-40.3184022077947));
#22757=CARTESIAN_POINT('Ctrl Pts',(0.55383814461556,-7.34022402408548,-40.2791440059056));
#22758=CARTESIAN_POINT('Ctrl Pts',(1.71416482952506,-7.05843475152745,-40.2398858040166));
#22759=CARTESIAN_POINT('Ctrl Pts',(2.87449151443453,-6.77664547896942,-40.2006276021276));
#22760=CARTESIAN_POINT('Ctrl Pts',(3.96386531001239,-6.20269273930873,-40.1613694002385));
#22761=CARTESIAN_POINT('Ctrl Pts',(4.85238853353121,-5.40501505307857,-40.1221111983495));
#22762=CARTESIAN_POINT('Ctrl Pts',(5.74091175705003,-4.6073373668484,-40.0828529964604));
#22763=CARTESIAN_POINT('Ctrl Pts',(6.42858440850981,-3.58593473404876,-40.0435947945714));
#22764=CARTESIAN_POINT('Ctrl Pts',(6.83340792666162,-2.46259990907762,-40.0043365926823));
#22765=CARTESIAN_POINT('Ctrl Pts',(7.23823144481344,-1.33926508410647,-39.9650783907933));
#22766=CARTESIAN_POINT('Ctrl Pts',(7.3602058296573,-0.11399806696383,-39.9258201889043));
#22767=CARTESIAN_POINT('Ctrl Pts',(7.1847867714185,1.06709945815779,-39.8865619870152));
#22768=CARTESIAN_POINT('Ctrl Pts',(7.0093677131797,2.24819698327945,-39.8473037851262));
#22769=CARTESIAN_POINT('Ctrl Pts',(6.53655521185824,3.38512501638008,-39.8080455832371));
#22770=CARTESIAN_POINT('Ctrl Pts',(5.82272775621115,4.34231547465169,-39.7687873813481));
#22771=CARTESIAN_POINT('Ctrl Pts',(5.10890030056408,5.29950593292327,-39.729529179459));
#22772=CARTESIAN_POINT('Ctrl Pts',(4.15405789059141,6.07695881636586,-39.69027097757));
#22773=CARTESIAN_POINT('Ctrl Pts',(3.07205659381453,6.58197010694754,-39.651012775681));
#22774=CARTESIAN_POINT('Ctrl Pts',(1.99005529703764,7.08698139752923,-39.6117545737919));
#22775=CARTESIAN_POINT('Ctrl Pts',(0.780895113456552,7.31955109525001,-39.5724963719029));
#22776=CARTESIAN_POINT('Ctrl Pts',(-0.411242862679016,7.25194742894955,
-39.5332381700138));
#22777=CARTESIAN_POINT('Ctrl Pts',(-1.60338083881458,7.1843437626491,-39.4939799681248));
#22778=CARTESIAN_POINT('Ctrl Pts',(-2.77849660750463,6.81656673232741,-39.4547217662357));
#22779=CARTESIAN_POINT('Ctrl Pts',(-3.79646855401131,6.1924703247373,-39.4154635643467));
#22780=CARTESIAN_POINT('Ctrl Pts',(-4.81444050051797,5.56837391714719,-39.3762053624577));
#22781=CARTESIAN_POINT('Ctrl Pts',(-5.67526862484128,4.68795813228867,-39.3369471605686));
#22782=CARTESIAN_POINT('Ctrl Pts',(-6.27630718772275,3.65620435557054,-39.2976889586796));
#22783=CARTESIAN_POINT('Ctrl Pts',(-6.87734575060422,2.62445057885241,-39.2584307567905));
#22784=CARTESIAN_POINT('Ctrl Pts',(-7.21859475204387,1.44135881027467,-39.2191725549015));
#22785=CARTESIAN_POINT('Ctrl Pts',(-7.2593634257495,0.248001728306349,-39.1799143530124));
#22786=CARTESIAN_POINT('Ctrl Pts',(-7.2621855336339,0.165394615447164,-39.1771968037029));
#22787=CARTESIAN_POINT('Ctrl Pts',(-7.26356781521829,0.0827383137831455,
-39.1744792543934));
#22788=CARTESIAN_POINT('Ctrl Pts',(-7.26352054254983,8.04286712641332E-5,
-39.1717617050839));
#22789=CARTESIAN_POINT('Origin',(0.,0.,-48.));
#22790=CARTESIAN_POINT('',(-7.26313420453275,-0.000171068891272981,-37.6717617050839));
#22791=CARTESIAN_POINT('',(-7.26295522622064,0.000178426625192518,-38.0782382949161));
#22792=CARTESIAN_POINT('',(-7.263,-8.89460970220723E-16,-48.));
#22793=CARTESIAN_POINT('Ctrl Pts',(-7.26295522622064,0.000178426625192518,
-38.0782382949161));
#22794=CARTESIAN_POINT('Ctrl Pts',(-7.26324087904769,0.291174376834878,
-38.0878032379312));
#22795=CARTESIAN_POINT('Ctrl Pts',(-7.24607581082464,0.582136841251713,
-38.0973681809462));
#22796=CARTESIAN_POINT('Ctrl Pts',(-7.21119217782702,0.870959278336532,
-38.1069331239613));
#22797=CARTESIAN_POINT('Ctrl Pts',(-7.06801634241581,2.05639755301244,-38.1461913258504));
#22798=CARTESIAN_POINT('Ctrl Pts',(-6.62635408862456,3.20578499051862,-38.1854495277394));
#22799=CARTESIAN_POINT('Ctrl Pts',(-5.93886952815666,4.1820678399582,-38.2247077296284));
#22800=CARTESIAN_POINT('Ctrl Pts',(-5.25138496768876,5.15835068939778,-38.2639659315175));
#22801=CARTESIAN_POINT('Ctrl Pts',(-4.31807810054421,5.96152895077076,-38.3032241334065));
#22802=CARTESIAN_POINT('Ctrl Pts',(-3.25023708129094,6.49583109429408,-38.3424823352956));
#22803=CARTESIAN_POINT('Ctrl Pts',(-2.18239606203769,7.03013323781739,-38.3817405371846));
#22804=CARTESIAN_POINT('Ctrl Pts',(-0.980020890675717,7.29555926349104,
-38.4209987390737));
#22805=CARTESIAN_POINT('Ctrl Pts',(0.213516388094846,7.26045958892129,-38.4602569409627));
#22806=CARTESIAN_POINT('Ctrl Pts',(1.40705366686543,7.22535991435153,-38.4995151428517));
#22807=CARTESIAN_POINT('Ctrl Pts',(2.5917530530446,6.88973453953835,-38.5387733447408));
#22808=CARTESIAN_POINT('Ctrl Pts',(3.62635017472901,6.29360366566943,-38.5780315466298));
#22809=CARTESIAN_POINT('Ctrl Pts',(4.66094729641343,5.69747279180051,-38.6172897485189));
#22810=CARTESIAN_POINT('Ctrl Pts',(5.54544215360309,4.84083641887585,-38.6565479504079));
#22811=CARTESIAN_POINT('Ctrl Pts',(6.17436696949242,3.82584045881966,-38.6958061522969));
#22812=CARTESIAN_POINT('Ctrl Pts',(6.80329178538175,2.81084449876349,-38.735064354186));
#22813=CARTESIAN_POINT('Ctrl Pts',(7.17664655997076,1.63748895157579,-38.774322556075));
#22814=CARTESIAN_POINT('Ctrl Pts',(7.24991221243256,0.445685541971607,-38.8135807579641));
#22815=CARTESIAN_POINT('Ctrl Pts',(7.32317786489436,-0.74611786763258,-38.8528389598531));
#22816=CARTESIAN_POINT('Ctrl Pts',(7.09635439522896,-1.95636913965326,-38.8920971617422));
#22817=CARTESIAN_POINT('Ctrl Pts',(6.5964883904005,-3.0407570777042,-38.9313553636312));
#22818=CARTESIAN_POINT('Ctrl Pts',(6.09662238557205,-4.12514501575514,-38.9706135655202));
#22819=CARTESIAN_POINT('Ctrl Pts',(5.32371384558054,-5.08366961983634,-39.0098717674093));
#22820=CARTESIAN_POINT('Ctrl Pts',(4.36992491781035,-5.80203575506052,-39.0491299692983));
#22821=CARTESIAN_POINT('Ctrl Pts',(3.41613599004017,-6.52040189028469,-39.0883881711874));
#22822=CARTESIAN_POINT('Ctrl Pts',(2.28146667449132,-6.99860955665184,-39.1276463730764));
#22823=CARTESIAN_POINT('Ctrl Pts',(1.10121572293315,-7.1796369422042,-39.1669045749655));
#22824=CARTESIAN_POINT('Ctrl Pts',(-0.0790352286250597,-7.36066432775656,
-39.2061627768545));
#22825=CARTESIAN_POINT('Ctrl Pts',(-1.30486781619259,-7.24451143249411,
-39.2454209787435));
#22826=CARTESIAN_POINT('Ctrl Pts',(-2.43011291656941,-6.84502840775857,
-39.2846791806326));
#22827=CARTESIAN_POINT('Ctrl Pts',(-3.55535801694622,-6.44554538302304,
-39.3239373825216));
#22828=CARTESIAN_POINT('Ctrl Pts',(-4.58001563013233,-5.76273222881443,
-39.3631955844107));
#22829=CARTESIAN_POINT('Ctrl Pts',(-5.38190487562348,-4.87800805657794,
-39.4024537862997));
#22830=CARTESIAN_POINT('Ctrl Pts',(-6.18379412111464,-3.99328388434143,
-39.4417119881888));
#22831=CARTESIAN_POINT('Ctrl Pts',(-6.76291499891085,-2.90664869407702,
-39.4809701900778));
#22832=CARTESIAN_POINT('Ctrl Pts',(-7.05021273612318,-1.74767361532571,
-39.5202283919668));
#22833=CARTESIAN_POINT('Ctrl Pts',(-7.19172128763834,-1.17682023434321,
-39.5395650262832));
#22834=CARTESIAN_POINT('Ctrl Pts',(-7.26243188840829,-0.588416785700682,
-39.5589016605997));
#22835=CARTESIAN_POINT('Ctrl Pts',(-7.26240901964853,-7.93431878864936E-6,
-39.5782382949161));
#22836=CARTESIAN_POINT('Ctrl Pts',(-7.26352054254983,8.04286712641332E-5,
-39.1717617050839));
#22837=CARTESIAN_POINT('Ctrl Pts',(-7.2628849058206,-1.11135223320081,-39.1352210525044));
#22838=CARTESIAN_POINT('Ctrl Pts',(-7.00378627314357,-2.22307118198899,
-39.0986803999249));
#22839=CARTESIAN_POINT('Ctrl Pts',(-6.51119666041538,-3.21934469321509,
-39.0621397473453));
#22840=CARTESIAN_POINT('Ctrl Pts',(-5.98197287540399,-4.28971163740927,
-39.0228815454563));
#22841=CARTESIAN_POINT('Ctrl Pts',(-5.18323695940958,-5.22682313043868,
-38.9836233435672));
#22842=CARTESIAN_POINT('Ctrl Pts',(-4.21023073394239,-5.91893735153225,
-38.9443651416782));
#22843=CARTESIAN_POINT('Ctrl Pts',(-3.23722450847519,-6.61105157262582,
-38.9051069397891));
#22844=CARTESIAN_POINT('Ctrl Pts',(-2.08994797353521,-7.05816852178353,
-38.8658487379001));
#22845=CARTESIAN_POINT('Ctrl Pts',(-0.90520317443169,-7.20697366564122,
-38.8265905360111));
#22846=CARTESIAN_POINT('Ctrl Pts',(0.279541624671835,-7.3557788094989,-38.787332334122));
#22847=CARTESIAN_POINT('Ctrl Pts',(1.5017546879389,-7.20627214805655,-38.748074132233));
#22848=CARTESIAN_POINT('Ctrl Pts',(2.61569848675283,-6.77628095867734,-38.7088159303439));
#22849=CARTESIAN_POINT('Ctrl Pts',(3.72964228556675,-6.34628976929814,-38.6695577284549));
#22850=CARTESIAN_POINT('Ctrl Pts',(4.73531681992753,-5.63581405198208,-38.6302995265658));
#22851=CARTESIAN_POINT('Ctrl Pts',(5.51280476472356,-4.72957142140441,-38.5910413246768));
#22852=CARTESIAN_POINT('Ctrl Pts',(6.29029270951958,-3.82332879082673,-38.5517831227878));
#22853=CARTESIAN_POINT('Ctrl Pts',(6.83959406475085,-2.72131924698744,-38.5125249208987));
#22854=CARTESIAN_POINT('Ctrl Pts',(7.09520975800467,-1.554947167695,-38.4732667190097));
#22855=CARTESIAN_POINT('Ctrl Pts',(7.35082545125849,-0.388575088402531,
-38.4340085171206));
#22856=CARTESIAN_POINT('Ctrl Pts',(7.31275548253484,0.842159526343091,-38.3947503152316));
#22857=CARTESIAN_POINT('Ctrl Pts',(6.98553934108194,1.99050303171896,-38.3554921133426));
#22858=CARTESIAN_POINT('Ctrl Pts',(6.65832319962904,3.13884653709483,-38.3162339114535));
#22859=CARTESIAN_POINT('Ctrl Pts',(6.04196088544689,4.20479893310094,-38.2769757095645));
#22860=CARTESIAN_POINT('Ctrl Pts',(5.20994786614568,5.06125532190715,-38.2377175076754));
#22861=CARTESIAN_POINT('Ctrl Pts',(4.37793484684449,5.91771171071335,-38.1984593057864));
#22862=CARTESIAN_POINT('Ctrl Pts',(3.33027112242425,6.56467209231964,-38.1592011038973));
#22863=CARTESIAN_POINT('Ctrl Pts',(2.1918808376328,6.92499246246351,-38.1199429020083));
#22864=CARTESIAN_POINT('Ctrl Pts',(1.05349055284132,7.28531283260738,-38.0806847001193));
#22865=CARTESIAN_POINT('Ctrl Pts',(-0.175626292321373,7.35899319128881,
-38.0414264982302));
#22866=CARTESIAN_POINT('Ctrl Pts',(-1.34890895684957,7.13724784608893,-38.0021682963412));
#22867=CARTESIAN_POINT('Ctrl Pts',(-2.52219162137778,6.91550250088904,-37.9629100944521));
#22868=CARTESIAN_POINT('Ctrl Pts',(-3.63964010527149,6.39833145180785,-37.9236518925631));
#22869=CARTESIAN_POINT('Ctrl Pts',(-4.56800908195572,5.64740252255931,-37.884393690674));
#22870=CARTESIAN_POINT('Ctrl Pts',(-5.4963780586399,4.89647359331081,-37.845135488785));
#22871=CARTESIAN_POINT('Ctrl Pts',(-6.23566752811461,3.911786783895,-37.805877286896));
#22872=CARTESIAN_POINT('Ctrl Pts',(-6.69772410140762,2.81075684662822,-37.7666190850069));
#22873=CARTESIAN_POINT('Ctrl Pts',(-7.06987118413825,1.92397132546851,-37.7349999583659));
#22874=CARTESIAN_POINT('Ctrl Pts',(-7.2621793435513,0.961714880272418,-37.7033808317249));
#22875=CARTESIAN_POINT('Ctrl Pts',(-7.26313420453275,-0.000171068891272981,
-37.6717617050839));
#22876=CARTESIAN_POINT('Origin',(0.,0.,-48.));
#22877=CARTESIAN_POINT('',(-7.26243100057087,-0.00011786593126363,-36.1717617050839));
#22878=CARTESIAN_POINT('',(-7.26359129981488,-2.41004779799603E-5,-36.5782382949161));
#22879=CARTESIAN_POINT('',(-7.263,-8.89460970220723E-16,-48.));
#22880=CARTESIAN_POINT('',(-5.46288453460435,-4.78623668048088,-36.));
#22881=CARTESIAN_POINT('Ctrl Pts',(-7.26243100057087,-0.00011786593126363,
-36.1717617050839));
#22882=CARTESIAN_POINT('Ctrl Pts',(-7.26254766902496,-0.547742115475237,
-36.1537660052783));
#22883=CARTESIAN_POINT('Ctrl Pts',(-7.2013797096861,-1.09531506383856,-36.1357703054727));
#22884=CARTESIAN_POINT('Ctrl Pts',(-7.07862623058799,-1.62865307118789,
-36.1177746056671));
#22885=CARTESIAN_POINT('Ctrl Pts',(-6.81083554075238,-2.79214720555352,
-36.0785164037781));
#22886=CARTESIAN_POINT('Ctrl Pts',(-6.24995421752147,-3.88789606644511,
-36.039258201889));
#22887=CARTESIAN_POINT('Ctrl Pts',(-5.46288453460428,-4.78623668048096,
-36.));
#22888=CARTESIAN_POINT('',(5.46288453460446,-4.78623668048075,-36.));
#22889=CARTESIAN_POINT('Origin',(0.,0.,-36.));
#22890=CARTESIAN_POINT('Ctrl Pts',(5.46328275624298,-4.78643223329959,-36.));
#22891=CARTESIAN_POINT('Ctrl Pts',(4.76265403019709,-5.58484238403501,-36.0349216092067));
#22892=CARTESIAN_POINT('Ctrl Pts',(3.88494973086336,-6.22857884933557,-36.0698432184135));
#22893=CARTESIAN_POINT('Ctrl Pts',(2.91187905542927,-6.65437827772981,-36.1047648276202));
#22894=CARTESIAN_POINT('Ctrl Pts',(1.81797170418512,-7.13305381141417,-36.1440230295092));
#22895=CARTESIAN_POINT('Ctrl Pts',(0.603542002707702,-7.33630434768437,
-36.1832812313982));
#22896=CARTESIAN_POINT('Ctrl Pts',(-0.586609857006575,-7.23987449212561,
-36.2225394332873));
#22897=CARTESIAN_POINT('Ctrl Pts',(-1.77676171672083,-7.14344463656685,
-36.2617976351763));
#22898=CARTESIAN_POINT('Ctrl Pts',(-2.94263573467192,-6.74733438917911,
-36.3010558370653));
#22899=CARTESIAN_POINT('Ctrl Pts',(-3.94520774032596,-6.0987858833362,-36.3403140389544));
#22900=CARTESIAN_POINT('Ctrl Pts',(-4.94777974598003,-5.45023737749328,
-36.3795722408435));
#22901=CARTESIAN_POINT('Ctrl Pts',(-5.78704973933708,-4.54925061319516,
-36.4188304427325));
#22902=CARTESIAN_POINT('Ctrl Pts',(-6.36294482586013,-3.50325511296896,
-36.4580886446215));
#22903=CARTESIAN_POINT('Ctrl Pts',(-6.93883991238317,-2.45725961274279,
-36.4973468465106));
#22904=CARTESIAN_POINT('Ctrl Pts',(-7.25136009207222,-1.26625537658855,
-36.5366050483996));
#22905=CARTESIAN_POINT('Ctrl Pts',(-7.26323914168565,-0.0722609137693696,
-36.5758632502886));
#22906=CARTESIAN_POINT('Ctrl Pts',(-7.26347869479477,-0.0481828018704033,
-36.5766549318311));
#22907=CARTESIAN_POINT('Ctrl Pts',(-7.26359598671164,-0.0241034739412912,
-36.5774466133736));
#22908=CARTESIAN_POINT('Ctrl Pts',(-7.26359129981488,-2.41004779799603E-5,
-36.5782382949161));
#22909=CARTESIAN_POINT('Origin',(0.,0.,-51.3123464956316));
#22910=CARTESIAN_POINT('',(-8.10164969819937,-0.000190818480503285,-37.1876535043684));
#22911=CARTESIAN_POINT('',(-8.10215956429164,-2.68828339804187E-5,-37.0623464956316));
#22912=CARTESIAN_POINT('',(-8.1015,-2.19835914433334E-13,-51.3123464956316));
#22913=CARTESIAN_POINT('',(2.10185380438477,7.82409821225381,-36.));
#22914=CARTESIAN_POINT('Ctrl Pts',(-8.10215956429164,-2.6882833979924E-5,
-37.0623464956316));
#22915=CARTESIAN_POINT('Ctrl Pts',(-8.10216479228202,-0.0268861757036945,
-37.0615548140891));
#22916=CARTESIAN_POINT('Ctrl Pts',(-8.09554616061823,-1.38565160926748,
-37.0215049306576));
#22917=CARTESIAN_POINT('Ctrl Pts',(-7.39131616610511,-4.06944920443886,
-36.942196845337));
#22918=CARTESIAN_POINT('Ctrl Pts',(-4.58282965177962,-7.08446129488128,
-36.8244222396699));
#22919=CARTESIAN_POINT('Ctrl Pts',(-0.681413560730255,-8.40998263697618,
-36.7066476340027));
#22920=CARTESIAN_POINT('Ctrl Pts',(3.38248657413956,-7.72983632570271,-36.5888730283357));
#22921=CARTESIAN_POINT('Ctrl Pts',(6.63976810478354,-5.20635617176029,-36.4710984226685));
#22922=CARTESIAN_POINT('Ctrl Pts',(8.31350431780115,-1.44107773576215,-36.3533238170014));
#22923=CARTESIAN_POINT('Ctrl Pts',(8.00479582109024,2.66750482517421,-36.2355492113343));
#22924=CARTESIAN_POINT('Ctrl Pts',(5.78674112666189,6.14069293294423,-36.1177746056671));
#22925=CARTESIAN_POINT('Ctrl Pts',(3.38848271769057,7.47846018434309,-36.039258201889));
#22926=CARTESIAN_POINT('Ctrl Pts',(2.10185380438477,7.82409821225381,-36.));
#22927=CARTESIAN_POINT('',(-2.10185380438507,7.82409821225373,-36.));
#22928=CARTESIAN_POINT('Origin',(0.,0.,-36.));
#22929=CARTESIAN_POINT('Ctrl Pts',(-8.10164969819937,-0.000190818480503216,
-37.1876535043684));
#22930=CARTESIAN_POINT('Ctrl Pts',(-8.10190702229628,-0.259408063727026,
-37.1800144291204));
#22931=CARTESIAN_POINT('Ctrl Pts',(-8.02700216464902,-1.85062837958727,
-37.1331171519833));
#22932=CARTESIAN_POINT('Ctrl Pts',(-7.01423999417884,-4.68960618017365,
-37.0469616729571));
#22933=CARTESIAN_POINT('Ctrl Pts',(-3.95702765317846,-7.45210691888099,
-36.92918706729));
#22934=CARTESIAN_POINT('Ctrl Pts',(0.0438619977836959,-8.43741959751058,
-36.8114124616229));
#22935=CARTESIAN_POINT('Ctrl Pts',(4.03429158844322,-7.41056343594989,-36.6936378559558));
#22936=CARTESIAN_POINT('Ctrl Pts',(7.06261733076329,-4.61642867900756,-36.5758632502887));
#22937=CARTESIAN_POINT('Ctrl Pts',(8.40664121397815,-0.721355965422936,
-36.4580886446215));
#22938=CARTESIAN_POINT('Ctrl Pts',(7.74583594905282,3.34573518158168,-36.3403140389544));
#22939=CARTESIAN_POINT('Ctrl Pts',(5.23779660784082,6.61495421252791,-36.2225394332873));
#22940=CARTESIAN_POINT('Ctrl Pts',(1.61897602708266,8.24429461880617,-36.1091014203025));
#22941=CARTESIAN_POINT('Ctrl Pts',(-0.957565004786227,8.13102710041623,
-36.0349216092067));
#22942=CARTESIAN_POINT('Ctrl Pts',(-2.10210198597168,7.82452632564983,-36.));
#22943=CARTESIAN_POINT('Origin',(0.,0.,-51.3123464956316));
#22944=CARTESIAN_POINT('',(-8.10208063823041,8.97140133537117E-5,-38.6876535043684));
#22945=CARTESIAN_POINT('',(-8.10145005717011,0.000199025651108617,-38.5623464956316));
#22946=CARTESIAN_POINT('',(-8.1015,-2.19835914433334E-13,-51.3123464956316));
#22947=CARTESIAN_POINT('Ctrl Pts',(-8.10145005717011,0.000199025651108561,
-38.5623464956316));
#22948=CARTESIAN_POINT('Ctrl Pts',(-8.10046090434358,-1.00745585958161,
-38.5326532367576));
#22949=CARTESIAN_POINT('Ctrl Pts',(-7.66255247376433,-3.34819241285004,
-38.4637017759946));
#22950=CARTESIAN_POINT('Ctrl Pts',(-5.46347918924325,-6.4298027756069,-38.3554921133425));
#22951=CARTESIAN_POINT('Ctrl Pts',(-1.76708585226559,-8.25041672623214,
-38.2377175076754));
#22952=CARTESIAN_POINT('Ctrl Pts',(2.35072455830847,-8.10345991964222,-38.1199429020083));
#22953=CARTESIAN_POINT('Ctrl Pts',(5.90793092950644,-6.02397880472869,-38.0021682963412));
#22954=CARTESIAN_POINT('Ctrl Pts',(8.05620579157874,-2.50789093275115,-37.8843936906741));
#22955=CARTESIAN_POINT('Ctrl Pts',(8.28322556673132,1.60628226439634,-37.7666190850069));
#22956=CARTESIAN_POINT('Ctrl Pts',(6.53485031734875,5.33738697798904,-37.6488444793398));
#22957=CARTESIAN_POINT('Ctrl Pts',(3.22803487993391,7.79562443188376,-37.5310698736727));
#22958=CARTESIAN_POINT('Ctrl Pts',(-0.848606625837317,8.39475031472183,
-37.4132952680055));
#22959=CARTESIAN_POINT('Ctrl Pts',(-4.72287154262983,6.99188517896739,-37.2955206623384));
#22960=CARTESIAN_POINT('Ctrl Pts',(-7.4523472329625,3.94222294771503,-37.1785377382137));
#22961=CARTESIAN_POINT('Ctrl Pts',(-8.10190554473014,1.30502253442654,-37.1008130159782));
#22962=CARTESIAN_POINT('Ctrl Pts',(-8.10215956429164,-2.6882833979924E-5,
-37.0623464956316));
#22963=CARTESIAN_POINT('Ctrl Pts',(-8.10208063823041,8.97140133539198E-5,
-38.6876535043684));
#22964=CARTESIAN_POINT('Ctrl Pts',(-8.10137161840911,-1.23965580576583,
-38.6511128517889));
#22965=CARTESIAN_POINT('Ctrl Pts',(-7.50185551031583,-3.81200985713521,
-38.5753139973203));
#22966=CARTESIAN_POINT('Ctrl Pts',(-4.89068362979871,-6.87554954592136,
-38.4602569409627));
#22967=CARTESIAN_POINT('Ctrl Pts',(-1.05150112347229,-8.3717568832205,-38.3424823352955));
#22968=CARTESIAN_POINT('Ctrl Pts',(3.03844482120267,-7.87145609112005,-38.2247077296284));
#22969=CARTESIAN_POINT('Ctrl Pts',(6.40377825371979,-5.49395959222041,-38.1069331239613));
#22970=CARTESIAN_POINT('Ctrl Pts',(8.24192981481277,-1.80625603195024,-37.9891585182942));
#22971=CARTESIAN_POINT('Ctrl Pts',(8.11453458490175,2.31220595952502,-37.871383912627));
#22972=CARTESIAN_POINT('Ctrl Pts',(6.05197395361438,5.87924988197173,-37.7536093069599));
#22973=CARTESIAN_POINT('Ctrl Pts',(2.54613022648071,8.0442021874585,-37.6358347012928));
#22974=CARTESIAN_POINT('Ctrl Pts',(-1.56691815067151,8.29076204944015,-37.5180600956257));
#22975=CARTESIAN_POINT('Ctrl Pts',(-5.30628572285852,6.56012956115795,-37.4002854899586));
#22976=CARTESIAN_POINT('Ctrl Pts',(-7.61974018825314,3.47875455134372,-37.2901499595394));
#22977=CARTESIAN_POINT('Ctrl Pts',(-8.10058460027276,1.07274309548756,-37.2192726310094));
#22978=CARTESIAN_POINT('Ctrl Pts',(-8.10164969819937,-0.000190818480503216,
-37.1876535043684));
#22979=CARTESIAN_POINT('Origin',(0.,0.,-51.3123464956316));
#22980=CARTESIAN_POINT('',(-8.1011219890517,0.00016778068961748,-40.1876535043684));
#22981=CARTESIAN_POINT('',(-8.10084079205323,-8.85032130801111E-6,-40.0623464956316));
#22982=CARTESIAN_POINT('',(-8.1015,-2.19835914433334E-13,-51.3123464956316));
#22983=CARTESIAN_POINT('Ctrl Pts',(-8.10084079205322,-8.85032130713836E-6,
-40.0623464956316));
#22984=CARTESIAN_POINT('Ctrl Pts',(-8.10086630096926,-0.656348422050696,
-40.0430098613152));
#22985=CARTESIAN_POINT('Ctrl Pts',(-7.86185833292864,-2.64520314986847,
-39.9844150251097));
#22986=CARTESIAN_POINT('Ctrl Pts',(-6.25172246740249,-5.66638639445397,
-39.8865619870152));
#22987=CARTESIAN_POINT('Ctrl Pts',(-2.82286511373573,-7.95131442783728,
-39.768787381348));
#22988=CARTESIAN_POINT('Ctrl Pts',(1.27919300612309,-8.34000202840266,-39.651012775681));
#22989=CARTESIAN_POINT('Ctrl Pts',(5.07618741335941,-6.73975444101172,-39.5332381700138));
#22990=CARTESIAN_POINT('Ctrl Pts',(7.66260564414886,-3.53220091768916,-39.4154635643467));
#22991=CARTESIAN_POINT('Ctrl Pts',(8.42163511110229,0.517716752808797,-39.2976889586796));
#22992=CARTESIAN_POINT('Ctrl Pts',(7.17226141992802,4.4441686179642,-39.1799143530125));
#22993=CARTESIAN_POINT('Ctrl Pts',(4.21243693189744,7.31076902079321,-39.0621397473453));
#22994=CARTESIAN_POINT('Ctrl Pts',(0.248024673685762,8.43388714307694,-38.9443651416782));
#22995=CARTESIAN_POINT('Ctrl Pts',(-3.77553685080373,7.54568022568945,-38.8265905360111));
#22996=CARTESIAN_POINT('Ctrl Pts',(-6.89870313918519,4.85796907966996,-38.7088159303439));
#22997=CARTESIAN_POINT('Ctrl Pts',(-8.0040363497543,1.98143594698576,-38.6207345835508));
#22998=CARTESIAN_POINT('Ctrl Pts',(-8.10176868809099,0.324789923437666,
-38.5719114386467));
#22999=CARTESIAN_POINT('Ctrl Pts',(-8.10145005717011,0.000199025651108561,
-38.5623464956316));
#23000=CARTESIAN_POINT('Ctrl Pts',(-8.1011219890517,0.000167780689617515,
-40.1876535043684));
#23001=CARTESIAN_POINT('Ctrl Pts',(-8.10043536239369,-0.888503088336933,
-40.1614694763464));
#23002=CARTESIAN_POINT('Ctrl Pts',(-7.73586399862886,-3.11012449507375,
-40.0960272464354));
#23003=CARTESIAN_POINT('Ctrl Pts',(-5.74161917229395,-6.18269983140913,
-39.9913268146354));
#23004=CARTESIAN_POINT('Ctrl Pts',(-2.12907933537458,-8.16449564324956,
-39.8735522089682));
#23005=CARTESIAN_POINT('Ctrl Pts',(1.9912062783033,-8.19921127195815,-39.7557776033011));
#23006=CARTESIAN_POINT('Ctrl Pts',(5.63662627205554,-6.27856768651366,-39.638002997634));
#23007=CARTESIAN_POINT('Ctrl Pts',(7.93781585726883,-2.86060261851435,-39.5202283919668));
#23008=CARTESIAN_POINT('Ctrl Pts',(8.3459841673938,1.23956290787192,-39.4024537862997));
#23009=CARTESIAN_POINT('Ctrl Pts',(6.76379066080322,5.0441157621324,-39.2846791806326));
#23010=CARTESIAN_POINT('Ctrl Pts',(3.56855902743119,7.64574093157071,-39.1669045749655));
#23011=CARTESIAN_POINT('Ctrl Pts',(-0.477707485283489,8.42399925709112,
-39.0491299692983));
#23012=CARTESIAN_POINT('Ctrl Pts',(-4.4100496579569,7.19329061968874,-38.9313553636312));
#23013=CARTESIAN_POINT('Ctrl Pts',(-7.29067710496446,4.24711611286043,-38.8135807579641));
#23014=CARTESIAN_POINT('Ctrl Pts',(-8.07831747062495,1.51640970996623,-38.7323468048765));
#23015=CARTESIAN_POINT('Ctrl Pts',(-8.10213336844155,0.09229030002937,-38.6903710536779));
#23016=CARTESIAN_POINT('Ctrl Pts',(-8.10208063823041,8.97140133539198E-5,
-38.6876535043684));
#23017=CARTESIAN_POINT('Origin',(0.,0.,-51.3123464956316));
#23018=CARTESIAN_POINT('',(-8.10093877791723,-0.000108962703712356,-41.6876535043684));
#23019=CARTESIAN_POINT('',(-8.10151037503517,-0.000198521445029568,-41.5623464956316));
#23020=CARTESIAN_POINT('',(-8.1015,-2.19835914433334E-13,-51.3123464956316));
#23021=CARTESIAN_POINT('Ctrl Pts',(-8.10151037503517,-0.000198521445028341,
-41.5623464956316));
#23022=CARTESIAN_POINT('Ctrl Pts',(-8.10181323302049,-0.304932897552518,
-41.5533664858727));
#23023=CARTESIAN_POINT('Ctrl Pts',(-8.01118479339215,-1.9417053813148,-41.5051282742248));
#23024=CARTESIAN_POINT('Ctrl Pts',(-6.93422489492358,-4.80712946437895,
-41.4176318606879));
#23025=CARTESIAN_POINT('Ctrl Pts',(-3.83089878888002,-7.51772459259022,
-41.2998572550207));
#23026=CARTESIAN_POINT('Ctrl Pts',(0.186025344688875,-8.43548238998882,
-41.1820826493536));
#23027=CARTESIAN_POINT('Ctrl Pts',(4.15858589745246,-7.3415347110933,-41.0643080436865));
#23028=CARTESIAN_POINT('Ctrl Pts',(7.13940114902576,-4.49676770736134,-40.9465334380193));
#23029=CARTESIAN_POINT('Ctrl Pts',(8.41760216646814,-0.579605337923066,
-40.8287588323522));
#23030=CARTESIAN_POINT('Ctrl Pts',(7.68836180798567,3.47578211201243,-40.7109842266851));
#23031=CARTESIAN_POINT('Ctrl Pts',(5.12559032018552,6.70226024937101,-40.593209621018));
#23032=CARTESIAN_POINT('Ctrl Pts',(1.34046098257293,8.33037411734177,-40.4754350153508));
#23033=CARTESIAN_POINT('Ctrl Pts',(-2.76434333919955,7.97184887486595,-40.3576604096838));
#23034=CARTESIAN_POINT('Ctrl Pts',(-6.20990324829623,5.71218611631991,-40.2398858040166));
#23035=CARTESIAN_POINT('Ctrl Pts',(-7.85195993614671,2.68493126162982,-40.1414478326659));
#23036=CARTESIAN_POINT('Ctrl Pts',(-8.10081451149239,0.676184995765657,
-40.0822680632042));
#23037=CARTESIAN_POINT('Ctrl Pts',(-8.10084079205322,-8.85032130713836E-6,
-40.0623464956316));
#23038=CARTESIAN_POINT('Ctrl Pts',(-8.10093877791723,-0.000108962703712148,
-41.6876535043684));
#23039=CARTESIAN_POINT('Ctrl Pts',(-8.10119988867663,-0.537316780940126,
-41.671826100904));
#23040=CARTESIAN_POINT('Ctrl Pts',(-7.9179157370419,-2.40683601775939,-41.6167404955505));
#23041=CARTESIAN_POINT('Ctrl Pts',(-6.49544168759803,-5.38527670672303,
-41.522396688308));
#23042=CARTESIAN_POINT('Ctrl Pts',(-3.17064656618999,-7.81914114703574,
-41.4046220826409));
#23043=CARTESIAN_POINT('Ctrl Pts',(0.910288721922364,-8.38828602085676,
-41.2868474769737));
#23044=CARTESIAN_POINT('Ctrl Pts',(4.77413709997572,-6.95698087359707,-41.1690728713066));
#23045=CARTESIAN_POINT('Ctrl Pts',(7.4994426769679,-3.86656533112174,-41.0512982656395));
#23046=CARTESIAN_POINT('Ctrl Pts',(8.43627081960314,0.145954045071271,-40.9335236599723));
#23047=CARTESIAN_POINT('Ctrl Pts',(7.36120546016224,4.12366609926623,-40.8157490543053));
#23048=CARTESIAN_POINT('Ctrl Pts',(4.53062966851309,7.11796057391082,-40.6979744486381));
#23049=CARTESIAN_POINT('Ctrl Pts',(0.619583063952851,8.41475399235312,-40.5801998429711));
#23050=CARTESIAN_POINT('Ctrl Pts',(-3.43922256435361,7.70478527136227,-40.4624252373038));
#23051=CARTESIAN_POINT('Ctrl Pts',(-6.67783765143915,5.15736873085314,-40.3446506316368));
#23052=CARTESIAN_POINT('Ctrl Pts',(-7.95795209728732,2.21980900261142,-40.2530600539916));
#23053=CARTESIAN_POINT('Ctrl Pts',(-8.10146483455665,0.443897730966563,
-40.2007276782355));
#23054=CARTESIAN_POINT('Ctrl Pts',(-8.1011219890517,0.000167780689617515,
-40.1876535043684));
#23055=CARTESIAN_POINT('Origin',(0.,0.,-51.3123464956316));
#23056=CARTESIAN_POINT('',(-8.10186514679612,-0.000159416706437265,-43.1876535043684));
#23057=CARTESIAN_POINT('',(-8.10214365571365,4.6928369269332E-5,-43.0623464956316));
#23058=CARTESIAN_POINT('',(-8.1015,-2.19835914433334E-13,-51.3123464956316));
#23059=CARTESIAN_POINT('Ctrl Pts',(-8.10214365571365,4.69283692696408E-5,
-43.0623464956316));
#23060=CARTESIAN_POINT('Ctrl Pts',(-8.10172795851372,-1.28516454579568,
-43.0244649085412));
#23061=CARTESIAN_POINT('Ctrl Pts',(-7.46758783086871,-3.90268783700937,
-42.9473251195619));
#23062=CARTESIAN_POINT('Ctrl Pts',(-4.77413712196194,-6.95698090563593,
-42.8309271286933));
#23063=CARTESIAN_POINT('Ctrl Pts',(-0.910288726114504,-8.38828605948718,
-42.7131525230263));
#23064=CARTESIAN_POINT('Ctrl Pts',(3.17064658079171,-7.8191411830451,-42.5953779173591));
#23065=CARTESIAN_POINT('Ctrl Pts',(6.49544171751139,-5.38527673152374,-42.477603311692));
#23066=CARTESIAN_POINT('Ctrl Pts',(8.27119495360724,-1.66712405660176,-42.3598287060249));
#23067=CARTESIAN_POINT('Ctrl Pts',(8.07442220785581,2.44860666297451,-42.2420541003577));
#23068=CARTESIAN_POINT('Ctrl Pts',(5.95205011609281,5.98039028794925,-42.1242794946906));
#23069=CARTESIAN_POINT('Ctrl Pts',(2.41022490236832,8.08596218768562,-42.0065048890235));
#23070=CARTESIAN_POINT('Ctrl Pts',(-1.70639407074438,8.26318267110237,-41.8887302833564));
#23071=CARTESIAN_POINT('Ctrl Pts',(-5.41606983206093,6.46978795285578,-41.7709556776892));
#23072=CARTESIAN_POINT('Ctrl Pts',(-7.64974417706006,3.38785496849908,-41.662161081781));
#23073=CARTESIAN_POINT('Ctrl Pts',(-8.10048921887679,1.02728432503435,-41.5926246877618));
#23074=CARTESIAN_POINT('Ctrl Pts',(-8.10151037503517,-0.000198521445028341,
-41.5623464956316));
#23075=CARTESIAN_POINT('Ctrl Pts',(-8.10186514679612,-0.000159416706436502,
-43.1876535043684));
#23076=CARTESIAN_POINT('Ctrl Pts',(-8.10203123770816,-0.185785457421342,
-43.1821827254615));
#23077=CARTESIAN_POINT('Ctrl Pts',(-8.05090917221341,-1.70336898962407,
-43.1374537446656));
#23078=CARTESIAN_POINT('Ctrl Pts',(-7.1394011161468,-4.49676768665247,-43.0534665619807));
#23079=CARTESIAN_POINT('Ctrl Pts',(-4.15858587830098,-7.34153467728348,
-42.9356919563136));
#23080=CARTESIAN_POINT('Ctrl Pts',(-0.186025343832157,-8.43548235114104,
-42.8179173506464));
#23081=CARTESIAN_POINT('Ctrl Pts',(3.83089877123767,-7.51772455796898,-42.7001427449793));
#23082=CARTESIAN_POINT('Ctrl Pts',(6.93422486298953,-4.80712944224074,-42.5823681393122));
#23083=CARTESIAN_POINT('Ctrl Pts',(8.38386744432517,-0.950123466158245,
-42.464593533645));
#23084=CARTESIAN_POINT('Ctrl Pts',(7.83411375280636,3.13346926473683,-42.3468189279779));
#23085=CARTESIAN_POINT('Ctrl Pts',(5.41606980711838,6.46978792306059,-42.2290443223107));
#23086=CARTESIAN_POINT('Ctrl Pts',(1.70639406288594,8.2631826330481,-42.1112697166436));
#23087=CARTESIAN_POINT('Ctrl Pts',(-2.4102248912686,8.08596215044749,-41.9934951109765));
#23088=CARTESIAN_POINT('Ctrl Pts',(-5.95205008868199,5.98039026040782,-41.8757205053094));
#23089=CARTESIAN_POINT('Ctrl Pts',(-7.78920245753314,2.92323328116088,-41.7737733031067));
#23090=CARTESIAN_POINT('Ctrl Pts',(-8.10055223102823,0.795170448066936,
-41.711084302793));
#23091=CARTESIAN_POINT('Ctrl Pts',(-8.10093877791723,-0.000108962703712148,
-41.6876535043684));
#23092=CARTESIAN_POINT('Origin',(0.,0.,-51.3123464956316));
#23093=CARTESIAN_POINT('',(-8.10191814333788,0.000147149967349575,-44.6876535043684));
#23094=CARTESIAN_POINT('',(-8.1012379593904,0.000186305278623682,-44.5623464956316));
#23095=CARTESIAN_POINT('',(-8.1015,-2.19835914433334E-13,-51.3123464956316));
#23096=CARTESIAN_POINT('Ctrl Pts',(-8.1012379593904,0.000186305278623185,
-44.5623464956316));
#23097=CARTESIAN_POINT('Ctrl Pts',(-8.10041846603269,-0.93395673238637,
-44.5348215330988));
#23098=CARTESIAN_POINT('Ctrl Pts',(-7.70856096931196,-3.20111578570497,
-44.4680383686769));
#23099=CARTESIAN_POINT('Ctrl Pts',(-5.63662629801377,-6.27856771542826,
-44.3619970023661));
#23100=CARTESIAN_POINT('Ctrl Pts',(-1.99120628747333,-8.19921130971783,
-44.2442223966989));
#23101=CARTESIAN_POINT('Ctrl Pts',(2.12907934517964,-8.16449568084935,-44.1264477910318));
#23102=CARTESIAN_POINT('Ctrl Pts',(5.74161919873576,-6.18269985988217,-44.0086731853647));
#23103=CARTESIAN_POINT('Ctrl Pts',(7.98488978577069,-2.72644524789567,-43.8908985796975));
#23104=CARTESIAN_POINT('Ctrl Pts',(8.32391284231425,1.38001578767571,-43.7731239740304));
#23105=CARTESIAN_POINT('Ctrl Pts',(6.67783768219246,5.1573687546043,-43.6553493683633));
#23106=CARTESIAN_POINT('Ctrl Pts',(3.43922258019218,7.70478530684499,-43.5375747626961));
#23107=CARTESIAN_POINT('Ctrl Pts',(-0.619583066806221,8.41475403110543,
-43.4198001570291));
#23108=CARTESIAN_POINT('Ctrl Pts',(-4.53062968937796,7.11796060669102,-43.3020255513619));
#23109=CARTESIAN_POINT('Ctrl Pts',(-7.36120549406269,4.12366611825681,-43.1842509456948));
#23110=CARTESIAN_POINT('Ctrl Pts',(-8.0904816961954,1.42536436889202,-43.104357927118));
#23111=CARTESIAN_POINT('Ctrl Pts',(-8.10215876212711,0.0467514429017632,
-43.0637231104303));
#23112=CARTESIAN_POINT('Ctrl Pts',(-8.10214365571365,4.69283692696408E-5,
-43.0623464956316));
#23113=CARTESIAN_POINT('Ctrl Pts',(-8.10191814333787,0.00014714996734987,
-44.6876535043684));
#23114=CARTESIAN_POINT('Ctrl Pts',(-8.10093166009298,-1.16610059920954,
-44.6532811481301));
#23115=CARTESIAN_POINT('Ctrl Pts',(-7.55530879276033,-3.66526533641054,
-44.5796505900026));
#23116=CARTESIAN_POINT('Ctrl Pts',(-5.0761873899821,-6.73975440997329,-44.4667618299862));
#23117=CARTESIAN_POINT('Ctrl Pts',(-1.27919300023199,-8.3400019899946,-44.3489872243191));
#23118=CARTESIAN_POINT('Ctrl Pts',(2.82286510073567,-7.95131439121922,-44.2312126186519));
#23119=CARTESIAN_POINT('Ctrl Pts',(6.25172243861154,-5.66638636835865,-44.1134380129848));
#23120=CARTESIAN_POINT('Ctrl Pts',(8.18966038568263,-2.03013070814185,-43.9956634073177));
#23121=CARTESIAN_POINT('Ctrl Pts',(8.17451682713419,2.09027332372109,-43.8778888016505));
#23122=CARTESIAN_POINT('Ctrl Pts',(6.20990321969786,5.71218609001371,-43.7601141959834));
#23123=CARTESIAN_POINT('Ctrl Pts',(2.76434332646893,7.97184883815334,-43.6423395903163));
#23124=CARTESIAN_POINT('Ctrl Pts',(-1.34046097639977,8.33037407897806,-43.5245649846492));
#23125=CARTESIAN_POINT('Ctrl Pts',(-5.12559029658075,6.70226021850519,-43.406790378982));
#23126=CARTESIAN_POINT('Ctrl Pts',(-7.569317806737,3.62565607228497,-43.2944865522218));
#23127=CARTESIAN_POINT('Ctrl Pts',(-8.10083937258845,1.1462633616389,-43.2214409273506));
#23128=CARTESIAN_POINT('Ctrl Pts',(-8.10186514679612,-0.000159416706436502,
-43.1876535043684));
#23129=CARTESIAN_POINT('Origin',(0.,0.,-51.3123464956316));
#23130=CARTESIAN_POINT('',(-8.10097060232049,0.000123429424611077,-46.1876535043684));
#23131=CARTESIAN_POINT('',(-8.10088198729152,-7.28186706448135E-5,-46.0623464956316));
#23132=CARTESIAN_POINT('',(-8.1015,-2.19835914433334E-13,-51.3123464956316));
#23133=CARTESIAN_POINT('Ctrl Pts',(-8.10088198729152,-7.28186706448752E-5,
-46.0623464956316));
#23134=CARTESIAN_POINT('Ctrl Pts',(-8.10106954261305,-0.582805848585725,
-46.0451781576563));
#23135=CARTESIAN_POINT('Ctrl Pts',(-7.8971652255018,-2.4979235666786,-45.988751617792));
#23136=CARTESIAN_POINT('Ctrl Pts',(-6.40377828321054,-5.49395961752304,
-45.8930668760387));
#23137=CARTESIAN_POINT('Ctrl Pts',(-3.03844483519571,-7.87145612736966,
-45.7752922703716));
#23138=CARTESIAN_POINT('Ctrl Pts',(1.05150112831493,-8.37175692177514,-45.6575176647045));
#23139=CARTESIAN_POINT('Ctrl Pts',(4.89068365232167,-6.87554957758499,-45.5397430590373));
#23140=CARTESIAN_POINT('Ctrl Pts',(7.56352919268905,-3.73965168591192,-45.4219684533702));
#23141=CARTESIAN_POINT('Ctrl Pts',(8.43261385803414,0.288083498271241,-45.3041938477031));
#23142=CARTESIAN_POINT('Ctrl Pts',(7.29067713854007,4.2471161324196,-45.1864192420359));
#23143=CARTESIAN_POINT('Ctrl Pts',(4.41004967826638,7.19329065281592,-45.0686446363688));
#23144=CARTESIAN_POINT('Ctrl Pts',(0.477707487483417,8.42399929588601,-44.9508700307017));
#23145=CARTESIAN_POINT('Ctrl Pts',(-3.56855904386543,7.64574096678149,-44.8330954250346));
#23146=CARTESIAN_POINT('Ctrl Pts',(-6.76379069195239,5.04411578536195,-44.7153208193674));
#23147=CARTESIAN_POINT('Ctrl Pts',(-7.97621164796412,2.12872042471518,-44.6250711762331));
#23148=CARTESIAN_POINT('Ctrl Pts',(-8.10158728999186,0.398389348818652,
-44.5740797349878));
#23149=CARTESIAN_POINT('Ctrl Pts',(-8.1012379593904,0.000186305278623185,
-44.5623464956316));
#23150=CARTESIAN_POINT('Ctrl Pts',(-8.10097060232049,0.000123429424611493,
-46.1876535043684));
#23151=CARTESIAN_POINT('Ctrl Pts',(-8.10051945174223,-0.815000391918625,
-46.1636377726876));
#23152=CARTESIAN_POINT('Ctrl Pts',(-7.77817455032938,-2.96294542208346,
-46.1003638391178));
#23153=CARTESIAN_POINT('Ctrl Pts',(-5.90793090228909,-6.02397877694788,
-45.9978317036589));
#23154=CARTESIAN_POINT('Ctrl Pts',(-2.35072454748789,-8.10345988234339,
-45.8800570979917));
#23155=CARTESIAN_POINT('Ctrl Pts',(1.76708584413041,-8.25041668822644,-45.7622824923246));
#23156=CARTESIAN_POINT('Ctrl Pts',(5.46347916408095,-6.42980274600106,-45.6445078866575));
#23157=CARTESIAN_POINT('Ctrl Pts',(7.85693443764436,-3.07580057347912,-45.5267332809903));
#23158=CARTESIAN_POINT('Ctrl Pts',(8.37665714814605,1.01172276152054,-45.4089586753233));
#23159=CARTESIAN_POINT('Ctrl Pts',(6.89870310741494,4.85796905729832,-45.291184069656));
#23160=CARTESIAN_POINT('Ctrl Pts',(3.77553683341622,7.54568019093911,-45.173409463989));
#23161=CARTESIAN_POINT('Ctrl Pts',(-0.248024672543488,8.4338871042367,-45.0556348583218));
#23162=CARTESIAN_POINT('Ctrl Pts',(-4.21243691249803,7.31076898712496,-44.9378602526548));
#23163=CARTESIAN_POINT('Ctrl Pts',(-7.17226138689772,4.44416859749758,-44.8200856469875));
#23164=CARTESIAN_POINT('Ctrl Pts',(-8.05700708526735,1.66364630693569,-44.7366833975588));
#23165=CARTESIAN_POINT('Ctrl Pts',(-8.10205836662772,0.165922997669041,
-44.6925393500191));
#23166=CARTESIAN_POINT('Ctrl Pts',(-8.10191814333787,0.00014714996734987,
-44.6876535043684));
#23167=CARTESIAN_POINT('Origin',(0.,0.,-51.3123464956316));
#23168=CARTESIAN_POINT('',(-8.1010842906964,-0.000174961242810356,-47.6876535043684));
#23169=CARTESIAN_POINT('',(-8.10173447928736,-0.000181404600999652,-47.5623464956316));
#23170=CARTESIAN_POINT('',(-8.1015,-2.19835914433334E-13,-51.3123464956316));
#23171=CARTESIAN_POINT('',(-2.10185380438479,7.8240982122538,-48.));
#23172=CARTESIAN_POINT('Ctrl Pts',(-2.10185380438476,7.82409821225381,-48.));
#23173=CARTESIAN_POINT('Ctrl Pts',(-3.38848271769056,7.47846018434309,-47.960741798111));
#23174=CARTESIAN_POINT('Ctrl Pts',(-5.7867414247356,6.14069431107141,-47.8822253943329));
#23175=CARTESIAN_POINT('Ctrl Pts',(-7.74755312548167,3.07031331488377,-47.778109895789));
#23176=CARTESIAN_POINT('Ctrl Pts',(-8.10047270114376,0.868629507982853,
-47.7132525991342));
#23177=CARTESIAN_POINT('Ctrl Pts',(-8.1010842906964,-0.000174961242810426,
-47.6876535043684));
#23178=CARTESIAN_POINT('',(2.10210202563587,7.82452631996418,-48.));
#23179=CARTESIAN_POINT('Origin',(0.,0.,-48.));
#23180=CARTESIAN_POINT('Ctrl Pts',(2.10210202563587,7.82452631996418,-48.));
#23181=CARTESIAN_POINT('Ctrl Pts',(0.957565047422177,8.13102709012696,-47.9650783907933));
#23182=CARTESIAN_POINT('Ctrl Pts',(-1.61897608126858,8.24429472572672,-47.8908985796976));
#23183=CARTESIAN_POINT('Ctrl Pts',(-5.23779660691551,6.61495420237904,-47.7774605667127));
#23184=CARTESIAN_POINT('Ctrl Pts',(-7.6007788734818,3.5348165809474,-47.6664976744634));
#23185=CARTESIAN_POINT('Ctrl Pts',(-8.10066624715266,1.10079321078201,-47.5947929841029));
#23186=CARTESIAN_POINT('Ctrl Pts',(-8.10173447928736,-0.000181404600998816,
-47.5623464956316));
#23187=CARTESIAN_POINT('Origin',(0.,0.,-51.3123464956316));
#23188=CARTESIAN_POINT('Ctrl Pts',(-8.10173447928736,-0.000181404600998816,
-47.5623464956316));
#23189=CARTESIAN_POINT('Ctrl Pts',(-8.10195874057133,-0.231316541667576,
-47.5555347822139));
#23190=CARTESIAN_POINT('Ctrl Pts',(-8.03636740777228,-1.79443477535343,
-47.5094648669071));
#23191=CARTESIAN_POINT('Ctrl Pts',(-7.06261736652514,-4.61642869377352,
-47.4241367497114));
#23192=CARTESIAN_POINT('Ctrl Pts',(-4.03429160538818,-7.41056347354498,
-47.3063621440442));
#23193=CARTESIAN_POINT('Ctrl Pts',(-0.04386199881008,-8.4374196345273,-47.1885875383771));
#23194=CARTESIAN_POINT('Ctrl Pts',(3.95702767181747,-7.45210695417129,-47.07081293271));
#23195=CARTESIAN_POINT('Ctrl Pts',(7.0142400262719,-4.68960620126019,-46.9530383270429));
#23196=CARTESIAN_POINT('Ctrl Pts',(8.39868669392937,-0.808721361269664,
-46.8352637213757));
#23197=CARTESIAN_POINT('Ctrl Pts',(7.78020299818498,3.26502830145453,-46.7174891157086));
#23198=CARTESIAN_POINT('Ctrl Pts',(5.30628574732215,6.56012959129681,-46.5997145100415));
#23199=CARTESIAN_POINT('Ctrl Pts',(1.56691815787412,8.290762087659,-46.4819399043743));
#23200=CARTESIAN_POINT('Ctrl Pts',(-2.54613023819965,8.04420222448489,-46.3641652987072));
#23201=CARTESIAN_POINT('Ctrl Pts',(-6.05197398148885,5.87924990905731,-46.2463906930401));
#23202=CARTESIAN_POINT('Ctrl Pts',(-7.81386931352349,2.83218407214127,-46.1457844253482));
#23203=CARTESIAN_POINT('Ctrl Pts',(-8.10064066681339,0.749708164640068,
-46.0844363595454));
#23204=CARTESIAN_POINT('Ctrl Pts',(-8.10088198729152,-7.28186706448752E-5,
-46.0623464956316));
#23205=CARTESIAN_POINT('Ctrl Pts',(-8.1010842906964,-0.000174961242810426,
-47.6876535043684));
#23206=CARTESIAN_POINT('Ctrl Pts',(-8.10141062126752,-0.463749686165932,
-47.6739943972452));
#23207=CARTESIAN_POINT('Ctrl Pts',(-7.94970659616376,-2.25948586872497,
-47.6210770882329));
#23208=CARTESIAN_POINT('Ctrl Pts',(-6.63976806498755,-5.20635630979624,
-47.5289015773315));
#23209=CARTESIAN_POINT('Ctrl Pts',(-3.38248655907778,-7.72983620180326,
-47.4111269716644));
#23210=CARTESIAN_POINT('Ctrl Pts',(0.681413555862794,-8.40998264592954,
-47.2933523659973));
#23211=CARTESIAN_POINT('Ctrl Pts',(4.58282963250162,-7.08446123670512,-47.1755777603301));
#23212=CARTESIAN_POINT('Ctrl Pts',(7.39131613068618,-4.06944919929777,-47.057803154663));
#23213=CARTESIAN_POINT('Ctrl Pts',(8.43711630815339,-0.0839387386951516,
-46.9400285489959));
#23214=CARTESIAN_POINT('Ctrl Pts',(7.47081891547249,3.92158434705153,-46.8222539433287));
#23215=CARTESIAN_POINT('Ctrl Pts',(4.72287152121607,6.99188514875576,-46.7044793376616));
#23216=CARTESIAN_POINT('Ctrl Pts',(0.848606621735488,8.39475027502305,-46.5867047319945));
#23217=CARTESIAN_POINT('Ctrl Pts',(-3.22803486495866,7.79562439652349,-46.4689301263274));
#23218=CARTESIAN_POINT('Ctrl Pts',(-6.53485028731455,5.33738695312811,-46.3511555206602));
#23219=CARTESIAN_POINT('Ctrl Pts',(-7.92670970382778,2.36710169478299,-46.2573966466739));
#23220=CARTESIAN_POINT('Ctrl Pts',(-8.10125694168087,0.517471837874847,
-46.2028959745766));
#23221=CARTESIAN_POINT('Ctrl Pts',(-8.10097060232049,0.000123429424611493,
-46.1876535043684));
#23222=CARTESIAN_POINT('Ctrl Pts',(5.46288453460432,-4.78623668048091,-48.));
#23223=CARTESIAN_POINT('Ctrl Pts',(6.2499542175215,-3.88789606644505,-47.960741798111));
#23224=CARTESIAN_POINT('Ctrl Pts',(7.37171595554078,-1.69639746569614,-47.8822253943329));
#23225=CARTESIAN_POINT('Ctrl Pts',(7.29581740547595,1.99731954537833,-47.7644507886657));
#23226=CARTESIAN_POINT('Ctrl Pts',(5.4801165872417,5.21397460516973,-47.6466761829987));
#23227=CARTESIAN_POINT('Ctrl Pts',(2.3574553976849,7.18755200305922,-47.5289015773315));
#23228=CARTESIAN_POINT('Ctrl Pts',(-1.32738855178181,7.4468564743695,-47.4111269716644));
#23229=CARTESIAN_POINT('Ctrl Pts',(-4.69568805233936,5.9303107291093,-47.2933523659972));
#23230=CARTESIAN_POINT('Ctrl Pts',(-6.94414699118569,2.99945379218927,-47.1755777603301));
#23231=CARTESIAN_POINT('Ctrl Pts',(-7.53655932503615,-0.646696104264617,
-47.057803154663));
#23232=CARTESIAN_POINT('Ctrl Pts',(-6.3316410458646,-4.13863131554368,-46.9400285489958));
#23233=CARTESIAN_POINT('Ctrl Pts',(-3.61674503856499,-6.64357495628676,
-46.8222539433288));
#23234=CARTESIAN_POINT('Ctrl Pts',(-0.0393223103570487,-7.5641521700391,
-46.7044793376616));
#23235=CARTESIAN_POINT('Ctrl Pts',(3.54747787204966,-6.68081871358959,-46.5867047319945));
#23236=CARTESIAN_POINT('Ctrl Pts',(6.2882707289777,-4.20423499842656,-46.4689301263273));
#23237=CARTESIAN_POINT('Ctrl Pts',(7.52942806369302,-0.725019224452457,
-46.3511555206603));
#23238=CARTESIAN_POINT('Ctrl Pts',(6.97495702966333,2.92709998808421,-46.233380914993));
#23239=CARTESIAN_POINT('Ctrl Pts',(4.7570886110968,5.88116042974619,-46.115606309326));
#23240=CARTESIAN_POINT('Ctrl Pts',(1.40474314394121,7.43267358423345,-45.9978317036588));
#23241=CARTESIAN_POINT('Ctrl Pts',(-2.28260740851004,7.21163250712014,-45.8800570979917));
#23242=CARTESIAN_POINT('Ctrl Pts',(-5.42559859625422,5.27075135338927,-45.7622824923246));
#23243=CARTESIAN_POINT('Ctrl Pts',(-7.27468554731165,2.07289415063032,-45.6445078866575));
#23244=CARTESIAN_POINT('Ctrl Pts',(-7.38889545401083,-1.61930971060316,
-45.5267332809903));
#23245=CARTESIAN_POINT('Ctrl Pts',(-5.7409913807268,-4.92533835734985,-45.4089586753232));
#23246=CARTESIAN_POINT('Ctrl Pts',(-2.72396776375072,-7.056765519112,-45.2911840696561));
#23247=CARTESIAN_POINT('Ctrl Pts',(0.942671442936654,-7.50528550550551,
-45.173409463989));
#23248=CARTESIAN_POINT('Ctrl Pts',(4.38450106360703,-6.16393465185457,-45.0556348583218));
#23249=CARTESIAN_POINT('Ctrl Pts',(6.7807088226255,-3.35260015981957,-44.9378602526547));
#23250=CARTESIAN_POINT('Ctrl Pts',(7.55984378829871,0.258267042886377,-44.8200856469876));
#23251=CARTESIAN_POINT('Ctrl Pts',(6.53609677926514,3.80754236496496,-44.7023110413205));
#23252=CARTESIAN_POINT('Ctrl Pts',(3.95361239440211,6.44878973170425,-44.5845364356533));
#23253=CARTESIAN_POINT('Ctrl Pts',(0.42826507209678,7.55212082775043,-44.4667618299862));
#23254=CARTESIAN_POINT('Ctrl Pts',(-3.19921549535205,6.85441173137493,-44.3489872243191));
#23255=CARTESIAN_POINT('Ctrl Pts',(-6.06374273846204,4.52205307030598,-44.2312126186519));
#23256=CARTESIAN_POINT('Ctrl Pts',(-7.4821802489587,1.11126895529654,-44.1134380129848));
#23257=CARTESIAN_POINT('Ctrl Pts',(-7.11625709274196,-2.56453211305952,
-43.9956634073177));
#23258=CARTESIAN_POINT('Ctrl Pts',(-5.05323912886181,-5.62874002557001,
-43.8778888016506));
#23259=CARTESIAN_POINT('Ctrl Pts',(-1.78511772707755,-7.35059825248172,
-43.7601141959834));
#23260=CARTESIAN_POINT('Ctrl Pts',(1.90872101265689,-7.31947566870441,-43.6423395903163));
#23261=CARTESIAN_POINT('Ctrl Pts',(5.14736533239743,-5.54279443094788,-43.5245649846491));
#23262=CARTESIAN_POINT('Ctrl Pts',(7.15845886737674,-2.44425993155172,-43.406790378982));
#23263=CARTESIAN_POINT('Ctrl Pts',(7.46239325726449,1.23718504794034,-43.2890157733149));
#23264=CARTESIAN_POINT('Ctrl Pts',(5.98668580951229,4.62358443062285,-43.1712411676478));
#23265=CARTESIAN_POINT('Ctrl Pts',(3.08326527185531,6.90734502050424,-43.0534665619806));
#23266=CARTESIAN_POINT('Ctrl Pts',(-0.55545662089904,7.54383244188345,-42.9356919563136));
#23267=CARTESIAN_POINT('Ctrl Pts',(-4.06171245250289,6.38125629653729,-42.8179173506464));
#23268=CARTESIAN_POINT('Ctrl Pts',(-6.59932549569553,3.69686934726893,-42.7001427449793));
#23269=CARTESIAN_POINT('Ctrl Pts',(-7.56312229154544,0.130847896591264,
-42.5823681393121));
#23270=CARTESIAN_POINT('Ctrl Pts',(-6.7232552507141,-3.46637834095748,-42.4645935336451));
#23271=CARTESIAN_POINT('Ctrl Pts',(-4.2800170236141,-6.23693789022203,-42.3468189279779));
#23272=CARTESIAN_POINT('Ctrl Pts',(-0.816074432854366,-7.5201038881757,
-42.2290443223108));
#23273=CARTESIAN_POINT('Ctrl Pts',(2.84248671434799,-7.00986513762347,-42.1112697166436));
#23274=CARTESIAN_POINT('Ctrl Pts',(5.82316770897799,-4.82790407962191,-41.9934951109766));
#23275=CARTESIAN_POINT('Ctrl Pts',(7.415131635876,-1.49457779708679,-41.8757205053093));
#23276=CARTESIAN_POINT('Ctrl Pts',(7.23872474179556,2.19517746012267,-41.7579458996423));
#23277=CARTESIAN_POINT('Ctrl Pts',(5.33601678617319,5.36142376860771,-41.6401712939751));
#23278=CARTESIAN_POINT('Ctrl Pts',(2.16076818686676,7.24907034119122,-41.522396688308));
#23279=CARTESIAN_POINT('Ctrl Pts',(-1.52978339021372,7.4079486194182,-41.4046220826408));
#23280=CARTESIAN_POINT('Ctrl Pts',(-4.8555101142083,5.80016909233988,-41.2868474769738));
#23281=CARTESIAN_POINT('Ctrl Pts',(-7.0232880884613,2.80915723934978,-41.1690728713066));
#23282=CARTESIAN_POINT('Ctrl Pts',(-7.51614263143352,-0.85178630704034,
-41.0512982656395));
#23283=CARTESIAN_POINT('Ctrl Pts',(-6.21653711187188,-4.30959467997091,
-40.9335236599724));
#23284=CARTESIAN_POINT('Ctrl Pts',(-3.43440324676116,-6.73964496895424,
-40.8157490543052));
#23285=CARTESIAN_POINT('Ctrl Pts',(0.166771842063232,-7.56241542905497,
-40.6979744486381));
#23286=CARTESIAN_POINT('Ctrl Pts',(3.72817495194683,-6.58169062601625,-40.580199842971));
#23287=CARTESIAN_POINT('Ctrl Pts',(6.40047775663446,-4.03135516368146,-40.4624252373039));
#23288=CARTESIAN_POINT('Ctrl Pts',(7.5463857970818,-0.5196165610486,-40.3446506316367));
#23289=CARTESIAN_POINT('Ctrl Pts',(6.89262134313397,3.11604091582377,-40.2268760259696));
#23290=CARTESIAN_POINT('Ctrl Pts',(4.5950950435731,6.00858065681437,-40.1091014203025));
#23291=CARTESIAN_POINT('Ctrl Pts',(1.20172413953307,7.46818579451377,-39.9913268146353));
#23292=CARTESIAN_POINT('Ctrl Pts',(-2.47823559496468,7.14676768229974,-39.8735522089682));
#23293=CARTESIAN_POINT('Ctrl Pts',(-5.56718228628964,5.12097855493816,-39.7557776033011));
#23294=CARTESIAN_POINT('Ctrl Pts',(-7.32845966659239,1.87393139790187,-39.638002997634));
#23295=CARTESIAN_POINT('Ctrl Pts',(-7.34203587670703,-1.82001350381267,
-39.5202283919668));
#23296=CARTESIAN_POINT('Ctrl Pts',(-5.60467324331843,-5.07991907460583,
-39.4024537862997));
#23297=CARTESIAN_POINT('Ctrl Pts',(-2.53070040376012,-7.12835853723164,
-39.2846791806325));
#23298=CARTESIAN_POINT('Ctrl Pts',(1.14679735894242,-7.47681722301901,-39.1669045749655));
#23299=CARTESIAN_POINT('Ctrl Pts',(4.55080530558902,-6.04219422391756,-39.0491299692983));
#23300=CARTESIAN_POINT('Ctrl Pts',(6.86953092556355,-3.16662041167394,-38.9313553636312));
#23301=CARTESIAN_POINT('Ctrl Pts',(7.55000133455977,0.464133404388116,-38.8135807579641));
#23302=CARTESIAN_POINT('Ctrl Pts',(6.42993701079272,3.98420004595123,-38.695806152297));
#23303=CARTESIAN_POINT('Ctrl Pts',(3.77645243922374,6.55410916472519,-38.5780315466298));
#23304=CARTESIAN_POINT('Ctrl Pts',(0.222354280686254,7.5609852891647,-38.4602569409627));
#23305=CARTESIAN_POINT('Ctrl Pts',(-3.38477123339968,6.76470721214373,-38.3424823352955));
#23306=CARTESIAN_POINT('Ctrl Pts',(-6.1846918348333,4.3551724280248,-38.2247077296285));
#23307=CARTESIAN_POINT('Ctrl Pts',(-7.50967859620706,0.907010115506259,
-38.1069331239613));
#23308=CARTESIAN_POINT('Ctrl Pts',(-7.04374684730056,-2.75745722003065,
-37.9891585182942));
#23309=CARTESIAN_POINT('Ctrl Pts',(-4.89801263364484,-5.76432235502473,
-37.871383912627));
#23310=CARTESIAN_POINT('Ctrl Pts',(-1.58419361167746,-7.39650394156935,
-37.7536093069599));
#23311=CARTESIAN_POINT('Ctrl Pts',(2.10742608985921,-7.26475706922933,-37.6358347012928));
#23312=CARTESIAN_POINT('Ctrl Pts',(5.29646390680803,-5.40050090214708,-37.5180600956257));
#23313=CARTESIAN_POINT('Ctrl Pts',(7.22239371279843,-2.24832584639531,-37.4002854899585));
#23314=CARTESIAN_POINT('Ctrl Pts',(7.42591708833791,1.44003309094744,-37.2825108842915));
#23315=CARTESIAN_POINT('Ctrl Pts',(5.85849754427007,4.78497088454414,-37.1647362786242));
#23316=CARTESIAN_POINT('Ctrl Pts',(2.8939353617182,6.98878235496782,-37.0469616729572));
#23317=CARTESIAN_POINT('Ctrl Pts',(-0.760776389984131,7.52589909718257,
-36.92918706729));
#23318=CARTESIAN_POINT('Ctrl Pts',(-4.23405739852132,6.26822959388264,-36.8114124616229));
#23319=CARTESIAN_POINT('Ctrl Pts',(-6.69759403037466,3.51570292801806,-36.6936378559558));
#23320=CARTESIAN_POINT('Ctrl Pts',(-7.56388027176127,-0.0752511404343053,
-36.5758632502887));
#23321=CARTESIAN_POINT('Ctrl Pts',(-6.62631973269411,-3.64826384889705,
-36.4580886446215));
#23322=CARTESIAN_POINT('Ctrl Pts',(-4.10850975262302,-6.35122414179136,
-36.3403140389544));
#23323=CARTESIAN_POINT('Ctrl Pts',(-0.610887698769837,-7.53955488395458,
-36.2225394332872));
#23324=CARTESIAN_POINT('Ctrl Pts',(3.03240140566261,-6.92980327514396,-36.1047648276202));
#23325=CARTESIAN_POINT('Ctrl Pts',(5.95255640869504,-4.66750168184842,-35.986990221953));
#23326=CARTESIAN_POINT('Ctrl Pts',(7.45306200829349,-1.2919271239697,-35.8692156162859));
#23327=CARTESIAN_POINT('Ctrl Pts',(7.17630464094038,2.39141980438688,-35.7514410106187));
#23328=CARTESIAN_POINT('Ctrl Pts',(5.18781717002348,5.50513519372634,-35.6336664049517));
#23329=CARTESIAN_POINT('Ctrl Pts',(3.03777695224176,6.70444440151624,-35.5551500011735));
#23330=CARTESIAN_POINT('Ctrl Pts',(1.88431329769136,7.01430911752138,-35.5158917992845));
#23331=CARTESIAN_POINT('Ctrl Pts',(5.67311119403182,-4.9704240895673,-48.1613694002385));
#23332=CARTESIAN_POINT('Ctrl Pts',(6.49046945968001,-4.03751288464296,-48.1221111983495));
#23333=CARTESIAN_POINT('Ctrl Pts',(7.65539964128684,-1.76167945546099,-48.0435947945714));
#23334=CARTESIAN_POINT('Ctrl Pts',(7.57658030852297,2.07418183546964,-47.9258201889043));
#23335=CARTESIAN_POINT('Ctrl Pts',(5.69100638293687,5.41462253331856,-47.8080455832371));
#23336=CARTESIAN_POINT('Ctrl Pts',(2.44817669517256,7.46414855887019,-47.69027097757));
#23337=CARTESIAN_POINT('Ctrl Pts',(-1.37847007459924,7.73343177171031,-47.5724963719029));
#23338=CARTESIAN_POINT('Ctrl Pts',(-4.87639090386474,6.15852522019922,-47.4547217662358));
#23339=CARTESIAN_POINT('Ctrl Pts',(-7.21137665992263,3.11488093454325,-47.3369471605686));
#23340=CARTESIAN_POINT('Ctrl Pts',(-7.82658663211968,-0.671582729783266,
-47.2191725549015));
#23341=CARTESIAN_POINT('Ctrl Pts',(-6.57529981941811,-4.29789710828696,
-47.1013979492344));
#23342=CARTESIAN_POINT('Ctrl Pts',(-3.75592722750606,-6.89923779537283,
-46.9836233435672));
#23343=CARTESIAN_POINT('Ctrl Pts',(-0.0408355398413912,-7.85524132486851,
-46.8658487379001));
#23344=CARTESIAN_POINT('Ctrl Pts',(3.68399447197226,-6.93791479378349,-46.748074132233));
#23345=CARTESIAN_POINT('Ctrl Pts',(6.53026049474244,-4.36602539937111,-46.6302995265658));
#23346=CARTESIAN_POINT('Ctrl Pts',(7.81918094043847,-0.75291993672486,-46.5125249208988));
#23347=CARTESIAN_POINT('Ctrl Pts',(7.24337235250388,3.03974275920765,-46.3947503152315));
#23348=CARTESIAN_POINT('Ctrl Pts',(4.94015432317192,6.10748348359639,-46.2769757095645));
#23349=CARTESIAN_POINT('Ctrl Pts',(1.45880148191885,7.7187030853753,-46.1592011038973));
#23350=CARTESIAN_POINT('Ctrl Pts',(-2.37044835173991,7.48915574624172,-46.0414264982303));
#23351=CARTESIAN_POINT('Ctrl Pts',(-5.63439039133243,5.47358420527862,-45.9236518925631));
#23352=CARTESIAN_POINT('Ctrl Pts',(-7.55463523896436,2.15266475714294,-45.805877286896));
#23353=CARTESIAN_POINT('Ctrl Pts',(-7.67324025359723,-1.68162515382409,
-45.6881026812288));
#23354=CARTESIAN_POINT('Ctrl Pts',(-5.96192034822138,-5.11487877740758,
-45.5703280755617));
#23355=CARTESIAN_POINT('Ctrl Pts',(-2.82879345423239,-7.32832905519788,
-45.4525534698945));
#23356=CARTESIAN_POINT('Ctrl Pts',(0.978948004729415,-7.79410931092872,
-45.3347788642275));
#23357=CARTESIAN_POINT('Ctrl Pts',(4.55322859317857,-6.40113962709804,-45.2170042585603));
#23358=CARTESIAN_POINT('Ctrl Pts',(7.04164894598002,-3.48161733518369,-45.0992296528932));
#23359=CARTESIAN_POINT('Ctrl Pts',(7.85076714487718,0.268205861347997,-44.9814550472261));
#23360=CARTESIAN_POINT('Ctrl Pts',(6.78762356569012,3.95406695411651,-44.863680441559));
#23361=CARTESIAN_POINT('Ctrl Pts',(4.10575815569019,6.69695670540814,-44.7459058358918));
#23362=CARTESIAN_POINT('Ctrl Pts',(0.444745877225661,7.84274698379562,-44.6281312302247));
#23363=CARTESIAN_POINT('Ctrl Pts',(-3.32233001152318,7.11818814317712,-44.5103566245576));
#23364=CARTESIAN_POINT('Ctrl Pts',(-6.29709205629216,4.69607397532464,-44.3925820188905));
#23365=CARTESIAN_POINT('Ctrl Pts',(-7.77011490124893,1.15403360805785,-44.2748074132233));
#23366=CARTESIAN_POINT('Ctrl Pts',(-7.39011002643621,-2.66322228593577,
-44.1570328075562));
#23367=CARTESIAN_POINT('Ctrl Pts',(-5.24770151857913,-5.84534925552276,
-44.0392582018891));
#23368=CARTESIAN_POINT('Ctrl Pts',(-1.85381391387615,-7.63346927156042,
-43.9214835962219));
#23369=CARTESIAN_POINT('Ctrl Pts',(1.98217379016447,-7.60114900608606,-43.8037089905548));
#23370=CARTESIAN_POINT('Ctrl Pts',(5.34544995451021,-5.75609624059265,-43.6859343848877));
#23371=CARTESIAN_POINT('Ctrl Pts',(7.43393584017472,-2.53832170366637,-43.5681597792206));
#23372=CARTESIAN_POINT('Ctrl Pts',(7.74956645228107,1.2847952945188,-43.4503851735534));
#23373=CARTESIAN_POINT('Ctrl Pts',(6.21706976707235,4.80151253861666,-43.3326105678863));
#23374=CARTESIAN_POINT('Ctrl Pts',(3.2019177079676,7.17315844928449,-43.2148359622191));
#23375=CARTESIAN_POINT('Ctrl Pts',(-0.576832102868098,7.83413963829078,
-43.0970613565521));
#23376=CARTESIAN_POINT('Ctrl Pts',(-4.21801819812791,6.62682439992187,-42.9792867508849));
#23377=CARTESIAN_POINT('Ctrl Pts',(-6.85328549515125,3.83913493759823,-42.8615121452178));
#23378=CARTESIAN_POINT('Ctrl Pts',(-7.85417181384847,0.135883279641968,
-42.7437375395506));
#23379=CARTESIAN_POINT('Ctrl Pts',(-6.98198440431105,-3.59977401028112,
-42.6259629338836));
#23380=CARTESIAN_POINT('Ctrl Pts',(-4.44472372306338,-6.47695222869333,
-42.5081883282163));
#23381=CARTESIAN_POINT('Ctrl Pts',(-0.847479197274412,-7.80949794527952,
-42.3904137225493));
#23382=CARTESIAN_POINT('Ctrl Pts',(2.95187333649589,-7.27962381943069,-42.2726391168821));
#23383=CARTESIAN_POINT('Ctrl Pts',(6.04725904515579,-5.01369496358918,-42.1548645112151));
#23384=CARTESIAN_POINT('Ctrl Pts',(7.70048607511974,-1.55209321692512,-42.0370899055479));
#23385=CARTESIAN_POINT('Ctrl Pts',(7.51729056381565,2.27965386107329,-41.9193152998808));
#23386=CARTESIAN_POINT('Ctrl Pts',(5.54136122947973,5.56774594172155,-41.8015406942136));
#23387=CARTESIAN_POINT('Ctrl Pts',(2.24392042536729,7.5280342900227,-41.6837660885465));
#23388=CARTESIAN_POINT('Ctrl Pts',(-1.58865361705728,7.69302663664625,-41.5659914828794));
#23389=CARTESIAN_POINT('Ctrl Pts',(-5.0423633534925,6.02337537917852,-41.4482168772123));
#23390=CARTESIAN_POINT('Ctrl Pts',(-7.29356332193576,2.91726125262229,-41.3304422715451));
#23391=CARTESIAN_POINT('Ctrl Pts',(-7.80538424860076,-0.884565361538173,
-41.212667665878));
#23392=CARTESIAN_POINT('Ctrl Pts',(-6.45576637288911,-4.47543960810693,
-41.0948930602109));
#23393=CARTESIAN_POINT('Ctrl Pts',(-3.56656842746744,-6.99900484349956,
-40.9771184545437));
#23394=CARTESIAN_POINT('Ctrl Pts',(0.173189676271779,-7.85343774936625,
-40.8593438488766));
#23395=CARTESIAN_POINT('Ctrl Pts',(3.87164526711537,-6.8349719877086,-40.7415692432095));
#23396=CARTESIAN_POINT('Ctrl Pts',(6.64678555409823,-4.18649267824142,-40.6237946375423));
#23397=CARTESIAN_POINT('Ctrl Pts',(7.83679125354391,-0.539612820006756,
-40.5060200318753));
#23398=CARTESIAN_POINT('Ctrl Pts',(7.1578681647512,3.23595464788666,-40.3882454262081));
#23399=CARTESIAN_POINT('Ctrl Pts',(4.77192680244391,6.23980718766658,-40.270470820541));
#23400=CARTESIAN_POINT('Ctrl Pts',(1.24796975387969,7.75558190212311,-40.1526962148738));
#23401=CARTESIAN_POINT('Ctrl Pts',(-2.57360484304297,7.42179474648848,-40.0349216092068));
#23402=CARTESIAN_POINT('Ctrl Pts',(-5.7814226069585,5.31804774206541,-39.9171470035396));
#23403=CARTESIAN_POINT('Ctrl Pts',(-7.61047873265497,1.9460453763837,-39.7993723978725));
#23404=CARTESIAN_POINT('Ctrl Pts',(-7.6245773922708,-1.89005257503884,-39.6815977922054));
#23405=CARTESIAN_POINT('Ctrl Pts',(-5.82035631801311,-5.27540818122188,
-39.5638231865382));
#23406=CARTESIAN_POINT('Ctrl Pts',(-2.62808864041866,-7.40267716743352,
-39.4460485808711));
#23407=CARTESIAN_POINT('Ctrl Pts',(1.19092924133598,-7.76454549148023,-39.328273975204));
#23408=CARTESIAN_POINT('Ctrl Pts',(4.72593267484581,-6.27471429628227,-39.2104993695368));
#23409=CARTESIAN_POINT('Ctrl Pts',(7.13388916509199,-3.28848058034568,-39.0927247638697));
#23410=CARTESIAN_POINT('Ctrl Pts',(7.84054592674062,0.481994520528341,-38.9749501582026));
#23411=CARTESIAN_POINT('Ctrl Pts',(6.67737848050448,4.13752290328889,-38.8571755525354));
#23412=CARTESIAN_POINT('Ctrl Pts',(3.9217806034483,6.80632911674786,-38.7394009468683));
#23413=CARTESIAN_POINT('Ctrl Pts',(0.230911078352757,7.85195257380211,-38.6216263412012));
#23414=CARTESIAN_POINT('Ctrl Pts',(-3.51502643920103,7.0250315499923,-38.5038517355341));
#23415=CARTESIAN_POINT('Ctrl Pts',(-6.4226956029506,4.52277131190652,-38.3860771298669));
#23416=CARTESIAN_POINT('Ctrl Pts',(-7.79867145971248,0.941914332397903,
-38.2683025241998));
#23417=CARTESIAN_POINT('Ctrl Pts',(-7.31480938947604,-2.86357167590268,
-38.1505279185327));
#23418=CARTESIAN_POINT('Ctrl Pts',(-5.08650148551097,-5.98614916188545,
-38.0327533128655));
#23419=CARTESIAN_POINT('Ctrl Pts',(-1.6451576918735,-7.68114153645695,-37.9149787071984));
#23420=CARTESIAN_POINT('Ctrl Pts',(2.1885255793423,-7.54432468603362,-37.7972041015313));
#23421=CARTESIAN_POINT('Ctrl Pts',(5.5002862477075,-5.60832686967428,-37.6794294958642));
#23422=CARTESIAN_POINT('Ctrl Pts',(7.50033107239187,-2.33484754184726,-37.5616548901971));
#23423=CARTESIAN_POINT('Ctrl Pts',(7.71168658113571,1.49544948209707,-37.4438802845299));
#23424=CARTESIAN_POINT('Ctrl Pts',(6.08394846862963,4.96910958235911,-37.3261056788628));
#23425=CARTESIAN_POINT('Ctrl Pts',(3.0053018677901,7.2577297139398,-37.2083310731957));
#23426=CARTESIAN_POINT('Ctrl Pts',(-0.790053135268523,7.81551616969566,
-37.0905564675285));
#23427=CARTESIAN_POINT('Ctrl Pts',(-4.39699544655749,6.50944812224422,-36.9727818618614));
#23428=CARTESIAN_POINT('Ctrl Pts',(-6.95533567039803,3.65099674164618,-36.8550072561943));
#23429=CARTESIAN_POINT('Ctrl Pts',(-7.8549589632052,-0.078147009049392,
-36.7372326505271));
#23430=CARTESIAN_POINT('Ctrl Pts',(-6.88131854383111,-3.78865896741099,
-36.61945804486));
#23431=CARTESIAN_POINT('Ctrl Pts',(-4.26661638567522,-6.59563652615466,
-36.5016834391929));
#23432=CARTESIAN_POINT('Ctrl Pts',(-0.634396319423309,-7.82969746829512,
-36.3839088335257));
#23433=CARTESIAN_POINT('Ctrl Pts',(3.14909646182159,-7.19648095866354,-36.2661342278587));
#23434=CARTESIAN_POINT('Ctrl Pts',(6.18162697405788,-4.84711984515238,-36.1483596221915));
#23435=CARTESIAN_POINT('Ctrl Pts',(7.73987611146271,-1.34164399456718,-36.0305850165244));
#23436=CARTESIAN_POINT('Ctrl Pts',(7.45246836765699,2.48344814464932,-35.9128104108572));
#23437=CARTESIAN_POINT('Ctrl Pts',(5.38745848890295,5.71698777346563,-35.7950358051902));
#23438=CARTESIAN_POINT('Ctrl Pts',(3.15467887405803,6.96244966245852,-35.716519401412));
#23439=CARTESIAN_POINT('Ctrl Pts',(1.9568267999225,7.28423881576552,-35.677261199523));
#23440=CARTESIAN_POINT('Ctrl Pts',(5.88333785345931,-5.15461149865368,-48.322738800477));
#23441=CARTESIAN_POINT('Ctrl Pts',(6.73098470183852,-4.18712970284087,-48.283480598588));
#23442=CARTESIAN_POINT('Ctrl Pts',(7.9390833270329,-1.82696144522583,-48.2049641948099));
#23443=CARTESIAN_POINT('Ctrl Pts',(7.85734321156999,2.15104412556096,-48.0871895891428));
#23444=CARTESIAN_POINT('Ctrl Pts',(5.90189617863205,5.61527046146739,-47.9694149834756));
#23445=CARTESIAN_POINT('Ctrl Pts',(2.53889799266023,7.74074511468116,-47.8516403778085));
#23446=CARTESIAN_POINT('Ctrl Pts',(-1.42955159741667,8.02000706905112,-47.7338657721414));
#23447=CARTESIAN_POINT('Ctrl Pts',(-5.05709375539013,6.38673971128913,-47.6160911664743));
#23448=CARTESIAN_POINT('Ctrl Pts',(-7.47860632865957,3.23030807689722,-47.4983165608071));
#23449=CARTESIAN_POINT('Ctrl Pts',(-8.11661393920319,-0.696469355301917,
-47.38054195514));
#23450=CARTESIAN_POINT('Ctrl Pts',(-6.81895859297162,-4.45716290103025,
-47.2627673494729));
#23451=CARTESIAN_POINT('Ctrl Pts',(-3.89510941644712,-7.1549006344589,-47.1449927438057));
#23452=CARTESIAN_POINT('Ctrl Pts',(-0.0423487693257355,-8.1463304796979,
-47.0272181381386));
#23453=CARTESIAN_POINT('Ctrl Pts',(3.82051107189486,-7.19501087397739,-46.9094435324715));
#23454=CARTESIAN_POINT('Ctrl Pts',(6.77225026050717,-4.52781580031565,-46.7916689268043));
#23455=CARTESIAN_POINT('Ctrl Pts',(8.10893381718392,-0.780820648997262,
-46.6738943211373));
#23456=CARTESIAN_POINT('Ctrl Pts',(7.51178767534443,3.15238553033109,-46.5561197154701));
#23457=CARTESIAN_POINT('Ctrl Pts',(5.12322003524703,6.3338065374466,-46.438345109803));
#23458=CARTESIAN_POINT('Ctrl Pts',(1.51285981989648,8.00473258651715,-46.3205705041358));
#23459=CARTESIAN_POINT('Ctrl Pts',(-2.45828929496978,7.76667898536331,-46.2027958984687));
#23460=CARTESIAN_POINT('Ctrl Pts',(-5.84318218641065,5.67641705716796,-46.0850212928016));
#23461=CARTESIAN_POINT('Ctrl Pts',(-7.83458493061706,2.23243536365556,-45.9672466871344));
#23462=CARTESIAN_POINT('Ctrl Pts',(-7.95758505318363,-1.74394059704502,
-45.8494720814674));
#23463=CARTESIAN_POINT('Ctrl Pts',(-6.18284931571595,-5.30441919746531,
-45.7316974758002));
#23464=CARTESIAN_POINT('Ctrl Pts',(-2.93361914471405,-7.59989259128377,
-45.6139228701331));
#23465=CARTESIAN_POINT('Ctrl Pts',(1.01522456652217,-8.08293311635193,-45.496148264466));
#23466=CARTESIAN_POINT('Ctrl Pts',(4.72195612275012,-6.63834460234152,-45.3783736587988));
#23467=CARTESIAN_POINT('Ctrl Pts',(7.30258906933454,-3.61063451054781,-45.2605990531317));
#23468=CARTESIAN_POINT('Ctrl Pts',(8.14169050145566,0.278144679809618,-45.1428244474646));
#23469=CARTESIAN_POINT('Ctrl Pts',(7.0391503521151,4.10059154326806,-45.0250498417974));
#23470=CARTESIAN_POINT('Ctrl Pts',(4.25790391697829,6.94512367911202,-44.9072752361303));
#23471=CARTESIAN_POINT('Ctrl Pts',(0.461226682354538,8.13337313984082,-44.7895006304633));
#23472=CARTESIAN_POINT('Ctrl Pts',(-3.4454445276943,7.3819645549793,-44.671726024796));
#23473=CARTESIAN_POINT('Ctrl Pts',(-6.53044137412228,4.8700948803433,-44.553951419129));
#23474=CARTESIAN_POINT('Ctrl Pts',(-8.05804955353917,1.19679826081915,-44.4361768134618));
#23475=CARTESIAN_POINT('Ctrl Pts',(-7.66396296013046,-2.761912458812,-44.3184022077947));
#23476=CARTESIAN_POINT('Ctrl Pts',(-5.44216390829645,-6.06195848547551,
-44.2006276021275));
#23477=CARTESIAN_POINT('Ctrl Pts',(-1.92251010067474,-7.91634029063913,
-44.0828529964604));
#23478=CARTESIAN_POINT('Ctrl Pts',(2.05562656767206,-7.8828223434677,-43.9650783907933));
#23479=CARTESIAN_POINT('Ctrl Pts',(5.54353457662299,-5.96939805023741,-43.8473037851262));
#23480=CARTESIAN_POINT('Ctrl Pts',(7.70941281297271,-2.63238347578102,-43.729529179459));
#23481=CARTESIAN_POINT('Ctrl Pts',(8.03673964729766,1.33240554109725,-43.611754573792));
#23482=CARTESIAN_POINT('Ctrl Pts',(6.4474537246324,4.97944064661048,-43.4939799681247));
#23483=CARTESIAN_POINT('Ctrl Pts',(3.32057014407989,7.43897187806474,-43.3762053624577));
#23484=CARTESIAN_POINT('Ctrl Pts',(-0.598207584837165,8.12444683469811,
-43.2584307567905));
#23485=CARTESIAN_POINT('Ctrl Pts',(-4.37432394375293,6.87239250330645,-43.1406561511235));
#23486=CARTESIAN_POINT('Ctrl Pts',(-7.10724549460698,3.98140052792752,-43.0228815454562));
#23487=CARTESIAN_POINT('Ctrl Pts',(-8.14522133615151,0.140918662692672,
-42.9051069397892));
#23488=CARTESIAN_POINT('Ctrl Pts',(-7.24071355790799,-3.73316967960476,
-42.787332334122));
#23489=CARTESIAN_POINT('Ctrl Pts',(-4.60943042251266,-6.71696656716463,
-42.6695577284549));
#23490=CARTESIAN_POINT('Ctrl Pts',(-0.878883961694459,-8.09889200238335,
-42.5517831227878));
#23491=CARTESIAN_POINT('Ctrl Pts',(3.0612599586438,-7.5493825012379,-42.4340085171206));
#23492=CARTESIAN_POINT('Ctrl Pts',(6.27135038133359,-5.19948584755646,-42.3162339114535));
#23493=CARTESIAN_POINT('Ctrl Pts',(7.98584051436349,-1.60960863676344,-42.1984593057864));
#23494=CARTESIAN_POINT('Ctrl Pts',(7.79585638583573,2.3641302620239,-42.0806847001193));
#23495=CARTESIAN_POINT('Ctrl Pts',(5.74670567278627,5.7740681148354,-41.9629100944521));
#23496=CARTESIAN_POINT('Ctrl Pts',(2.3270726638678,7.80699823885416,-41.845135488785));
#23497=CARTESIAN_POINT('Ctrl Pts',(-1.64752384390083,7.97810465387431,-41.7273608831179));
#23498=CARTESIAN_POINT('Ctrl Pts',(-5.22921659277671,6.24658166601716,-41.6095862774508));
#23499=CARTESIAN_POINT('Ctrl Pts',(-7.56383855541021,3.0253652658948,-41.4918116717836));
#23500=CARTESIAN_POINT('Ctrl Pts',(-8.094625865768,-0.917344416036007,-41.3740370661165));
#23501=CARTESIAN_POINT('Ctrl Pts',(-6.69499563390635,-4.64128453624294,
-41.2562624604494));
#23502=CARTESIAN_POINT('Ctrl Pts',(-3.69873360817373,-7.25836471804489,
-41.1384878547822));
#23503=CARTESIAN_POINT('Ctrl Pts',(0.179607510480324,-8.14446006967754,
-41.0207132491151));
#23504=CARTESIAN_POINT('Ctrl Pts',(4.01511558228392,-7.08825334940095,-40.902938643448));
#23505=CARTESIAN_POINT('Ctrl Pts',(6.893093351562,-4.34163019280138,-40.7851640377808));
#23506=CARTESIAN_POINT('Ctrl Pts',(8.12719671000602,-0.559609078964911,
-40.6673894321138));
#23507=CARTESIAN_POINT('Ctrl Pts',(7.42311498636844,3.35586837994955,-40.5496148264466));
#23508=CARTESIAN_POINT('Ctrl Pts',(4.94875856131471,6.47103371851879,-40.4318402207795));
#23509=CARTESIAN_POINT('Ctrl Pts',(1.29421536822631,8.04297800973245,-40.3140656151123));
#23510=CARTESIAN_POINT('Ctrl Pts',(-2.66897409112126,7.69682181067721,-40.1962910094452));
#23511=CARTESIAN_POINT('Ctrl Pts',(-5.99566292762737,5.51511692919266,-40.0785164037781));
#23512=CARTESIAN_POINT('Ctrl Pts',(-7.89249779871756,2.01815935486554,-39.960741798111));
#23513=CARTESIAN_POINT('Ctrl Pts',(-7.90711890783457,-1.960091646265,-39.8429671924438));
#23514=CARTESIAN_POINT('Ctrl Pts',(-6.03603939270779,-5.47089728783792,
-39.7251925867767));
#23515=CARTESIAN_POINT('Ctrl Pts',(-2.7254768770772,-7.67699579763541,-39.6074179811095));
#23516=CARTESIAN_POINT('Ctrl Pts',(1.23506112372953,-8.05227375994144,-39.4896433754425));
#23517=CARTESIAN_POINT('Ctrl Pts',(4.90106004410261,-6.50723436864699,-39.3718687697753));
#23518=CARTESIAN_POINT('Ctrl Pts',(7.39824740462043,-3.41034074901742,-39.2540941641082));
#23519=CARTESIAN_POINT('Ctrl Pts',(8.13109051892145,0.49985563666857,-39.1363195584411));
#23520=CARTESIAN_POINT('Ctrl Pts',(6.92481995021625,4.29084576062654,-39.0185449527739));
#23521=CARTESIAN_POINT('Ctrl Pts',(4.06710876767287,7.05854906877053,-38.9007703471068));
#23522=CARTESIAN_POINT('Ctrl Pts',(0.239467876019258,8.14291985843953,-38.7829957414397));
#23523=CARTESIAN_POINT('Ctrl Pts',(-3.64528164500238,7.28535588784087,-38.6652211357726));
#23524=CARTESIAN_POINT('Ctrl Pts',(-6.66069937106789,4.69037019578824,-38.5474465301054));
#23525=CARTESIAN_POINT('Ctrl Pts',(-8.0876643232179,0.976818549289544,-38.4296719244383));
#23526=CARTESIAN_POINT('Ctrl Pts',(-7.58587193165152,-2.96968613177471,
-38.3118973187712));
#23527=CARTESIAN_POINT('Ctrl Pts',(-5.2749903373771,-6.20797596874618,-38.194122713104));
#23528=CARTESIAN_POINT('Ctrl Pts',(-1.70612177206955,-7.96577913134455,
-38.0763481074369));
#23529=CARTESIAN_POINT('Ctrl Pts',(2.26962506882539,-7.82389230283792,-37.9585735017698));
#23530=CARTESIAN_POINT('Ctrl Pts',(5.70410858860697,-5.81615283720149,-37.8407988961027));
#23531=CARTESIAN_POINT('Ctrl Pts',(7.77826843198531,-2.4213692372992,-37.7230242904356));
#23532=CARTESIAN_POINT('Ctrl Pts',(7.99745607393352,1.55086587324671,-37.6052496847684));
#23533=CARTESIAN_POINT('Ctrl Pts',(6.30939939298919,5.15324828017407,-37.4874750791013));
#23534=CARTESIAN_POINT('Ctrl Pts',(3.11666837386201,7.52667707291178,-37.3697004734342));
#23535=CARTESIAN_POINT('Ctrl Pts',(-0.819329880552923,8.10513324220875,
-37.251925867767));
#23536=CARTESIAN_POINT('Ctrl Pts',(-4.55993349459366,6.7506666506058,-37.1341512620999));
#23537=CARTESIAN_POINT('Ctrl Pts',(-7.2130773104214,3.78629055527431,-37.0163766564328));
#23538=CARTESIAN_POINT('Ctrl Pts',(-8.14603765464913,-0.0810428776644847,
-36.8986020507657));
#23539=CARTESIAN_POINT('Ctrl Pts',(-7.13631735496811,-3.92905408592493,
-36.7808274450985));
#23540=CARTESIAN_POINT('Ctrl Pts',(-4.42472301872742,-6.84004891051797,
-36.6630528394314));
#23541=CARTESIAN_POINT('Ctrl Pts',(-0.657904940076782,-8.11984005263565,
-36.5452782337643));
#23542=CARTESIAN_POINT('Ctrl Pts',(3.26579151798057,-7.46315864218313,-36.4275036280972));
#23543=CARTESIAN_POINT('Ctrl Pts',(6.41069753942071,-5.02673800845634,-36.30972902243));
#23544=CARTESIAN_POINT('Ctrl Pts',(8.02669021463193,-1.39136086516467,-36.1919544167629));
#23545=CARTESIAN_POINT('Ctrl Pts',(7.72863209437362,2.57547648491176,-36.0741798110958));
#23546=CARTESIAN_POINT('Ctrl Pts',(5.58709980778241,5.92884035320494,-35.9564052054286));
#23547=CARTESIAN_POINT('Ctrl Pts',(3.2715807958743,7.22045492340081,-35.8778888016505));
#23548=CARTESIAN_POINT('Ctrl Pts',(2.02934030215363,7.55416851400967,-35.8386305997615));
#23549=CARTESIAN_POINT('Ctrl Pts',(6.09356451288681,-5.33879890774007,-48.4841082007155));
#23550=CARTESIAN_POINT('Ctrl Pts',(6.97149994399703,-4.33674652103877,-48.4448499988265));
#23551=CARTESIAN_POINT('Ctrl Pts',(8.22276701277896,-1.89224343499068,-48.3663335950484));
#23552=CARTESIAN_POINT('Ctrl Pts',(8.13810611461702,2.22790641565228,-48.2485589893812));
#23553=CARTESIAN_POINT('Ctrl Pts',(6.11278597432722,5.81591838961622,-48.1307843837142));
#23554=CARTESIAN_POINT('Ctrl Pts',(2.6296192901479,8.01734167049212,-48.0130097780469));
#23555=CARTESIAN_POINT('Ctrl Pts',(-1.4806331202341,8.30658236639193,-47.8952351723799));
#23556=CARTESIAN_POINT('Ctrl Pts',(-5.23779660691551,6.61495420237904,-47.7774605667127));
#23557=CARTESIAN_POINT('Ctrl Pts',(-7.74583599739651,3.34573521925119,-47.6596859610457));
#23558=CARTESIAN_POINT('Ctrl Pts',(-8.40664124628672,-0.721355980820569,
-47.5419113553785));
#23559=CARTESIAN_POINT('Ctrl Pts',(-7.06261736652514,-4.61642869377352,
-47.4241367497114));
#23560=CARTESIAN_POINT('Ctrl Pts',(-4.03429160538818,-7.41056347354498,
-47.3063621440442));
#23561=CARTESIAN_POINT('Ctrl Pts',(-0.04386199881008,-8.4374196345273,-47.1885875383771));
#23562=CARTESIAN_POINT('Ctrl Pts',(3.95702767181747,-7.45210695417129,-47.07081293271));
#23563=CARTESIAN_POINT('Ctrl Pts',(7.0142400262719,-4.68960620126019,-46.9530383270429));
#23564=CARTESIAN_POINT('Ctrl Pts',(8.39868669392937,-0.808721361269664,
-46.8352637213757));
#23565=CARTESIAN_POINT('Ctrl Pts',(7.78020299818498,3.26502830145453,-46.7174891157086));
#23566=CARTESIAN_POINT('Ctrl Pts',(5.30628574732215,6.56012959129681,-46.5997145100415));
#23567=CARTESIAN_POINT('Ctrl Pts',(1.56691815787412,8.290762087659,-46.4819399043743));
#23568=CARTESIAN_POINT('Ctrl Pts',(-2.54613023819965,8.04420222448489,-46.3641652987072));
#23569=CARTESIAN_POINT('Ctrl Pts',(-6.05197398148885,5.87924990905731,-46.2463906930401));
#23570=CARTESIAN_POINT('Ctrl Pts',(-8.11453462226977,2.31220597016818,-46.1286160873729));
#23571=CARTESIAN_POINT('Ctrl Pts',(-8.24192985277003,-1.80625604026594,
-46.0108414817058));
#23572=CARTESIAN_POINT('Ctrl Pts',(-6.40377828321054,-5.49395961752304,
-45.8930668760387));
#23573=CARTESIAN_POINT('Ctrl Pts',(-3.03844483519571,-7.87145612736966,
-45.7752922703716));
#23574=CARTESIAN_POINT('Ctrl Pts',(1.05150112831493,-8.37175692177514,-45.6575176647045));
#23575=CARTESIAN_POINT('Ctrl Pts',(4.89068365232167,-6.87554957758499,-45.5397430590373));
#23576=CARTESIAN_POINT('Ctrl Pts',(7.56352919268905,-3.73965168591192,-45.4219684533702));
#23577=CARTESIAN_POINT('Ctrl Pts',(8.43261385803414,0.288083498271241,-45.3041938477031));
#23578=CARTESIAN_POINT('Ctrl Pts',(7.29067713854007,4.2471161324196,-45.1864192420359));
#23579=CARTESIAN_POINT('Ctrl Pts',(4.41004967826638,7.19329065281592,-45.0686446363688));
#23580=CARTESIAN_POINT('Ctrl Pts',(0.477707487483417,8.42399929588601,-44.9508700307017));
#23581=CARTESIAN_POINT('Ctrl Pts',(-3.56855904386543,7.64574096678149,-44.8330954250346));
#23582=CARTESIAN_POINT('Ctrl Pts',(-6.76379069195239,5.04411578536195,-44.7153208193674));
#23583=CARTESIAN_POINT('Ctrl Pts',(-8.3459842058294,1.23956291358046,-44.5975462137003));
#23584=CARTESIAN_POINT('Ctrl Pts',(-7.93781589382472,-2.86060263168824,
-44.4797716080332));
#23585=CARTESIAN_POINT('Ctrl Pts',(-5.63662629801377,-6.27856771542826,
-44.3619970023661));
#23586=CARTESIAN_POINT('Ctrl Pts',(-1.99120628747333,-8.19921130971783,
-44.2442223966989));
#23587=CARTESIAN_POINT('Ctrl Pts',(2.12907934517964,-8.16449568084935,-44.1264477910318));
#23588=CARTESIAN_POINT('Ctrl Pts',(5.74161919873576,-6.18269985988217,-44.0086731853647));
#23589=CARTESIAN_POINT('Ctrl Pts',(7.98488978577069,-2.72644524789567,-43.8908985796975));
#23590=CARTESIAN_POINT('Ctrl Pts',(8.32391284231425,1.38001578767571,-43.7731239740304));
#23591=CARTESIAN_POINT('Ctrl Pts',(6.67783768219246,5.1573687546043,-43.6553493683633));
#23592=CARTESIAN_POINT('Ctrl Pts',(3.43922258019218,7.70478530684499,-43.5375747626961));
#23593=CARTESIAN_POINT('Ctrl Pts',(-0.619583066806221,8.41475403110543,
-43.4198001570291));
#23594=CARTESIAN_POINT('Ctrl Pts',(-4.53062968937796,7.11796060669102,-43.3020255513619));
#23595=CARTESIAN_POINT('Ctrl Pts',(-7.36120549406269,4.12366611825681,-43.1842509456948));
#23596=CARTESIAN_POINT('Ctrl Pts',(-8.43627085845454,0.145954045743379,
-43.0664763400276));
#23597=CARTESIAN_POINT('Ctrl Pts',(-7.49944271150493,-3.86656534892841,
-42.9487017343606));
#23598=CARTESIAN_POINT('Ctrl Pts',(-4.77413712196194,-6.95698090563593,
-42.8309271286933));
#23599=CARTESIAN_POINT('Ctrl Pts',(-0.910288726114504,-8.38828605948718,
-42.7131525230263));
#23600=CARTESIAN_POINT('Ctrl Pts',(3.17064658079171,-7.8191411830451,-42.5953779173591));
#23601=CARTESIAN_POINT('Ctrl Pts',(6.49544171751139,-5.38527673152374,-42.477603311692));
#23602=CARTESIAN_POINT('Ctrl Pts',(8.27119495360724,-1.66712405660176,-42.3598287060249));
#23603=CARTESIAN_POINT('Ctrl Pts',(8.07442220785581,2.44860666297451,-42.2420541003577));
#23604=CARTESIAN_POINT('Ctrl Pts',(5.95205011609281,5.98039028794925,-42.1242794946906));
#23605=CARTESIAN_POINT('Ctrl Pts',(2.41022490236832,8.08596218768562,-42.0065048890235));
#23606=CARTESIAN_POINT('Ctrl Pts',(-1.70639407074438,8.26318267110237,-41.8887302833564));
#23607=CARTESIAN_POINT('Ctrl Pts',(-5.41606983206093,6.46978795285578,-41.7709556776892));
#23608=CARTESIAN_POINT('Ctrl Pts',(-7.83411378888465,3.13346927916731,-41.6531810720221));
#23609=CARTESIAN_POINT('Ctrl Pts',(-8.38386748293525,-0.950123470533844,
-41.535406466355));
#23610=CARTESIAN_POINT('Ctrl Pts',(-6.93422489492358,-4.80712946437895,
-41.4176318606879));
#23611=CARTESIAN_POINT('Ctrl Pts',(-3.83089878888002,-7.51772459259022,
-41.2998572550207));
#23612=CARTESIAN_POINT('Ctrl Pts',(0.186025344688875,-8.43548238998882,
-41.1820826493536));
#23613=CARTESIAN_POINT('Ctrl Pts',(4.15858589745246,-7.3415347110933,-41.0643080436865));
#23614=CARTESIAN_POINT('Ctrl Pts',(7.13940114902576,-4.49676770736134,-40.9465334380193));
#23615=CARTESIAN_POINT('Ctrl Pts',(8.41760216646814,-0.579605337923066,
-40.8287588323522));
#23616=CARTESIAN_POINT('Ctrl Pts',(7.68836180798567,3.47578211201243,-40.7109842266851));
#23617=CARTESIAN_POINT('Ctrl Pts',(5.12559032018552,6.70226024937101,-40.593209621018));
#23618=CARTESIAN_POINT('Ctrl Pts',(1.34046098257293,8.33037411734177,-40.4754350153508));
#23619=CARTESIAN_POINT('Ctrl Pts',(-2.76434333919955,7.97184887486595,-40.3576604096838));
#23620=CARTESIAN_POINT('Ctrl Pts',(-6.20990324829623,5.71218611631991,-40.2398858040166));
#23621=CARTESIAN_POINT('Ctrl Pts',(-8.17451686478015,2.09027333334737,-40.1221111983495));
#23622=CARTESIAN_POINT('Ctrl Pts',(-8.18966042339832,-2.03013071749117,
-40.0043365926823));
#23623=CARTESIAN_POINT('Ctrl Pts',(-6.25172246740249,-5.66638639445397,
-39.8865619870152));
#23624=CARTESIAN_POINT('Ctrl Pts',(-2.82286511373573,-7.95131442783728,
-39.768787381348));
#23625=CARTESIAN_POINT('Ctrl Pts',(1.27919300612309,-8.34000202840266,-39.651012775681));
#23626=CARTESIAN_POINT('Ctrl Pts',(5.07618741335941,-6.73975444101172,-39.5332381700138));
#23627=CARTESIAN_POINT('Ctrl Pts',(7.66260564414886,-3.53220091768916,-39.4154635643467));
#23628=CARTESIAN_POINT('Ctrl Pts',(8.42163511110229,0.517716752808797,-39.2976889586796));
#23629=CARTESIAN_POINT('Ctrl Pts',(7.17226141992802,4.4441686179642,-39.1799143530125));
#23630=CARTESIAN_POINT('Ctrl Pts',(4.21243693189744,7.31076902079321,-39.0621397473453));
#23631=CARTESIAN_POINT('Ctrl Pts',(0.248024673685762,8.43388714307694,-38.9443651416782));
#23632=CARTESIAN_POINT('Ctrl Pts',(-3.77553685080373,7.54568022568945,-38.8265905360111));
#23633=CARTESIAN_POINT('Ctrl Pts',(-6.89870313918519,4.85796907966996,-38.7088159303439));
#23634=CARTESIAN_POINT('Ctrl Pts',(-8.37665718672332,1.01172276618119,-38.5910413246768));
#23635=CARTESIAN_POINT('Ctrl Pts',(-7.856934473827,-3.07580058764674,-38.4732667190097));
#23636=CARTESIAN_POINT('Ctrl Pts',(-5.46347918924325,-6.4298027756069,-38.3554921133425));
#23637=CARTESIAN_POINT('Ctrl Pts',(-1.76708585226559,-8.25041672623214,
-38.2377175076754));
#23638=CARTESIAN_POINT('Ctrl Pts',(2.35072455830847,-8.10345991964222,-38.1199429020083));
#23639=CARTESIAN_POINT('Ctrl Pts',(5.90793092950644,-6.02397880472869,-38.0021682963412));
#23640=CARTESIAN_POINT('Ctrl Pts',(8.05620579157874,-2.50789093275115,-37.8843936906741));
#23641=CARTESIAN_POINT('Ctrl Pts',(8.28322556673132,1.60628226439634,-37.7666190850069));
#23642=CARTESIAN_POINT('Ctrl Pts',(6.53485031734875,5.33738697798904,-37.6488444793398));
#23643=CARTESIAN_POINT('Ctrl Pts',(3.22803487993391,7.79562443188376,-37.5310698736727));
#23644=CARTESIAN_POINT('Ctrl Pts',(-0.848606625837317,8.39475031472183,
-37.4132952680055));
#23645=CARTESIAN_POINT('Ctrl Pts',(-4.72287154262983,6.99188517896739,-37.2955206623384));
#23646=CARTESIAN_POINT('Ctrl Pts',(-7.47081895044476,3.92158436890243,-37.1777460566712));
#23647=CARTESIAN_POINT('Ctrl Pts',(-8.43711634609307,-0.0839387462795732,
-37.0599714510042));
#23648=CARTESIAN_POINT('Ctrl Pts',(-7.39131616610511,-4.06944920443886,
-36.942196845337));
#23649=CARTESIAN_POINT('Ctrl Pts',(-4.58282965177962,-7.08446129488128,
-36.8244222396699));
#23650=CARTESIAN_POINT('Ctrl Pts',(-0.681413560730255,-8.40998263697618,
-36.7066476340027));
#23651=CARTESIAN_POINT('Ctrl Pts',(3.38248657413956,-7.72983632570271,-36.5888730283357));
#23652=CARTESIAN_POINT('Ctrl Pts',(6.63976810478354,-5.20635617176029,-36.4710984226685));
#23653=CARTESIAN_POINT('Ctrl Pts',(8.31350431780115,-1.44107773576215,-36.3533238170014));
#23654=CARTESIAN_POINT('Ctrl Pts',(8.00479582109024,2.66750482517421,-36.2355492113343));
#23655=CARTESIAN_POINT('Ctrl Pts',(5.78674112666189,6.14069293294423,-36.1177746056671));
#23656=CARTESIAN_POINT('Ctrl Pts',(3.38848271769057,7.47846018434309,-36.039258201889));
#23657=CARTESIAN_POINT('Ctrl Pts',(2.10185380438477,7.82409821225381,-36.));
#23658=CARTESIAN_POINT('Ctrl Pts',(2.10185380438477,7.82409821225381,-36.));
#23659=CARTESIAN_POINT('Ctrl Pts',(2.30082749329421,7.7596064443525,-36.));
#23660=CARTESIAN_POINT('Ctrl Pts',(2.49685155452529,7.68738684032504,-36.));
#23661=CARTESIAN_POINT('Ctrl Pts',(2.689555562529,7.60776034250278,-36.));
#23662=CARTESIAN_POINT('Ctrl Pts',(2.88412146665351,7.5273644975925,-36.));
#23663=CARTESIAN_POINT('Ctrl Pts',(3.07530344788642,7.43941759948373,-36.));
#23664=CARTESIAN_POINT('Ctrl Pts',(3.26270123260074,7.3442002249883,-36.));
#23665=CARTESIAN_POINT('Ctrl Pts',(3.45039098213973,7.24883450229285,-36.));
#23666=CARTESIAN_POINT('Ctrl Pts',(3.63428531442281,7.14617523423964,-36.));
#23667=CARTESIAN_POINT('Ctrl Pts',(3.81395427779333,7.0364602726816,-36.));
#23668=CARTESIAN_POINT('Ctrl Pts',(3.99143524378484,6.92808141305137,-36.));
#23669=CARTESIAN_POINT('Ctrl Pts',(4.16479360607289,6.81281720683301,-36.));
#23670=CARTESIAN_POINT('Ctrl Pts',(4.33358005423134,6.69086045395404,-36.));
#23671=CARTESIAN_POINT('Ctrl Pts',(4.43066189457222,6.62071390995915,-36.));
#23672=CARTESIAN_POINT('Ctrl Pts',(4.52623053968623,6.54835265306457,-36.));
#23673=CARTESIAN_POINT('Ctrl Pts',(4.62019422903912,6.47380866470389,-36.));
#23674=CARTESIAN_POINT('Ctrl Pts',(4.66632187332592,6.4372143312704,-36.));
#23675=CARTESIAN_POINT('Ctrl Pts',(4.71206266158868,6.40009392819384,-36.));
#23676=CARTESIAN_POINT('Ctrl Pts',(4.75740528585098,6.36245096836916,-36.));
#23677=CARTESIAN_POINT('Ctrl Pts',(4.77704327692769,6.34614771902784,-36.));
#23678=CARTESIAN_POINT('Ctrl Pts',(4.79660790428669,6.32974532323648,-36.));
#23679=CARTESIAN_POINT('Ctrl Pts',(4.81609406394226,6.31324758769124,-36.));
#23680=CARTESIAN_POINT('Ctrl Pts',(4.97467824697507,6.17898409198058,-36.));
#23681=CARTESIAN_POINT('Ctrl Pts',(5.12764651540678,6.03876779721708,-36.));
#23682=CARTESIAN_POINT('Ctrl Pts',(5.2746131961221,5.89285549710303,-36.));
#23683=CARTESIAN_POINT('Ctrl Pts',(5.32270090376221,5.84511278430017,-36.));
#23684=CARTESIAN_POINT('Ctrl Pts',(5.37014581825667,5.79675992826811,-36.));
#23685=CARTESIAN_POINT('Ctrl Pts',(5.41693362537058,5.74780501532688,-36.));
#23686=CARTESIAN_POINT('Ctrl Pts',(5.55998414133242,5.59812872171345,-36.));
#23687=CARTESIAN_POINT('Ctrl Pts',(5.69689520934925,5.44282686808312,-36.));
#23688=CARTESIAN_POINT('Ctrl Pts',(5.82744384911316,5.28234284303486,-36.));
#23689=CARTESIAN_POINT('Ctrl Pts',(5.95822183969036,5.12157687600901,-36.));
#23690=CARTESIAN_POINT('Ctrl Pts',(6.08261535950187,4.95560987748997,-36.));
#23691=CARTESIAN_POINT('Ctrl Pts',(6.20035566189897,4.78486047060351,-36.));
#23692=CARTESIAN_POINT('Ctrl Pts',(6.31730039604029,4.61526481315583,-36.));
#23693=CARTESIAN_POINT('Ctrl Pts',(6.42768178546486,4.44095051821423,-36.));
#23694=CARTESIAN_POINT('Ctrl Pts',(6.5311881819826,4.26231063676596,-36.));
#23695=CARTESIAN_POINT('Ctrl Pts',(6.57281068005803,4.1904750945007,-36.));
#23696=CARTESIAN_POINT('Ctrl Pts',(6.61332089089221,4.11793994409325,-36.));
#23697=CARTESIAN_POINT('Ctrl Pts',(6.65269617438066,4.04473030956882,-36.));
#23698=CARTESIAN_POINT('Ctrl Pts',(6.66624691189691,4.01953570896632,-36.));
#23699=CARTESIAN_POINT('Ctrl Pts',(6.67966322249545,3.99426122477837,-36.));
#23700=CARTESIAN_POINT('Ctrl Pts',(6.69294414431972,3.96890787749673,-36.));
#23701=CARTESIAN_POINT('Ctrl Pts',(6.70467576680984,3.9465121505205,-36.));
#23702=CARTESIAN_POINT('Ctrl Pts',(6.71630216391417,3.92405397007754,-36.));
#23703=CARTESIAN_POINT('Ctrl Pts',(6.72781502483286,3.90154926003667,-36.));
#23704=CARTESIAN_POINT('Ctrl Pts',(6.82109912412433,3.71920261129266,-36.));
#23705=CARTESIAN_POINT('Ctrl Pts',(6.90705463802017,3.53357359685618,-36.));
#23706=CARTESIAN_POINT('Ctrl Pts',(6.98547179470946,3.34508790000042,-36.));
#23707=CARTESIAN_POINT('Ctrl Pts',(7.06354641293418,3.1574255382912,-36.));
#23708=CARTESIAN_POINT('Ctrl Pts',(7.13414864143153,2.96693075444826,-36.));
#23709=CARTESIAN_POINT('Ctrl Pts',(7.1970241992718,2.77400366738376,-36.));
#23710=CARTESIAN_POINT('Ctrl Pts',(7.23384826254667,2.66101287246235,-36.));
#23711=CARTESIAN_POINT('Ctrl Pts',(7.26802113681645,2.5471874598649,-36.));
#23712=CARTESIAN_POINT('Ctrl Pts',(7.29948362757048,2.43260592056936,-36.));
#23713=CARTESIAN_POINT('Ctrl Pts',(7.3534896782826,2.23592421249213,-36.));
#23714=CARTESIAN_POINT('Ctrl Pts',(7.39951253414964,2.03701441433134,-36.));
#23715=CARTESIAN_POINT('Ctrl Pts',(7.43751281341565,1.83636829928625,-36.));
#23716=CARTESIAN_POINT('Ctrl Pts',(7.46184111046734,1.70791191992879,-36.));
#23717=CARTESIAN_POINT('Ctrl Pts',(7.48288011604595,1.57874381119794,-36.));
#23718=CARTESIAN_POINT('Ctrl Pts',(7.50060831271862,1.44899412782466,-36.));
#23719=CARTESIAN_POINT('Ctrl Pts',(7.50964573314831,1.3828507709501,-36.));
#23720=CARTESIAN_POINT('Ctrl Pts',(7.51782262655261,1.31655630325051,-36.));
#23721=CARTESIAN_POINT('Ctrl Pts',(7.5251352705533,1.25012817277057,-36.));
#23722=CARTESIAN_POINT('Ctrl Pts',(7.52928149862857,1.21246379589706,-36.));
#23723=CARTESIAN_POINT('Ctrl Pts',(7.53314987483263,1.17475645171563,-36.));
#23724=CARTESIAN_POINT('Ctrl Pts',(7.53673963659345,1.13700934710221,-36.));
#23725=CARTESIAN_POINT('Ctrl Pts',(7.5398457973277,1.10434740962724,-36.));
#23726=CARTESIAN_POINT('Ctrl Pts',(7.54274371571818,1.07165049518016,-36.));
#23727=CARTESIAN_POINT('Ctrl Pts',(7.54543050825926,1.03895175486804,-36.));
#23728=CARTESIAN_POINT('Ctrl Pts',(7.56194131066929,0.838012370045629,-36.));
#23729=CARTESIAN_POINT('Ctrl Pts',(7.57050463381881,0.636810188211384,-36.));
#23730=CARTESIAN_POINT('Ctrl Pts',(7.5711535550322,0.435821667465856,-36.));
#23731=CARTESIAN_POINT('Ctrl Pts',(7.57180236612707,0.234867253413772,-36.));
#23732=CARTESIAN_POINT('Ctrl Pts',(7.56453941489479,0.03412571703456,-36.));
#23733=CARTESIAN_POINT('Ctrl Pts',(7.54934569594904,-0.165927099754431,
-36.));
#23734=CARTESIAN_POINT('Ctrl Pts',(7.53434530981631,-0.363434340048337,
-36.));
#23735=CARTESIAN_POINT('Ctrl Pts',(7.51161456525456,-0.560270924380012,
-36.));
#23736=CARTESIAN_POINT('Ctrl Pts',(7.48108594581124,-0.755969235382515,
-36.));
#23737=CARTESIAN_POINT('Ctrl Pts',(7.45371072786321,-0.931453224290022,
-36.));
#23738=CARTESIAN_POINT('Ctrl Pts',(7.42006472051527,-1.10602214252325,-36.));
#23739=CARTESIAN_POINT('Ctrl Pts',(7.3800660535423,-1.27932570484005,-36.));
#23740=CARTESIAN_POINT('Ctrl Pts',(7.34592028888866,-1.42727020150302,-36.));
#23741=CARTESIAN_POINT('Ctrl Pts',(7.30714422290839,-1.5742924439295,-36.));
#23742=CARTESIAN_POINT('Ctrl Pts',(7.26380602496235,-1.72018741510414,-36.));
#23743=CARTESIAN_POINT('Ctrl Pts',(7.25535126498663,-1.74864976521113,-36.));
#23744=CARTESIAN_POINT('Ctrl Pts',(7.24672283231802,-1.77706917955542,-36.));
#23745=CARTESIAN_POINT('Ctrl Pts',(7.23792117432662,-1.80544408661968,-36.));
#23746=CARTESIAN_POINT('Ctrl Pts',(7.23013840559116,-1.83053428437413,-36.));
#23747=CARTESIAN_POINT('Ctrl Pts',(7.22222273184584,-1.85558146827501,-36.));
#23748=CARTESIAN_POINT('Ctrl Pts',(7.21417570637184,-1.88058164144947,-36.));
#23749=CARTESIAN_POINT('Ctrl Pts',(7.15325531511497,-2.06984664827677,-36.));
#23750=CARTESIAN_POINT('Ctrl Pts',(7.08479320734585,-2.25647542918358,-36.));
#23751=CARTESIAN_POINT('Ctrl Pts',(7.00902681125197,-2.44004188332158,-36.));
#23752=CARTESIAN_POINT('Ctrl Pts',(6.93177164355565,-2.62721532602142,-36.));
#23753=CARTESIAN_POINT('Ctrl Pts',(6.84692207561124,-2.81120566590633,-36.));
#23754=CARTESIAN_POINT('Ctrl Pts',(6.75468151121674,-2.99153375862684,-36.));
#23755=CARTESIAN_POINT('Ctrl Pts',(6.71535300589298,-3.06842004397361,-36.));
#23756=CARTESIAN_POINT('Ctrl Pts',(6.67468031908831,-3.14464016518226,-36.));
#23757=CARTESIAN_POINT('Ctrl Pts',(6.63267679451784,-3.22015498690596,-36.));
#23758=CARTESIAN_POINT('Ctrl Pts',(6.60409277041902,-3.27154394785723,-36.));
#23759=CARTESIAN_POINT('Ctrl Pts',(6.57489240539613,-3.32260625824744,-36.));
#23760=CARTESIAN_POINT('Ctrl Pts',(6.54507954995881,-3.3733292184608,-36.));
#23761=CARTESIAN_POINT('Ctrl Pts',(6.52647860828883,-3.40497646628117,-36.));
#23762=CARTESIAN_POINT('Ctrl Pts',(6.50763779811667,-3.43649380740715,-36.));
#23763=CARTESIAN_POINT('Ctrl Pts',(6.4885706896475,-3.46785768454478,-36.));
#23764=CARTESIAN_POINT('Ctrl Pts',(6.38641008318404,-3.63590375794958,-36.));
#23765=CARTESIAN_POINT('Ctrl Pts',(6.27768402389073,-3.79967230920287,-36.));
#23766=CARTESIAN_POINT('Ctrl Pts',(6.16259229716626,-3.95873109508268,-36.));
#23767=CARTESIAN_POINT('Ctrl Pts',(6.04877580733772,-4.11602748119538,-36.));
#23768=CARTESIAN_POINT('Ctrl Pts',(5.92873351593867,-4.26871840542356,-36.));
#23769=CARTESIAN_POINT('Ctrl Pts',(5.80262143415048,-4.41635115060161,-36.));
#23770=CARTESIAN_POINT('Ctrl Pts',(5.77983952847348,-4.44302072284079,-36.));
#23771=CARTESIAN_POINT('Ctrl Pts',(5.75685945345182,-4.46952512396077,-36.));
#23772=CARTESIAN_POINT('Ctrl Pts',(5.73368201345117,-4.49586154264461,-36.));
#23773=CARTESIAN_POINT('Ctrl Pts',(5.64631446617484,-4.59513688558089,-36.));
#23774=CARTESIAN_POINT('Ctrl Pts',(5.55614292429607,-4.69202604818322,-36.));
#23775=CARTESIAN_POINT('Ctrl Pts',(5.46328275624301,-4.78643223329955,-36.));
#23776=CARTESIAN_POINT('Ctrl Pts',(5.46288453460432,-4.78623668048091,-48.));
#23777=CARTESIAN_POINT('Ctrl Pts',(5.59774281609631,-4.64891404164603,-48.));
#23778=CARTESIAN_POINT('Ctrl Pts',(5.72676707811106,-4.50639591331986,-48.));
#23779=CARTESIAN_POINT('Ctrl Pts',(5.84982506430564,-4.35916096560483,-48.));
#23780=CARTESIAN_POINT('Ctrl Pts',(5.97480997239641,-4.20962051742283,-48.));
#23781=CARTESIAN_POINT('Ctrl Pts',(6.09364072129775,-4.05521394491186,-48.));
#23782=CARTESIAN_POINT('Ctrl Pts',(6.20615004774937,-3.89639687941618,-48.));
#23783=CARTESIAN_POINT('Ctrl Pts',(6.3253334379493,-3.72815877076906,-48.));
#23784=CARTESIAN_POINT('Ctrl Pts',(6.437424033659,-3.55497113855592,-48.));
#23785=CARTESIAN_POINT('Ctrl Pts',(6.54218080780119,-3.37732938918555,-48.));
#23786=CARTESIAN_POINT('Ctrl Pts',(6.64196722139062,-3.20811615005545,-48.));
#23787=CARTESIAN_POINT('Ctrl Pts',(6.73509931029878,-3.03486055006183,-48.));
#23788=CARTESIAN_POINT('Ctrl Pts',(6.82132597032137,-2.85795972896024,-48.));
#23789=CARTESIAN_POINT('Ctrl Pts',(6.86766051232553,-2.76290074692666,-48.));
#23790=CARTESIAN_POINT('Ctrl Pts',(6.91200033896626,-2.66678873196007,-48.));
#23791=CARTESIAN_POINT('Ctrl Pts',(6.95430087098005,-2.56968260604186,-48.));
#23792=CARTESIAN_POINT('Ctrl Pts',(6.97457089805417,-2.52315024089848,-48.));
#23793=CARTESIAN_POINT('Ctrl Pts',(6.99437259374271,-2.47638958030327,-48.));
#23794=CARTESIAN_POINT('Ctrl Pts',(7.01370070790936,-2.4294069894874,-48.));
#23795=CARTESIAN_POINT('Ctrl Pts',(7.02151887657497,-2.41040266158564,-48.));
#23796=CARTESIAN_POINT('Ctrl Pts',(7.02925902870664,-2.39136323223209,-48.));
#23797=CARTESIAN_POINT('Ctrl Pts',(7.03691728406108,-2.37229819353851,-48.));
#23798=CARTESIAN_POINT('Ctrl Pts',(7.11159745538058,-2.18638374044777,-48.));
#23799=CARTESIAN_POINT('Ctrl Pts',(7.17858966450582,-1.99780302602708,-48.));
#23800=CARTESIAN_POINT('Ctrl Pts',(7.23771290858855,-1.80701588371416,-48.));
#23801=CARTESIAN_POINT('Ctrl Pts',(7.25137618887209,-1.76292530241471,-48.));
#23802=CARTESIAN_POINT('Ctrl Pts',(7.26461905057976,-1.71871673873425,-48.));
#23803=CARTESIAN_POINT('Ctrl Pts',(7.27743895299859,-1.67439562023028,-48.));
#23804=CARTESIAN_POINT('Ctrl Pts',(7.33236359165557,-1.48450950884079,-48.));
#23805=CARTESIAN_POINT('Ctrl Pts',(7.37952838594581,-1.29255934235065,-48.));
#23806=CARTESIAN_POINT('Ctrl Pts',(7.41900439368324,-1.09903098681805,-48.));
#23807=CARTESIAN_POINT('Ctrl Pts',(7.45887410032125,-0.90357255007484,-48.));
#23808=CARTESIAN_POINT('Ctrl Pts',(7.49090103834248,-0.706503641732061,
-48.));
#23809=CARTESIAN_POINT('Ctrl Pts',(7.51510880906928,-0.508305269117967,
-48.));
#23810=CARTESIAN_POINT('Ctrl Pts',(7.53937115123289,-0.30966009906489,-48.));
#23811=CARTESIAN_POINT('Ctrl Pts',(7.55577912898259,-0.109879669117689,
-48.));
#23812=CARTESIAN_POINT('Ctrl Pts',(7.56430520033345,0.0905611110017474,
-48.));
#23813=CARTESIAN_POINT('Ctrl Pts',(7.56775652782499,0.171698923058889,-48.));
#23814=CARTESIAN_POINT('Ctrl Pts',(7.56991572882259,0.252944988440767,-48.));
#23815=CARTESIAN_POINT('Ctrl Pts',(7.57077853657819,0.334267836558012,-48.));
#23816=CARTESIAN_POINT('Ctrl Pts',(7.57111603563457,0.366078381055583,-48.));
#23817=CARTESIAN_POINT('Ctrl Pts',(7.57125515949273,0.397900673006978,-48.));
#23818=CARTESIAN_POINT('Ctrl Pts',(7.5711955934687,0.429732823440462,-48.));
#23819=CARTESIAN_POINT('Ctrl Pts',(7.57115223714762,0.45290249032953,-48.));
#23820=CARTESIAN_POINT('Ctrl Pts',(7.57100362858594,0.476067922578518,-48.));
#23821=CARTESIAN_POINT('Ctrl Pts',(7.57074992211655,0.499226939952169,-48.));
#23822=CARTESIAN_POINT('Ctrl Pts',(7.56852821147751,0.702030736842373,-48.));
#23823=CARTESIAN_POINT('Ctrl Pts',(7.55825105142857,0.904377024570949,-48.));
#23824=CARTESIAN_POINT('Ctrl Pts',(7.53999284572521,1.10576747908613,-48.));
#23825=CARTESIAN_POINT('Ctrl Pts',(7.52160273684829,1.30861284327355,-48.));
#23826=CARTESIAN_POINT('Ctrl Pts',(7.49511595853735,1.51048921493983,-48.));
#23827=CARTESIAN_POINT('Ctrl Pts',(7.46055733584223,1.71089962196904,-48.));
#23828=CARTESIAN_POINT('Ctrl Pts',(7.44239810129864,1.81620762623544,-48.));
#23829=CARTESIAN_POINT('Ctrl Pts',(7.42200928932642,1.92111100147053,-48.));
#23830=CARTESIAN_POINT('Ctrl Pts',(7.39938874174189,2.02553797493781,-48.));
#23831=CARTESIAN_POINT('Ctrl Pts',(7.35650614536241,2.22350399400051,-48.));
#23832=CARTESIAN_POINT('Ctrl Pts',(7.30560625006247,2.41975857637032,-48.));
#23833=CARTESIAN_POINT('Ctrl Pts',(7.2469351304453,2.61389361700967,-48.));
#23834=CARTESIAN_POINT('Ctrl Pts',(7.20801060017588,2.74268978307958,-48.));
#23835=CARTESIAN_POINT('Ctrl Pts',(7.16566449045406,2.8705529273773,-48.));
#23836=CARTESIAN_POINT('Ctrl Pts',(7.11995645101958,2.9973606630013,-48.));
#23837=CARTESIAN_POINT('Ctrl Pts',(7.09565931107824,3.06476817678271,-48.));
#23838=CARTESIAN_POINT('Ctrl Pts',(7.0704120324254,3.13187741049653,-48.));
#23839=CARTESIAN_POINT('Ctrl Pts',(7.04422251139379,3.19866954231277,-48.));
#23840=CARTESIAN_POINT('Ctrl Pts',(7.02727232497963,3.24189824756163,-48.));
#23841=CARTESIAN_POINT('Ctrl Pts',(7.00992743343007,3.28499411728753,-48.));
#23842=CARTESIAN_POINT('Ctrl Pts',(6.99218981795071,3.32795196703053,-48.));
#23843=CARTESIAN_POINT('Ctrl Pts',(6.98238546444813,3.35169664370825,-48.));
#23844=CARTESIAN_POINT('Ctrl Pts',(6.972464205672,3.37539162567257,-48.));
#23845=CARTESIAN_POINT('Ctrl Pts',(6.96242916936618,3.39903019071691,-48.));
#23846=CARTESIAN_POINT('Ctrl Pts',(6.88204014270503,3.58839485046199,-48.));
#23847=CARTESIAN_POINT('Ctrl Pts',(6.79430434720432,3.77425980468391,-48.));
#23848=CARTESIAN_POINT('Ctrl Pts',(6.6995390662541,3.95622432161017,-48.));
#23849=CARTESIAN_POINT('Ctrl Pts',(6.60408885004849,4.13950402392524,-48.));
#23850=CARTESIAN_POINT('Ctrl Pts',(6.50150693964798,4.31882734921869,-48.));
#23851=CARTESIAN_POINT('Ctrl Pts',(6.39206487423864,4.49377618287241,-48.));
#23852=CARTESIAN_POINT('Ctrl Pts',(6.28276639945468,4.66849547944328,-48.));
#23853=CARTESIAN_POINT('Ctrl Pts',(6.16662546550751,4.83885239762259,-48.));
#23854=CARTESIAN_POINT('Ctrl Pts',(6.04386422543394,5.00441223060582,-48.));
#23855=CARTESIAN_POINT('Ctrl Pts',(5.93619140677786,5.14962332380472,-48.));
#23856=CARTESIAN_POINT('Ctrl Pts',(5.82342482808063,5.2911440803551,-48.));
#23857=CARTESIAN_POINT('Ctrl Pts',(5.70568636114417,5.42866369628278,-48.));
#23858=CARTESIAN_POINT('Ctrl Pts',(5.59912526890868,5.55312803540967,-48.));
#23859=CARTESIAN_POINT('Ctrl Pts',(5.48849099337009,5.67431475663495,-48.));
#23860=CARTESIAN_POINT('Ctrl Pts',(5.3739712089178,5.79208620502323,-48.));
#23861=CARTESIAN_POINT('Ctrl Pts',(5.35469219530606,5.81191262512533,-48.));
#23862=CARTESIAN_POINT('Ctrl Pts',(5.3353030320026,5.8316422195084,-48.));
#23863=CARTESIAN_POINT('Ctrl Pts',(5.31580457648251,5.85127428800012,-48.));
#23864=CARTESIAN_POINT('Ctrl Pts',(5.29758402265168,5.86961969799404,-48.));
#23865=CARTESIAN_POINT('Ctrl Pts',(5.27927476383158,5.88787316488096,-48.));
#23866=CARTESIAN_POINT('Ctrl Pts',(5.26087839653079,5.90603362442133,-48.));
#23867=CARTESIAN_POINT('Ctrl Pts',(5.11313196865418,6.05188541036452,-48.));
#23868=CARTESIAN_POINT('Ctrl Pts',(4.9597563132659,6.19175476807782,-48.));
#23869=CARTESIAN_POINT('Ctrl Pts',(4.80120569678638,6.32542442409823,-48.));
#23870=CARTESIAN_POINT('Ctrl Pts',(4.64119263820284,6.46032702476013,-48.));
#23871=CARTESIAN_POINT('Ctrl Pts',(4.47590823781459,6.58891549829174,-48.));
#23872=CARTESIAN_POINT('Ctrl Pts',(4.30577791160318,6.71093376130789,-48.));
#23873=CARTESIAN_POINT('Ctrl Pts',(4.16782007827905,6.8098777624542,-48.));
#23874=CARTESIAN_POINT('Ctrl Pts',(4.02667489872999,6.90450099949382,-48.));
#23875=CARTESIAN_POINT('Ctrl Pts',(3.88255276675076,6.99464809660295,-48.));
#23876=CARTESIAN_POINT('Ctrl Pts',(3.84870261005292,7.01582106511995,-48.));
#23877=CARTESIAN_POINT('Ctrl Pts',(3.8146849955381,7.03674886278265,-48.));
#23878=CARTESIAN_POINT('Ctrl Pts',(3.78052548102958,7.05741572459137,-48.));
#23879=CARTESIAN_POINT('Ctrl Pts',(3.59938595616017,7.16700702243138,-48.));
#23880=CARTESIAN_POINT('Ctrl Pts',(3.41413884653443,7.26934117499804,-48.));
#23881=CARTESIAN_POINT('Ctrl Pts',(3.2252257455022,7.36416892349042,-48.));
#23882=CARTESIAN_POINT('Ctrl Pts',(3.03641084043487,7.45894738105373,-48.));
#23883=CARTESIAN_POINT('Ctrl Pts',(2.84393319138116,7.5462276669538,-48.));
#23884=CARTESIAN_POINT('Ctrl Pts',(2.6482016111633,7.62572029240467,-48.));
#23885=CARTESIAN_POINT('Ctrl Pts',(2.60498561173223,7.64327164131033,-48.));
#23886=CARTESIAN_POINT('Ctrl Pts',(2.5616108804781,7.66044317667659,-48.));
#23887=CARTESIAN_POINT('Ctrl Pts',(2.51808164906492,7.67723148270866,-48.));
#23888=CARTESIAN_POINT('Ctrl Pts',(2.38090159934801,7.73013893320513,-48.));
#23889=CARTESIAN_POINT('Ctrl Pts',(2.24218744160261,7.77924116547427,-48.));
#23890=CARTESIAN_POINT('Ctrl Pts',(2.10210202563547,7.82452631996428,-48.));
#23891=CARTESIAN_POINT('Ctrl Pts',(-7.26359129981488,-2.41004779799603E-5,
-36.5782382949161));
#23892=CARTESIAN_POINT('Ctrl Pts',(-7.26336357111336,1.16995354780479,-36.6167048152626));
#23893=CARTESIAN_POINT('Ctrl Pts',(-6.97516456706758,2.34003869460332,-36.6551713356092));
#23894=CARTESIAN_POINT('Ctrl Pts',(-6.43138563196355,3.37596502758674,-36.6936378559558));
#23895=CARTESIAN_POINT('Ctrl Pts',(-5.87641515309022,4.43321181663958,-36.7328960578448));
#23896=CARTESIAN_POINT('Ctrl Pts',(-5.05523627580577,5.35072070526111,-36.7721542597339));
#23897=CARTESIAN_POINT('Ctrl Pts',(-4.06576666907401,6.0190867334552,-36.8114124616229));
#23898=CARTESIAN_POINT('Ctrl Pts',(-3.07629706234226,6.68745276164928,-36.8506706635119));
#23899=CARTESIAN_POINT('Ctrl Pts',(-1.91853672616322,7.10667592941592,-36.889928865401));
#23900=CARTESIAN_POINT('Ctrl Pts',(-0.730537932789972,7.22676805626345,
-36.92918706729));
#23901=CARTESIAN_POINT('Ctrl Pts',(0.45746086058329,7.34686018311099,-36.9684452691791));
#23902=CARTESIAN_POINT('Ctrl Pts',(1.67569811115074,7.16782126903941,-37.0077034710681));
#23903=CARTESIAN_POINT('Ctrl Pts',(2.77891043352645,6.71099990026633,-37.0469616729572));
#23904=CARTESIAN_POINT('Ctrl Pts',(3.88212275590215,6.25417853149326,-37.0862198748462));
#23905=CARTESIAN_POINT('Ctrl Pts',(4.8703101500861,5.51957470801871,-37.1254780767352));
#23906=CARTESIAN_POINT('Ctrl Pts',(5.62564043785605,4.59478316401532,-37.1647362786243));
#23907=CARTESIAN_POINT('Ctrl Pts',(6.380970725626,3.66999162001192,-37.2039944805133));
#23908=CARTESIAN_POINT('Ctrl Pts',(6.90344390698194,2.55501235547971,-37.2432526824024));
#23909=CARTESIAN_POINT('Ctrl Pts',(7.13075993507001,1.38279623365648,-37.2825108842914));
#23910=CARTESIAN_POINT('Ctrl Pts',(7.35807596315808,0.210580111833238,-37.3217690861805));
#23911=CARTESIAN_POINT('Ctrl Pts',(7.29023483797825,-1.01887286728106,-37.3610272880695));
#23912=CARTESIAN_POINT('Ctrl Pts',(6.93532597438994,-2.15896186613015,-37.4002854899585));
#23913=CARTESIAN_POINT('Ctrl Pts',(6.58041711080162,-3.29905086497925,-37.4395436918476));
#23914=CARTESIAN_POINT('Ctrl Pts',(5.93844050880484,-4.34977588356314,-37.4788018937366));
#23915=CARTESIAN_POINT('Ctrl Pts',(5.08594590498163,-5.18584775403549,-37.5180600956257));
#23916=CARTESIAN_POINT('Ctrl Pts',(4.23345130115843,-6.02191962450782,-37.5573182975147));
#23917=CARTESIAN_POINT('Ctrl Pts',(3.17043869550879,-6.64333834686859,-37.5965764994038));
#23918=CARTESIAN_POINT('Ctrl Pts',(2.02366244242788,-6.97600552010563,-37.6358347012928));
#23919=CARTESIAN_POINT('Ctrl Pts',(0.876886189346959,-7.30867269334268,
-37.6750929031818));
#23920=CARTESIAN_POINT('Ctrl Pts',(-0.353653711165226,-7.35258831745601,
-37.7143511050709));
#23921=CARTESIAN_POINT('Ctrl Pts',(-1.52122683174925,-7.10251586508858,
-37.7536093069599));
#23922=CARTESIAN_POINT('Ctrl Pts',(-2.68879995233323,-6.85244341272115,
-37.792867508849));
#23923=CARTESIAN_POINT('Ctrl Pts',(-3.79340629298905,-6.30838288387294,
-37.832125710738));
#23924=CARTESIAN_POINT('Ctrl Pts',(-4.70333183225955,-5.53520843028317,
-37.871383912627));
#23925=CARTESIAN_POINT('Ctrl Pts',(-5.61325737153008,-4.76203397669338,
-37.9106421145161));
#23926=CARTESIAN_POINT('Ctrl Pts',(-6.32850210941532,-3.75974559836202,
-37.9499003164052));
#23927=CARTESIAN_POINT('Ctrl Pts',(-6.76377976984235,-2.64785685327351,
-37.9891585182942));
#23928=CARTESIAN_POINT('Ctrl Pts',(-7.09300555276655,-1.80687079791927,
-38.0188517771682));
#23929=CARTESIAN_POINT('Ctrl Pts',(-7.26206845007066,-0.903184830974666,
-38.0485450360421));
#23930=CARTESIAN_POINT('Ctrl Pts',(-7.26295522622064,0.000178426625192518,
-38.0782382949161));
#23931=CARTESIAN_POINT('Ctrl Pts',(-2.10185380438476,7.82409821225381,-48.));
#23932=CARTESIAN_POINT('Ctrl Pts',(-3.38848271769056,7.47846018434309,-47.960741798111));
#23933=CARTESIAN_POINT('Ctrl Pts',(-5.7867414247356,6.14069431107141,-47.8822253943329));
#23934=CARTESIAN_POINT('Ctrl Pts',(-8.00479568248447,2.66750428527037,-47.7644507886658));
#23935=CARTESIAN_POINT('Ctrl Pts',(-8.31350431498314,-1.4410774330594,-47.6466761829986));
#23936=CARTESIAN_POINT('Ctrl Pts',(-6.63976806498755,-5.20635630979624,
-47.5289015773315));
#23937=CARTESIAN_POINT('Ctrl Pts',(-3.38248655907778,-7.72983620180326,
-47.4111269716644));
#23938=CARTESIAN_POINT('Ctrl Pts',(0.681413555862794,-8.40998264592954,
-47.2933523659973));
#23939=CARTESIAN_POINT('Ctrl Pts',(4.58282963250162,-7.08446123670512,-47.1755777603301));
#23940=CARTESIAN_POINT('Ctrl Pts',(7.39131613068618,-4.06944919929777,-47.057803154663));
#23941=CARTESIAN_POINT('Ctrl Pts',(8.43711630815339,-0.0839387386951516,
-46.9400285489959));
#23942=CARTESIAN_POINT('Ctrl Pts',(7.47081891547249,3.92158434705153,-46.8222539433287));
#23943=CARTESIAN_POINT('Ctrl Pts',(4.72287152121607,6.99188514875576,-46.7044793376616));
#23944=CARTESIAN_POINT('Ctrl Pts',(0.848606621735488,8.39475027502305,-46.5867047319945));
#23945=CARTESIAN_POINT('Ctrl Pts',(-3.22803486495866,7.79562439652349,-46.4689301263274));
#23946=CARTESIAN_POINT('Ctrl Pts',(-6.53485028731455,5.33738695312811,-46.3511555206602));
#23947=CARTESIAN_POINT('Ctrl Pts',(-8.28322552855154,1.60628225714427,-46.2333809149931));
#23948=CARTESIAN_POINT('Ctrl Pts',(-8.05620575449563,-2.50789092127668,
-46.115606309326));
#23949=CARTESIAN_POINT('Ctrl Pts',(-5.90793090228909,-6.02397877694788,
-45.9978317036589));
#23950=CARTESIAN_POINT('Ctrl Pts',(-2.35072454748789,-8.10345988234339,
-45.8800570979917));
#23951=CARTESIAN_POINT('Ctrl Pts',(1.76708584413041,-8.25041668822644,-45.7622824923246));
#23952=CARTESIAN_POINT('Ctrl Pts',(5.46347916408095,-6.42980274600106,-45.6445078866575));
#23953=CARTESIAN_POINT('Ctrl Pts',(7.85693443764436,-3.07580057347912,-45.5267332809903));
#23954=CARTESIAN_POINT('Ctrl Pts',(8.37665714814605,1.01172276152054,-45.4089586753233));
#23955=CARTESIAN_POINT('Ctrl Pts',(6.89870310741494,4.85796905729832,-45.291184069656));
#23956=CARTESIAN_POINT('Ctrl Pts',(3.77553683341622,7.54568019093911,-45.173409463989));
#23957=CARTESIAN_POINT('Ctrl Pts',(-0.248024672543488,8.4338871042367,-45.0556348583218));
#23958=CARTESIAN_POINT('Ctrl Pts',(-4.21243691249803,7.31076898712496,-44.9378602526548));
#23959=CARTESIAN_POINT('Ctrl Pts',(-7.17226138689772,4.44416859749758,-44.8200856469875));
#23960=CARTESIAN_POINT('Ctrl Pts',(-8.4216350723183,0.517716750424533,-44.7023110413205));
#23961=CARTESIAN_POINT('Ctrl Pts',(-7.66260560886039,-3.5322009014224,-44.5845364356533));
#23962=CARTESIAN_POINT('Ctrl Pts',(-5.0761873899821,-6.73975440997329,-44.4667618299862));
#23963=CARTESIAN_POINT('Ctrl Pts',(-1.27919300023199,-8.3400019899946,-44.3489872243191));
#23964=CARTESIAN_POINT('Ctrl Pts',(2.82286510073567,-7.95131439121922,-44.2312126186519));
#23965=CARTESIAN_POINT('Ctrl Pts',(6.25172243861154,-5.66638636835865,-44.1134380129848));
#23966=CARTESIAN_POINT('Ctrl Pts',(8.18966038568263,-2.03013070814185,-43.9956634073177));
#23967=CARTESIAN_POINT('Ctrl Pts',(8.17451682713419,2.09027332372109,-43.8778888016505));
#23968=CARTESIAN_POINT('Ctrl Pts',(6.20990321969786,5.71218609001371,-43.7601141959834));
#23969=CARTESIAN_POINT('Ctrl Pts',(2.76434332646893,7.97184883815334,-43.6423395903163));
#23970=CARTESIAN_POINT('Ctrl Pts',(-1.34046097639977,8.33037407897806,-43.5245649846492));
#23971=CARTESIAN_POINT('Ctrl Pts',(-5.12559029658075,6.70226021850519,-43.406790378982));
#23972=CARTESIAN_POINT('Ctrl Pts',(-7.68836177257858,3.47578209600548,-43.2890157733149));
#23973=CARTESIAN_POINT('Ctrl Pts',(-8.41760212770272,-0.579605335253821,
-43.1712411676478));
#23974=CARTESIAN_POINT('Ctrl Pts',(-7.1394011161468,-4.49676768665247,-43.0534665619807));
#23975=CARTESIAN_POINT('Ctrl Pts',(-4.15858587830098,-7.34153467728348,
-42.9356919563136));
#23976=CARTESIAN_POINT('Ctrl Pts',(-0.186025343832157,-8.43548235114104,
-42.8179173506464));
#23977=CARTESIAN_POINT('Ctrl Pts',(3.83089877123767,-7.51772455796898,-42.7001427449793));
#23978=CARTESIAN_POINT('Ctrl Pts',(6.93422486298953,-4.80712944224074,-42.5823681393122));
#23979=CARTESIAN_POINT('Ctrl Pts',(8.38386744432517,-0.950123466158245,
-42.464593533645));
#23980=CARTESIAN_POINT('Ctrl Pts',(7.83411375280636,3.13346926473683,-42.3468189279779));
#23981=CARTESIAN_POINT('Ctrl Pts',(5.41606980711838,6.46978792306059,-42.2290443223107));
#23982=CARTESIAN_POINT('Ctrl Pts',(1.70639406288594,8.2631826330481,-42.1112697166436));
#23983=CARTESIAN_POINT('Ctrl Pts',(-2.4102248912686,8.08596215044749,-41.9934951109765));
#23984=CARTESIAN_POINT('Ctrl Pts',(-5.95205008868199,5.98039026040782,-41.8757205053094));
#23985=CARTESIAN_POINT('Ctrl Pts',(-8.07442217067084,2.44860665169793,-41.7579458996422));
#23986=CARTESIAN_POINT('Ctrl Pts',(-8.27119491551605,-1.66712404892423,
-41.6401712939752));
#23987=CARTESIAN_POINT('Ctrl Pts',(-6.49544168759803,-5.38527670672303,
-41.522396688308));
#23988=CARTESIAN_POINT('Ctrl Pts',(-3.17064656618999,-7.81914114703574,
-41.4046220826409));
#23989=CARTESIAN_POINT('Ctrl Pts',(0.910288721922364,-8.38828602085676,
-41.2868474769737));
#23990=CARTESIAN_POINT('Ctrl Pts',(4.77413709997572,-6.95698087359707,-41.1690728713066));
#23991=CARTESIAN_POINT('Ctrl Pts',(7.4994426769679,-3.86656533112174,-41.0512982656395));
#23992=CARTESIAN_POINT('Ctrl Pts',(8.43627081960314,0.145954045071271,-40.9335236599723));
#23993=CARTESIAN_POINT('Ctrl Pts',(7.36120546016224,4.12366609926623,-40.8157490543053));
#23994=CARTESIAN_POINT('Ctrl Pts',(4.53062966851309,7.11796057391082,-40.6979744486381));
#23995=CARTESIAN_POINT('Ctrl Pts',(0.619583063952851,8.41475399235312,-40.5801998429711));
#23996=CARTESIAN_POINT('Ctrl Pts',(-3.43922256435361,7.70478527136227,-40.4624252373038));
#23997=CARTESIAN_POINT('Ctrl Pts',(-6.67783765143915,5.15736873085314,-40.3446506316368));
#23998=CARTESIAN_POINT('Ctrl Pts',(-8.32391280398028,1.38001578132032,-40.2268760259696));
#23999=CARTESIAN_POINT('Ctrl Pts',(-7.98488974899803,-2.72644523533966,
-40.1091014203025));
#24000=CARTESIAN_POINT('Ctrl Pts',(-5.74161917229395,-6.18269983140913,
-39.9913268146354));
#24001=CARTESIAN_POINT('Ctrl Pts',(-2.12907933537458,-8.16449564324956,
-39.8735522089682));
#24002=CARTESIAN_POINT('Ctrl Pts',(1.9912062783033,-8.19921127195815,-39.7557776033011));
#24003=CARTESIAN_POINT('Ctrl Pts',(5.63662627205554,-6.27856768651366,-39.638002997634));
#24004=CARTESIAN_POINT('Ctrl Pts',(7.93781585726883,-2.86060261851435,-39.5202283919668));
#24005=CARTESIAN_POINT('Ctrl Pts',(8.3459841673938,1.23956290787192,-39.4024537862997));
#24006=CARTESIAN_POINT('Ctrl Pts',(6.76379066080322,5.0441157621324,-39.2846791806326));
#24007=CARTESIAN_POINT('Ctrl Pts',(3.56855902743119,7.64574093157071,-39.1669045749655));
#24008=CARTESIAN_POINT('Ctrl Pts',(-0.477707485283489,8.42399925709112,
-39.0491299692983));
#24009=CARTESIAN_POINT('Ctrl Pts',(-4.4100496579569,7.19329061968874,-38.9313553636312));
#24010=CARTESIAN_POINT('Ctrl Pts',(-7.29067710496446,4.24711611286043,-38.8135807579641));
#24011=CARTESIAN_POINT('Ctrl Pts',(-8.43261381919959,0.288083496944457,
-38.695806152297));
#24012=CARTESIAN_POINT('Ctrl Pts',(-7.56352915785683,-3.73965166868971,
-38.5780315466298));
#24013=CARTESIAN_POINT('Ctrl Pts',(-4.89068362979871,-6.87554954592136,
-38.4602569409627));
#24014=CARTESIAN_POINT('Ctrl Pts',(-1.05150112347229,-8.3717568832205,-38.3424823352955));
#24015=CARTESIAN_POINT('Ctrl Pts',(3.03844482120267,-7.87145609112005,-38.2247077296284));
#24016=CARTESIAN_POINT('Ctrl Pts',(6.40377825371979,-5.49395959222041,-38.1069331239613));
#24017=CARTESIAN_POINT('Ctrl Pts',(8.24192981481277,-1.80625603195024,-37.9891585182942));
#24018=CARTESIAN_POINT('Ctrl Pts',(8.11453458490175,2.31220595952502,-37.871383912627));
#24019=CARTESIAN_POINT('Ctrl Pts',(6.05197395361438,5.87924988197173,-37.7536093069599));
#24020=CARTESIAN_POINT('Ctrl Pts',(2.54613022648071,8.0442021874585,-37.6358347012928));
#24021=CARTESIAN_POINT('Ctrl Pts',(-1.56691815067151,8.29076204944015,-37.5180600956257));
#24022=CARTESIAN_POINT('Ctrl Pts',(-5.30628572285852,6.56012956115795,-37.4002854899586));
#24023=CARTESIAN_POINT('Ctrl Pts',(-7.78020296240809,3.26502828627881,-37.2825108842914));
#24024=CARTESIAN_POINT('Ctrl Pts',(-8.39868665514552,-0.808721357278217,
-37.1647362786243));
#24025=CARTESIAN_POINT('Ctrl Pts',(-7.01423999417884,-4.68960618017365,
-37.0469616729571));
#24026=CARTESIAN_POINT('Ctrl Pts',(-3.95702765317846,-7.45210691888099,
-36.92918706729));
#24027=CARTESIAN_POINT('Ctrl Pts',(0.0438619977836959,-8.43741959751058,
-36.8114124616229));
#24028=CARTESIAN_POINT('Ctrl Pts',(4.03429158844322,-7.41056343594989,-36.6936378559558));
#24029=CARTESIAN_POINT('Ctrl Pts',(7.06261733076329,-4.61642867900756,-36.5758632502887));
#24030=CARTESIAN_POINT('Ctrl Pts',(8.40664121397815,-0.721355965422936,
-36.4580886446215));
#24031=CARTESIAN_POINT('Ctrl Pts',(7.74583594905282,3.34573518158168,-36.3403140389544));
#24032=CARTESIAN_POINT('Ctrl Pts',(5.23779660784082,6.61495421252791,-36.2225394332873));
#24033=CARTESIAN_POINT('Ctrl Pts',(1.48063306394132,8.30658225499598,-36.1047648276201));
#24034=CARTESIAN_POINT('Ctrl Pts',(-2.62961918038579,8.01734176317378,-35.986990221953));
#24035=CARTESIAN_POINT('Ctrl Pts',(-6.11278614011418,5.81591813633449,-35.8692156162859));
#24036=CARTESIAN_POINT('Ctrl Pts',(-8.1381056994787,2.22790678763051,-35.7514410106188));
#24037=CARTESIAN_POINT('Ctrl Pts',(-8.2227680260995,-1.89224441543144,-35.6336664049516));
#24038=CARTESIAN_POINT('Ctrl Pts',(-6.97149994399699,-4.33674652103884,
-35.5551500011735));
#24039=CARTESIAN_POINT('Ctrl Pts',(-6.09356451288676,-5.33879890774012,
-35.5158917992845));
#24040=CARTESIAN_POINT('Ctrl Pts',(-2.02934030215363,7.55416851400967,-48.1613694002385));
#24041=CARTESIAN_POINT('Ctrl Pts',(-3.27158079587429,7.22045492340081,-48.1221111983495));
#24042=CARTESIAN_POINT('Ctrl Pts',(-5.58710009557265,5.92884168378703,-48.0435947945714));
#24043=CARTESIAN_POINT('Ctrl Pts',(-7.72863196054971,2.5754759636345,-47.9258201889042));
#24044=CARTESIAN_POINT('Ctrl Pts',(-8.02669021191114,-1.3913605729051,-47.8080455832372));
#24045=CARTESIAN_POINT('Ctrl Pts',(-6.41069750099766,-5.02673814173007,
-47.69027097757));
#24046=CARTESIAN_POINT('Ctrl Pts',(-3.26579150343843,-7.46315852255819,
-47.5724963719029));
#24047=CARTESIAN_POINT('Ctrl Pts',(0.657904935377249,-8.11984006128011,
-47.4547217662357));
#24048=CARTESIAN_POINT('Ctrl Pts',(4.42472300011451,-6.84004885434888,-47.3369471605686));
#24049=CARTESIAN_POINT('Ctrl Pts',(7.13631732077113,-3.9290540809612,-47.2191725549015));
#24050=CARTESIAN_POINT('Ctrl Pts',(8.14603761801837,-0.0810428703417254,
-47.1013979492344));
#24051=CARTESIAN_POINT('Ctrl Pts',(7.21307727665566,3.78629053417727,-46.9836233435672));
#24052=CARTESIAN_POINT('Ctrl Pts',(4.55993347391867,6.75066662143647,-46.8658487379002));
#24053=CARTESIAN_POINT('Ctrl Pts',(0.819329876592602,8.10513320387957,-46.748074132233));
#24054=CARTESIAN_POINT('Ctrl Pts',(-3.11666835940339,7.52667703877142,-46.6302995265659));
#24055=CARTESIAN_POINT('Ctrl Pts',(-6.30939936399117,5.15324825617085,-46.5125249208987));
#24056=CARTESIAN_POINT('Ctrl Pts',(-7.99745603707093,1.55086586624483,-46.3947503152316));
#24057=CARTESIAN_POINT('Ctrl Pts',(-7.77826839618155,-2.4213692262206,-46.2769757095645));
#24058=CARTESIAN_POINT('Ctrl Pts',(-5.70410856232861,-5.8161528103791,-46.1592011038973));
#24059=CARTESIAN_POINT('Ctrl Pts',(-2.26962505837811,-7.8238922668259,-46.0414264982302));
#24060=CARTESIAN_POINT('Ctrl Pts',(1.70612176421503,-7.96577909465003,-45.9236518925631));
#24061=CARTESIAN_POINT('Ctrl Pts',(5.27499031308291,-6.20797594016174,-45.8058772868959));
#24062=CARTESIAN_POINT('Ctrl Pts',(7.58587189671717,-2.96968611809587,-45.6881026812289));
#24063=CARTESIAN_POINT('Ctrl Pts',(8.08766428597154,0.97681854478969,-45.5703280755617));
#24064=CARTESIAN_POINT('Ctrl Pts',(6.66069934039371,4.69037017418842,-45.4525534698946));
#24065=CARTESIAN_POINT('Ctrl Pts',(3.64528162821473,7.28535585428942,-45.3347788642275));
#24066=CARTESIAN_POINT('Ctrl Pts',(-0.239467874916397,8.14291982093926,
-45.2170042585603));
#24067=CARTESIAN_POINT('Ctrl Pts',(-4.06710874894274,7.05854903626383,-45.0992296528932));
#24068=CARTESIAN_POINT('Ctrl Pts',(-6.92481991832549,4.29084574086602,-44.9814550472261));
#24069=CARTESIAN_POINT('Ctrl Pts',(-8.1310904814755,0.499855634366561,-44.863680441559));
#24070=CARTESIAN_POINT('Ctrl Pts',(-7.3982473705494,-3.41034073331186,-44.7459058358918));
#24071=CARTESIAN_POINT('Ctrl Pts',(-4.90106002153181,-6.50723433867939,
-44.6281312302247));
#24072=CARTESIAN_POINT('Ctrl Pts',(-1.23506111804168,-8.05227372285845,
-44.5103566245576));
#24073=CARTESIAN_POINT('Ctrl Pts',(2.72547686452563,-7.67699576228066,-44.3925820188904));
#24074=CARTESIAN_POINT('Ctrl Pts',(6.03603936491014,-5.47089726264288,-44.2748074132233));
#24075=CARTESIAN_POINT('Ctrl Pts',(7.90711887142005,-1.96009163723823,-44.1570328075562));
#24076=CARTESIAN_POINT('Ctrl Pts',(7.89249776237038,2.01815934557136,-44.0392582018891));
#24077=CARTESIAN_POINT('Ctrl Pts',(5.99566290001563,5.51511690379401,-43.9214835962219));
#24078=CARTESIAN_POINT('Ctrl Pts',(2.66897407882984,7.69682177523119,-43.8037089905548));
#24079=CARTESIAN_POINT('Ctrl Pts',(-1.29421536226612,8.04297797269226,-43.6859343848877));
#24080=CARTESIAN_POINT('Ctrl Pts',(-4.9487585385243,6.47103368871784,-43.5681597792205));
#24081=CARTESIAN_POINT('Ctrl Pts',(-7.42311495218289,3.35586836449482,-43.4503851735534));
#24082=CARTESIAN_POINT('Ctrl Pts',(-8.127196672578,-0.559609076387755,-43.3326105678863));
#24083=CARTESIAN_POINT('Ctrl Pts',(-6.89309331981735,-4.34163017280696,
-43.2148359622192));
#24084=CARTESIAN_POINT('Ctrl Pts',(-4.01511556379315,-7.08825331675756,
-43.097061356552));
#24085=CARTESIAN_POINT('Ctrl Pts',(-0.179607509653168,-8.14446003217,-42.9792867508849));
#24086=CARTESIAN_POINT('Ctrl Pts',(3.69873359114005,-7.25836468461807,-42.8615121452178));
#24087=CARTESIAN_POINT('Ctrl Pts',(6.69499560307401,-4.64128451486849,-42.7437375395506));
#24088=CARTESIAN_POINT('Ctrl Pts',(8.09462582848997,-0.917344411811364,
-42.6259629338836));
#24089=CARTESIAN_POINT('Ctrl Pts',(7.5638385205766,3.02536525196216,-42.5081883282164));
#24090=CARTESIAN_POINT('Ctrl Pts',(5.22921656869468,6.24658163724989,-42.3904137225493));
#24091=CARTESIAN_POINT('Ctrl Pts',(1.6475238363135,7.9781046171329,-42.2726391168821));
#24092=CARTESIAN_POINT('Ctrl Pts',(-2.32707265315102,7.80699820290073,-42.1548645112151));
#24093=CARTESIAN_POINT('Ctrl Pts',(-5.74670564632112,5.77406808824415,-42.0370899055479));
#24094=CARTESIAN_POINT('Ctrl Pts',(-7.79585634993363,2.36413025113635,-41.9193152998808));
#24095=CARTESIAN_POINT('Ctrl Pts',(-7.98584047758644,-1.60960862935077,
-41.8015406942137));
#24096=CARTESIAN_POINT('Ctrl Pts',(-6.27135035245223,-5.19948582361138,
-41.6837660885465));
#24097=CARTESIAN_POINT('Ctrl Pts',(-3.06125994454584,-7.54938246647084,
-41.5659914828794));
#24098=CARTESIAN_POINT('Ctrl Pts',(0.878883957646947,-8.09889196508568,
-41.4482168772122));
#24099=CARTESIAN_POINT('Ctrl Pts',(4.60943040128496,-6.7169665362311,-41.3304422715451));
#24100=CARTESIAN_POINT('Ctrl Pts',(7.24071352456248,-3.73316966241243,-41.212667665878));
#24101=CARTESIAN_POINT('Ctrl Pts',(8.14522129864046,0.140918662043758,-41.0948930602109));
#24102=CARTESIAN_POINT('Ctrl Pts',(7.10724546187608,3.9814005095921,-40.9771184545438));
#24103=CARTESIAN_POINT('Ctrl Pts',(4.3743239236079,6.87239247165716,-40.8593438488766));
#24104=CARTESIAN_POINT('Ctrl Pts',(0.598207582082232,8.12444679728274,-40.7415692432096));
#24105=CARTESIAN_POINT('Ctrl Pts',(-3.32057012878775,7.43897184380617,-40.6237946375423));
#24106=CARTESIAN_POINT('Ctrl Pts',(-6.44745369494008,4.97944062367873,-40.5060200318753));
#24107=CARTESIAN_POINT('Ctrl Pts',(-8.03673961028621,1.33240553496112,-40.3882454262081));
#24108=CARTESIAN_POINT('Ctrl Pts',(-7.70941277746869,-2.63238346365819,
-40.270470820541));
#24109=CARTESIAN_POINT('Ctrl Pts',(-5.54353455109341,-5.96939802274668,
-40.1526962148739));
#24110=CARTESIAN_POINT('Ctrl Pts',(-2.05562655820527,-7.8828223071651,-40.0349216092067));
#24111=CARTESIAN_POINT('Ctrl Pts',(1.92251009182108,-7.91634025418214,-39.9171470035396));
#24112=CARTESIAN_POINT('Ctrl Pts',(5.44216388323377,-6.06195845755845,-39.7993723978724));
#24113=CARTESIAN_POINT('Ctrl Pts',(7.66396292483574,-2.76191244609261,-39.6815977922053));
#24114=CARTESIAN_POINT('Ctrl Pts',(8.05804951642959,1.19679825530756,-39.5638231865382));
#24115=CARTESIAN_POINT('Ctrl Pts',(6.53044134404774,4.87009485791515,-39.4460485808711));
#24116=CARTESIAN_POINT('Ctrl Pts',(3.44544451182704,7.38196452098329,-39.328273975204));
#24117=CARTESIAN_POINT('Ctrl Pts',(-0.461226680230507,8.13337310238434,
-39.2104993695368));
#24118=CARTESIAN_POINT('Ctrl Pts',(-4.25790389736948,6.94512364712774,-39.0927247638697));
#24119=CARTESIAN_POINT('Ctrl Pts',(-7.03915031969784,4.10059152438366,-38.9749501582026));
#24120=CARTESIAN_POINT('Ctrl Pts',(-8.1416904639609,0.278144678528614,-38.8571755525354));
#24121=CARTESIAN_POINT('Ctrl Pts',(-7.30258903570402,-3.61063449391976,
-38.7394009468683));
#24122=CARTESIAN_POINT('Ctrl Pts',(-4.7219561010042,-6.63834457177027,-38.6216263412012));
#24123=CARTESIAN_POINT('Ctrl Pts',(-1.01522456184661,-8.08293307912742,
-38.5038517355341));
#24124=CARTESIAN_POINT('Ctrl Pts',(2.93361913120376,-7.59989255628477,-38.3860771298669));
#24125=CARTESIAN_POINT('Ctrl Pts',(6.18284928724263,-5.30441917303561,-38.2683025241998));
#24126=CARTESIAN_POINT('Ctrl Pts',(7.95758501653589,-1.74394058901621,-38.1505279185327));
#24127=CARTESIAN_POINT('Ctrl Pts',(7.83458489453823,2.23243535337958,-38.0327533128655));
#24128=CARTESIAN_POINT('Ctrl Pts',(5.84318215949784,5.67641703101683,-37.9149787071985));
#24129=CARTESIAN_POINT('Ctrl Pts',(2.45828928365514,7.76667894961431,-37.7972041015313));
#24130=CARTESIAN_POINT('Ctrl Pts',(-1.51285981294236,8.00473254961685,-37.6794294958642));
#24131=CARTESIAN_POINT('Ctrl Pts',(-5.12322001162739,6.33380650834752,-37.561654890197));
#24132=CARTESIAN_POINT('Ctrl Pts',(-7.51178764080184,3.15238551567893,-37.4438802845299));
#24133=CARTESIAN_POINT('Ctrl Pts',(-8.1089337797381,-0.780820645143519,
-37.3261056788628));
#24134=CARTESIAN_POINT('Ctrl Pts',(-6.77225022952131,-4.52781577995659,
-37.2083310731957));
#24135=CARTESIAN_POINT('Ctrl Pts',(-3.82051105389889,-7.1950108399046,-37.0905564675286));
#24136=CARTESIAN_POINT('Ctrl Pts',(0.0423487683347632,-8.14633044395825,
-36.9727818618614));
#24137=CARTESIAN_POINT('Ctrl Pts',(3.89510940008676,-7.15490059816084,-36.8550072561943));
#24138=CARTESIAN_POINT('Ctrl Pts',(6.81895855844356,-4.4571628867737,-36.7372326505271));
#24139=CARTESIAN_POINT('Ctrl Pts',(8.11661390800927,-0.6964693404355,-36.61945804486));
#24140=CARTESIAN_POINT('Ctrl Pts',(7.47860628198373,3.23030804052729,-36.5016834391929));
#24141=CARTESIAN_POINT('Ctrl Pts',(5.05709375628351,6.38673972108787,-36.3839088335257));
#24142=CARTESIAN_POINT('Ctrl Pts',(1.42955154306598,8.0200069614983,-36.2661342278587));
#24143=CARTESIAN_POINT('Ctrl Pts',(-2.53889788668489,7.74074520416533,-36.1483596221915));
#24144=CARTESIAN_POINT('Ctrl Pts',(-5.90189633869939,5.61527021692382,-36.0305850165244));
#24145=CARTESIAN_POINT('Ctrl Pts',(-7.85734281075386,2.15104448470603,-35.9128104108573));
#24146=CARTESIAN_POINT('Ctrl Pts',(-7.9390843053941,-1.8269623918416,-35.7950358051901));
#24147=CARTESIAN_POINT('Ctrl Pts',(-6.73098470183848,-4.18712970284093,
-35.716519401412));
#24148=CARTESIAN_POINT('Ctrl Pts',(-5.88333785345927,-5.15461149865373,
-35.677261199523));
#24149=CARTESIAN_POINT('Ctrl Pts',(-1.95682679992249,7.28423881576552,-48.322738800477));
#24150=CARTESIAN_POINT('Ctrl Pts',(-3.15467887405802,6.96244966245853,-48.283480598588));
#24151=CARTESIAN_POINT('Ctrl Pts',(-5.38745876640971,5.71698905650265,-48.2049641948099));
#24152=CARTESIAN_POINT('Ctrl Pts',(-7.45246823861496,2.48344764199862,-48.0871895891427));
#24153=CARTESIAN_POINT('Ctrl Pts',(-7.73987610883915,-1.34164371275079,
-47.9694149834756));
#24154=CARTESIAN_POINT('Ctrl Pts',(-6.18162693700778,-4.84711997366391,
-47.8516403778085));
#24155=CARTESIAN_POINT('Ctrl Pts',(-3.14909644779907,-7.19648084331311,
-47.7338657721414));
#24156=CARTESIAN_POINT('Ctrl Pts',(0.634396314891706,-7.82969747663068,
-47.6160911664742));
#24157=CARTESIAN_POINT('Ctrl Pts',(4.26661636772739,-6.59563647199265,-47.4983165608071));
#24158=CARTESIAN_POINT('Ctrl Pts',(6.88131851085609,-3.78865896262463,-47.38054195514));
#24159=CARTESIAN_POINT('Ctrl Pts',(7.85495892788334,-0.0781470019882984,
-47.2627673494728));
#24160=CARTESIAN_POINT('Ctrl Pts',(6.95533563783883,3.65099672130299,-47.1449927438058));
#24161=CARTESIAN_POINT('Ctrl Pts',(4.39699542662127,6.50944809411718,-47.0272181381386));
#24162=CARTESIAN_POINT('Ctrl Pts',(0.790053131449719,7.81551613273609,-46.9094435324715));
#24163=CARTESIAN_POINT('Ctrl Pts',(-3.00530185384814,7.25772968101937,-46.7916689268043));
#24164=CARTESIAN_POINT('Ctrl Pts',(-6.08394844066777,4.96910955921358,-46.6738943211372));
#24165=CARTESIAN_POINT('Ctrl Pts',(-7.71168654559033,1.49544947534539,-46.5561197154701));
#24166=CARTESIAN_POINT('Ctrl Pts',(-7.50033103786747,-2.33484753116452,
-46.438345109803));
#24167=CARTESIAN_POINT('Ctrl Pts',(-5.50028622236814,-5.60832684381034,
-46.3205705041358));
#24168=CARTESIAN_POINT('Ctrl Pts',(-2.18852556926833,-7.5443246513084,-46.2027958984687));
#24169=CARTESIAN_POINT('Ctrl Pts',(1.64515768429965,-7.68114150107363,-46.0850212928016));
#24170=CARTESIAN_POINT('Ctrl Pts',(5.08650146208487,-5.98614913432241,-45.9672466871344));
#24171=CARTESIAN_POINT('Ctrl Pts',(7.31480935578999,-2.86357166271262,-45.8494720814674));
#24172=CARTESIAN_POINT('Ctrl Pts',(7.79867142379702,0.941914328058838,-45.7316974758002));
#24173=CARTESIAN_POINT('Ctrl Pts',(6.42269557337249,4.52277129107851,-45.6139228701331));
#24174=CARTESIAN_POINT('Ctrl Pts',(3.51502642301324,7.02503151763973,-45.4961482644659));
#24175=CARTESIAN_POINT('Ctrl Pts',(-0.230911077289297,7.85195253764182,
-45.3783736587988));
#24176=CARTESIAN_POINT('Ctrl Pts',(-3.92178058538745,6.80632908540271,-45.2605990531317));
#24177=CARTESIAN_POINT('Ctrl Pts',(-6.67737844975326,4.13752288423446,-45.1428244474646));
#24178=CARTESIAN_POINT('Ctrl Pts',(-7.8405458906327,0.481994518308594,-45.0250498417974));
#24179=CARTESIAN_POINT('Ctrl Pts',(-7.13388913223841,-3.28848056520132,
-44.9072752361303));
#24180=CARTESIAN_POINT('Ctrl Pts',(-4.72593265308153,-6.27471426738548,
-44.7895006304632));
#24181=CARTESIAN_POINT('Ctrl Pts',(-1.19092923585136,-7.7645454557223,-44.6717260247961));
#24182=CARTESIAN_POINT('Ctrl Pts',(2.62808862831559,-7.4026771333421,-44.5539514191289));
#24183=CARTESIAN_POINT('Ctrl Pts',(5.82035629120873,-5.27540815692712,-44.4361768134618));
#24184=CARTESIAN_POINT('Ctrl Pts',(7.62457735715747,-1.89005256633461,-44.3184022077947));
#24185=CARTESIAN_POINT('Ctrl Pts',(7.61047869760657,1.94604536742163,-44.2006276021275));
#24186=CARTESIAN_POINT('Ctrl Pts',(5.78142258033341,5.31804771757433,-44.0828529964604));
#24187=CARTESIAN_POINT('Ctrl Pts',(2.57360483119075,7.42179471230903,-43.9650783907933));
#24188=CARTESIAN_POINT('Ctrl Pts',(-1.24796974813247,7.75558186640647,-43.8473037851262));
#24189=CARTESIAN_POINT('Ctrl Pts',(-4.77192678046785,6.23980715893049,-43.729529179459));
#24190=CARTESIAN_POINT('Ctrl Pts',(-7.15786813178719,3.23595463298417,-43.6117545737919));
#24191=CARTESIAN_POINT('Ctrl Pts',(-7.83679121745328,-0.539612817521684,
-43.4939799681248));
#24192=CARTESIAN_POINT('Ctrl Pts',(-6.6467855234879,-4.18649265896147,-43.3762053624577));
#24193=CARTESIAN_POINT('Ctrl Pts',(-3.87164524928533,-6.83497195623163,
-43.2584307567905));
#24194=CARTESIAN_POINT('Ctrl Pts',(-0.173189675474176,-7.85343771319897,
-43.1406561511234));
#24195=CARTESIAN_POINT('Ctrl Pts',(3.56656841104242,-6.99900481126716,-43.0228815454563));
#24196=CARTESIAN_POINT('Ctrl Pts',(6.45576634315849,-4.47543958749625,-42.9051069397891));
#24197=CARTESIAN_POINT('Ctrl Pts',(7.80538421265478,-0.884565357464481,
-42.787332334122));
#24198=CARTESIAN_POINT('Ctrl Pts',(7.29356328834684,2.9172612391875,-42.6695577284549));
#24199=CARTESIAN_POINT('Ctrl Pts',(5.04236333027098,6.02337535143919,-42.5517831227878));
#24200=CARTESIAN_POINT('Ctrl Pts',(1.58865360974106,7.6930266012177,-42.4340085171206));
#24201=CARTESIAN_POINT('Ctrl Pts',(-2.24392041503344,7.52803425535397,-42.3162339114536));
#24202=CARTESIAN_POINT('Ctrl Pts',(-5.54136120396024,5.56774591608048,-42.1984593057864));
#24203=CARTESIAN_POINT('Ctrl Pts',(-7.51729052919641,2.27965385057478,-42.0806847001193));
#24204=CARTESIAN_POINT('Ctrl Pts',(-7.70048603965684,-1.55209320977732,
-41.9629100944521));
#24205=CARTESIAN_POINT('Ctrl Pts',(-6.04725901730644,-5.01369494049972,
-41.845135488785));
#24206=CARTESIAN_POINT('Ctrl Pts',(-2.95187332290169,-7.27962378590596,
-41.7273608831179));
#24207=CARTESIAN_POINT('Ctrl Pts',(0.84747919337153,-7.80949790931459,-41.6095862774508));
#24208=CARTESIAN_POINT('Ctrl Pts',(4.4447237025942,-6.47695219886514,-41.4918116717836));
#24209=CARTESIAN_POINT('Ctrl Pts',(6.98198437215706,-3.59977399370311,-41.3740370661165));
#24210=CARTESIAN_POINT('Ctrl Pts',(7.85417177767779,0.135883279016239,-41.2562624604493));
#24211=CARTESIAN_POINT('Ctrl Pts',(6.85328546358993,3.83913491991798,-41.1384878547823));
#24212=CARTESIAN_POINT('Ctrl Pts',(4.2180181787027,6.62682436940348,-41.0207132491151));
#24213=CARTESIAN_POINT('Ctrl Pts',(0.576832100211618,7.83413960221236,-40.902938643448));
#24214=CARTESIAN_POINT('Ctrl Pts',(-3.20191769322189,7.17315841625007,-40.7851640377808));
#24215=CARTESIAN_POINT('Ctrl Pts',(-6.21706973844099,4.80151251650432,-40.6673894321137));
#24216=CARTESIAN_POINT('Ctrl Pts',(-7.74956641659215,1.28479528860193,-40.5496148264466));
#24217=CARTESIAN_POINT('Ctrl Pts',(-7.43393580593934,-2.53832169197672,
-40.4318402207795));
#24218=CARTESIAN_POINT('Ctrl Pts',(-5.34544992989288,-5.75609621408423,
-40.3140656151123));
#24219=CARTESIAN_POINT('Ctrl Pts',(-1.98217378103596,-7.60114897108064,
-40.1962910094452));
#24220=CARTESIAN_POINT('Ctrl Pts',(1.85381390533885,-7.63346923640613,-40.0785164037781));
#24221=CARTESIAN_POINT('Ctrl Pts',(5.247701494412,-5.84534922860326,-39.960741798111));
#24222=CARTESIAN_POINT('Ctrl Pts',(7.39010999240267,-2.66322227367086,-39.8429671924438));
#24223=CARTESIAN_POINT('Ctrl Pts',(7.77011486546537,1.1540336027432,-39.7251925867767));
#24224=CARTESIAN_POINT('Ctrl Pts',(6.29709202729227,4.6960739536979,-39.6074179811096));
#24225=CARTESIAN_POINT('Ctrl Pts',(3.32232999622289,7.11818811039587,-39.4896433754424));
#24226=CARTESIAN_POINT('Ctrl Pts',(-0.44474587517752,7.84274694767756,-39.3718687697753));
#24227=CARTESIAN_POINT('Ctrl Pts',(-4.10575813678208,6.69695667456673,-39.2540941641082));
#24228=CARTESIAN_POINT('Ctrl Pts',(-6.7876235344312,3.9540669359069,-39.1363195584411));
#24229=CARTESIAN_POINT('Ctrl Pts',(-7.85076710872221,0.268205860112767,
-39.018544952774));
#24230=CARTESIAN_POINT('Ctrl Pts',(-7.0416489135512,-3.4816173191498,-38.9007703471068));
#24231=CARTESIAN_POINT('Ctrl Pts',(-4.55322857220969,-6.40113959761918,
-38.7829957414397));
#24232=CARTESIAN_POINT('Ctrl Pts',(-0.978948000220917,-7.79410927503433,
-38.6652211357725));
#24233=CARTESIAN_POINT('Ctrl Pts',(2.82879344120486,-7.32832902144949,-38.5474465301054));
#24234=CARTESIAN_POINT('Ctrl Pts',(5.96192032076547,-5.11487875385082,-38.4296719244383));
#24235=CARTESIAN_POINT('Ctrl Pts',(7.673240218259,-1.68162514608217,-38.3118973187712));
#24236=CARTESIAN_POINT('Ctrl Pts',(7.55463520417472,2.15266474723415,-38.194122713104));
#24237=CARTESIAN_POINT('Ctrl Pts',(5.63439036538128,5.47358418006194,-38.0763481074369));
#24238=CARTESIAN_POINT('Ctrl Pts',(2.37044834082958,7.48915571177013,-37.9585735017698));
#24239=CARTESIAN_POINT('Ctrl Pts',(-1.45880147521322,7.71870304979355,-37.8407988961027));
#24240=CARTESIAN_POINT('Ctrl Pts',(-4.94015430039627,6.1074834555371,-37.7230242904356));
#24241=CARTESIAN_POINT('Ctrl Pts',(-7.24337231919559,3.03974274507905,-37.6052496847684));
#24242=CARTESIAN_POINT('Ctrl Pts',(-7.81918090433069,-0.752919933008821,
-37.4874750791013));
#24243=CARTESIAN_POINT('Ctrl Pts',(-6.53026046486378,-4.36602537973952,
-37.3697004734342));
#24244=CARTESIAN_POINT('Ctrl Pts',(-3.68399445461933,-6.93791476092821,
-37.251925867767));
#24245=CARTESIAN_POINT('Ctrl Pts',(0.0408355388858274,-7.85524129040592,
-37.1341512620999));
#24246=CARTESIAN_POINT('Ctrl Pts',(3.7559272117303,-6.89923776037179,-37.0163766564328));
#24247=CARTESIAN_POINT('Ctrl Pts',(6.57529978612382,-4.29789709453984,-36.8986020507657));
#24248=CARTESIAN_POINT('Ctrl Pts',(7.82658660204039,-0.671582715448067,
-36.7808274450985));
#24249=CARTESIAN_POINT('Ctrl Pts',(7.21137661491463,3.11488089947291,-36.6630528394314));
#24250=CARTESIAN_POINT('Ctrl Pts',(4.87639090472621,6.15852522964781,-36.5452782337643));
#24251=CARTESIAN_POINT('Ctrl Pts',(1.37847002219063,7.73343166800063,-36.4275036280971));
#24252=CARTESIAN_POINT('Ctrl Pts',(-2.44817659298399,7.46414864515686,-36.30972902243));
#24253=CARTESIAN_POINT('Ctrl Pts',(-5.69100653728461,5.41462229751315,-36.1919544167629));
#24254=CARTESIAN_POINT('Ctrl Pts',(-7.57657992202902,2.07418218178154,-36.0741798110957));
#24255=CARTESIAN_POINT('Ctrl Pts',(-7.6554005846887,-1.76168036825176,-35.9564052054286));
#24256=CARTESIAN_POINT('Ctrl Pts',(-6.49046945967997,-4.03751288464302,
-35.8778888016505));
#24257=CARTESIAN_POINT('Ctrl Pts',(-5.67311119403177,-4.97042408956735,
-35.8386305997615));
#24258=CARTESIAN_POINT('Ctrl Pts',(-1.88431329769136,7.01430911752138,-48.4841082007155));
#24259=CARTESIAN_POINT('Ctrl Pts',(-3.03777695224175,6.70444440151624,-48.4448499988265));
#24260=CARTESIAN_POINT('Ctrl Pts',(-5.18781743724676,5.50513642921826,-48.3663335950484));
#24261=CARTESIAN_POINT('Ctrl Pts',(-7.17630451668021,2.39141932036274,-48.2485589893813));
#24262=CARTESIAN_POINT('Ctrl Pts',(-7.45306200576714,-1.29192685259649,
-48.1307843837141));
#24263=CARTESIAN_POINT('Ctrl Pts',(-5.9525563730179,-4.66750180559774,-48.013009778047));
#24264=CARTESIAN_POINT('Ctrl Pts',(-3.03240139215972,-6.92980316406803,
-47.8952351723799));
#24265=CARTESIAN_POINT('Ctrl Pts',(0.61088769440616,-7.53955489198126,-47.7774605667127));
#24266=CARTESIAN_POINT('Ctrl Pts',(4.10850973534028,-6.35122408963641,-47.6596859610457));
#24267=CARTESIAN_POINT('Ctrl Pts',(6.62631970094104,-3.64826384428806,-47.5419113553785));
#24268=CARTESIAN_POINT('Ctrl Pts',(7.56388023774832,-0.075251133634871,
-47.4241367497114));
#24269=CARTESIAN_POINT('Ctrl Pts',(6.697593999022,3.51570290842873,-47.3063621440442));
#24270=CARTESIAN_POINT('Ctrl Pts',(4.23405737932386,6.26822956679788,-47.1885875383771));
#24271=CARTESIAN_POINT('Ctrl Pts',(0.76077638630684,7.5258990615926,-47.07081293271));
#24272=CARTESIAN_POINT('Ctrl Pts',(-2.89393534829288,6.98878232326731,-46.9530383270428));
#24273=CARTESIAN_POINT('Ctrl Pts',(-5.85849751734439,4.7849708622563,-46.8352637213758));
#24274=CARTESIAN_POINT('Ctrl Pts',(-7.42591705410972,1.44003308444595,-46.7174891157086));
#24275=CARTESIAN_POINT('Ctrl Pts',(-7.22239367955339,-2.24832583610844,
-46.5997145100415));
#24276=CARTESIAN_POINT('Ctrl Pts',(-5.29646388240766,-5.40050087724156,
-46.4819399043744));
#24277=CARTESIAN_POINT('Ctrl Pts',(-2.10742608015855,-7.26475703579091,
-46.3641652987072));
#24278=CARTESIAN_POINT('Ctrl Pts',(1.58419360438427,-7.39650390749722,-46.2463906930401));
#24279=CARTESIAN_POINT('Ctrl Pts',(4.89801261108683,-5.76432232848308,-46.1286160873729));
#24280=CARTESIAN_POINT('Ctrl Pts',(7.0437468148628,-2.75745720732937,-46.0108414817059));
#24281=CARTESIAN_POINT('Ctrl Pts',(7.50967856162251,0.907010111327988,-45.8930668760387));
#24282=CARTESIAN_POINT('Ctrl Pts',(6.18469180635125,4.35517240796861,-45.7752922703716));
#24283=CARTESIAN_POINT('Ctrl Pts',(3.38477121781176,6.76470718099003,-45.6575176647045));
#24284=CARTESIAN_POINT('Ctrl Pts',(-0.222354279662207,7.5609852543444,-45.5397430590373));
#24285=CARTESIAN_POINT('Ctrl Pts',(-3.77645242183215,6.55410913454158,-45.4219684533702));
#24286=CARTESIAN_POINT('Ctrl Pts',(-6.42993698118103,3.9842000276029,-45.304193847703));
#24287=CARTESIAN_POINT('Ctrl Pts',(-7.55000129978989,0.464133402250619,
-45.186419242036));
#24288=CARTESIAN_POINT('Ctrl Pts',(-6.86953089392742,-3.16662039709077,
-45.0686446363688));
#24289=CARTESIAN_POINT('Ctrl Pts',(-4.55080528463124,-6.04219419609158,
-44.9508700307017));
#24290=CARTESIAN_POINT('Ctrl Pts',(-1.14679735366105,-7.47681718858616,
-44.8330954250346));
#24291=CARTESIAN_POINT('Ctrl Pts',(2.53070039210556,-7.12835850440353,-44.7153208193674));
#24292=CARTESIAN_POINT('Ctrl Pts',(5.60467321750733,-5.07991905121136,-44.5975462137003));
#24293=CARTESIAN_POINT('Ctrl Pts',(7.34203584289489,-1.820013495431,-44.4797716080332));
#24294=CARTESIAN_POINT('Ctrl Pts',(7.32845963284276,1.8739313892719,-44.361997002366));
#24295=CARTESIAN_POINT('Ctrl Pts',(5.56718226065119,5.12097853135463,-44.244222396699));
#24296=CARTESIAN_POINT('Ctrl Pts',(2.47823558355166,7.14676764938687,-44.1264477910318));
#24297=CARTESIAN_POINT('Ctrl Pts',(-1.20172413399882,7.46818576012066,-44.0086731853647));
#24298=CARTESIAN_POINT('Ctrl Pts',(-4.59509502241141,6.00858062914315,-43.8908985796975));
#24299=CARTESIAN_POINT('Ctrl Pts',(-6.8926213113915,3.11604090147352,-43.7731239740304));
#24300=CARTESIAN_POINT('Ctrl Pts',(-7.54638576232856,-0.519616558655614,
-43.6553493683633));
#24301=CARTESIAN_POINT('Ctrl Pts',(-6.40047772715846,-4.03135514511596,
-43.5375747626962));
#24302=CARTESIAN_POINT('Ctrl Pts',(-3.72817493477751,-6.58169059570571,
-43.419800157029));
#24303=CARTESIAN_POINT('Ctrl Pts',(-0.166771841295187,-7.56241539422793,
-43.3020255513619));
#24304=CARTESIAN_POINT('Ctrl Pts',(3.43440323094479,-6.73964493791626,-43.1842509456948));
#24305=CARTESIAN_POINT('Ctrl Pts',(6.21653708324298,-4.309594660124,-43.0664763400276));
#24306=CARTESIAN_POINT('Ctrl Pts',(7.51614259681957,-0.851786303117605,
-42.9487017343606));
#24307=CARTESIAN_POINT('Ctrl Pts',(7.02328805611709,2.80915722641283,-42.8309271286934));
#24308=CARTESIAN_POINT('Ctrl Pts',(4.85551009184728,5.80016906562848,-42.7131525230263));
#24309=CARTESIAN_POINT('Ctrl Pts',(1.52978338316862,7.40794858530251,-42.5953779173591));
#24310=CARTESIAN_POINT('Ctrl Pts',(-2.16076817691586,7.24907030780721,-42.477603311692));
#24311=CARTESIAN_POINT('Ctrl Pts',(-5.33601676159937,5.3614237439168,-42.3598287060249));
#24312=CARTESIAN_POINT('Ctrl Pts',(-7.2387247084592,2.19517745001321,-42.2420541003578));
#24313=CARTESIAN_POINT('Ctrl Pts',(-7.41513160172723,-1.49457779020387,
-42.1242794946906));
#24314=CARTESIAN_POINT('Ctrl Pts',(-5.82316768216064,-4.82790405738806,
-42.0065048890235));
#24315=CARTESIAN_POINT('Ctrl Pts',(-2.84248670125753,-7.00986510534107,
-41.8887302833564));
#24316=CARTESIAN_POINT('Ctrl Pts',(0.81607442909611,-7.5201038535435,-41.7709556776893));
#24317=CARTESIAN_POINT('Ctrl Pts',(4.28001700390344,-6.23693786149917,-41.6531810720221));
#24318=CARTESIAN_POINT('Ctrl Pts',(6.72325521975163,-3.46637832499379,-41.535406466355));
#24319=CARTESIAN_POINT('Ctrl Pts',(7.56312225671513,0.130847895988726,-41.4176318606878));
#24320=CARTESIAN_POINT('Ctrl Pts',(6.59932546530375,3.69686933024385,-41.2998572550208));
#24321=CARTESIAN_POINT('Ctrl Pts',(4.06171243379752,6.38125626714983,-41.1820826493536));
#24322=CARTESIAN_POINT('Ctrl Pts',(0.555456618340993,7.54383240714197,-41.0643080436865));
#24323=CARTESIAN_POINT('Ctrl Pts',(-3.08326525765602,6.90734498869397,-40.9465334380193));
#24324=CARTESIAN_POINT('Ctrl Pts',(-5.98668578194193,4.62358440932992,-40.8287588323522));
#24325=CARTESIAN_POINT('Ctrl Pts',(-7.46239322289808,1.23718504224273,-40.7109842266851));
#24326=CARTESIAN_POINT('Ctrl Pts',(-7.15845883441,-2.44425992029525,-40.593209621018));
#24327=CARTESIAN_POINT('Ctrl Pts',(-5.14736530869233,-5.54279440542178,
-40.4754350153509));
#24328=CARTESIAN_POINT('Ctrl Pts',(-1.90872100386664,-7.31947563499618,
-40.3576604096837));
#24329=CARTESIAN_POINT('Ctrl Pts',(1.78511771885662,-7.35059821863013,-40.2398858040166));
#24330=CARTESIAN_POINT('Ctrl Pts',(5.05323910559024,-5.62873999964806,-40.1221111983495));
#24331=CARTESIAN_POINT('Ctrl Pts',(7.11625705996958,-2.56453210124912,-40.0043365926823));
#24332=CARTESIAN_POINT('Ctrl Pts',(7.48218021450115,1.11126895017883,-39.8865619870152));
#24333=CARTESIAN_POINT('Ctrl Pts',(6.0637427105368,4.52205304948066,-39.7687873813481));
#24334=CARTESIAN_POINT('Ctrl Pts',(3.19921548061873,6.85441169980844,-39.651012775681));
#24335=CARTESIAN_POINT('Ctrl Pts',(-0.428265070124539,7.55212079297079,
-39.5332381700138));
#24336=CARTESIAN_POINT('Ctrl Pts',(-3.95361237619466,6.44878970200573,-39.4154635643467));
#24337=CARTESIAN_POINT('Ctrl Pts',(-6.53609674916458,3.80754234743014,-39.2976889586796));
#24338=CARTESIAN_POINT('Ctrl Pts',(-7.55984375348351,0.258267041696921,
-39.1799143530124));
#24339=CARTESIAN_POINT('Ctrl Pts',(-6.7807087913984,-3.35260014437985,-39.0621397473453));
#24340=CARTESIAN_POINT('Ctrl Pts',(-4.38450104341517,-6.1639346234681,-38.9443651416782));
#24341=CARTESIAN_POINT('Ctrl Pts',(-0.942671438595233,-7.50528547094125,
-38.8265905360111));
#24342=CARTESIAN_POINT('Ctrl Pts',(2.72396775120595,-7.0567654866142,-38.7088159303439));
#24343=CARTESIAN_POINT('Ctrl Pts',(5.74099135428831,-4.92533833466603,-38.5910413246768));
#24344=CARTESIAN_POINT('Ctrl Pts',(7.38889541998213,-1.61930970314814,-38.4732667190097));
#24345=CARTESIAN_POINT('Ctrl Pts',(7.2746855138112,2.07289414108871,-38.3554921133426));
#24346=CARTESIAN_POINT('Ctrl Pts',(5.42559857126474,5.27075132910704,-38.2377175076754));
#24347=CARTESIAN_POINT('Ctrl Pts',(2.282607398004,7.21163247392595,-38.1199429020083));
#24348=CARTESIAN_POINT('Ctrl Pts',(-1.40474313748407,7.43267354997024,-38.0021682963412));
#24349=CARTESIAN_POINT('Ctrl Pts',(-4.75708858916514,5.88116040272668,-37.8843936906741));
#24350=CARTESIAN_POINT('Ctrl Pts',(-6.97495699758933,2.92709997447918,-37.7666190850069));
#24351=CARTESIAN_POINT('Ctrl Pts',(-7.52942802892327,-0.725019220874125,
-37.6488444793398));
#24352=CARTESIAN_POINT('Ctrl Pts',(-6.28827070020625,-4.20423497952246,
-37.5310698736727));
#24353=CARTESIAN_POINT('Ctrl Pts',(-3.54747785533976,-6.68081868195182,
-37.4132952680055));
#24354=CARTESIAN_POINT('Ctrl Pts',(0.0393223094368914,-7.56415213685359,
-37.2955206623384));
#24355=CARTESIAN_POINT('Ctrl Pts',(3.61674502337384,-6.64357492258274,-37.1777460566713));
#24356=CARTESIAN_POINT('Ctrl Pts',(6.33164101380409,-4.13863130230598,-37.0599714510042));
#24357=CARTESIAN_POINT('Ctrl Pts',(7.5365592960715,-0.646696090460631,-36.942196845337));
#24358=CARTESIAN_POINT('Ctrl Pts',(6.94414694784554,2.99945375841853,-36.8244222396699));
#24359=CARTESIAN_POINT('Ctrl Pts',(4.6956880531689,5.93031073820777,-36.7066476340028));
#24360=CARTESIAN_POINT('Ctrl Pts',(1.32738850131529,7.44685637450296,-36.5888730283356));
#24361=CARTESIAN_POINT('Ctrl Pts',(-2.3574552992831,7.1875520861484,-36.4710984226685));
#24362=CARTESIAN_POINT('Ctrl Pts',(-5.48011673586982,5.21397437810249,-36.3533238170014));
#24363=CARTESIAN_POINT('Ctrl Pts',(-7.29581703330418,1.99731987885706,-36.2355492113343));
#24364=CARTESIAN_POINT('Ctrl Pts',(-7.3717168639833,-1.69639834466192,-36.1177746056671));
#24365=CARTESIAN_POINT('Ctrl Pts',(-6.24995421752146,-3.88789606644511,
-36.039258201889));
#24366=CARTESIAN_POINT('Ctrl Pts',(-5.46288453460428,-4.78623668048096,
-36.));
#24367=CARTESIAN_POINT('Ctrl Pts',(-5.46288453460428,-4.78623668048096,
-36.));
#24368=CARTESIAN_POINT('Ctrl Pts',(-5.5977429381527,-4.64891391735923,-36.));
#24369=CARTESIAN_POINT('Ctrl Pts',(-5.72676732341115,-4.50639566671148,
-36.));
#24370=CARTESIAN_POINT('Ctrl Pts',(-5.84982542989412,-4.35916059628739,
-36.));
#24371=CARTESIAN_POINT('Ctrl Pts',(-5.97481042968556,-4.20962005993278,
-36.));
#24372=CARTESIAN_POINT('Ctrl Pts',(-6.09364127024401,-4.05521340122182,
-36.));
#24373=CARTESIAN_POINT('Ctrl Pts',(-6.20615068412284,-3.89639624867873,
-36.));
#24374=CARTESIAN_POINT('Ctrl Pts',(-6.32533404445892,-3.7281582207082,-36.));
#24375=CARTESIAN_POINT('Ctrl Pts',(-6.43742462013448,-3.55497067838873,
-36.));
#24376=CARTESIAN_POINT('Ctrl Pts',(-6.54218137983461,-3.37732902325465,
-36.));
#24377=CARTESIAN_POINT('Ctrl Pts',(-6.6419677919629,-3.20811585303918,-36.));
#24378=CARTESIAN_POINT('Ctrl Pts',(-6.73509988284937,-3.03486032491094,
-36.));
#24379=CARTESIAN_POINT('Ctrl Pts',(-6.82132654460192,-2.85795957462792,
-36.));
#24380=CARTESIAN_POINT('Ctrl Pts',(-6.86766107917013,-2.76290064781184,
-36.));
#24381=CARTESIAN_POINT('Ctrl Pts',(-6.91200089902377,-2.66678868814126,
-36.));
#24382=CARTESIAN_POINT('Ctrl Pts',(-6.95430142435144,-2.56968261694418,
-36.));
#24383=CARTESIAN_POINT('Ctrl Pts',(-6.97457148673207,-2.52315018961722,
-36.));
#24384=CARTESIAN_POINT('Ctrl Pts',(-6.99437321597084,-2.47638946583898,
-36.));
#24385=CARTESIAN_POINT('Ctrl Pts',(-7.01370136184102,-2.42940681080466,
-36.));
#24386=CARTESIAN_POINT('Ctrl Pts',(-7.02151953803784,-2.41040246979236,
-36.));
#24387=CARTESIAN_POINT('Ctrl Pts',(-7.02925969742251,-2.39136302740604,
-36.));
#24388=CARTESIAN_POINT('Ctrl Pts',(-7.03691795983629,-2.37229797553799,
-36.));
#24389=CARTESIAN_POINT('Ctrl Pts',(-7.11159816098769,-2.18638349108455,
-36.));
#24390=CARTESIAN_POINT('Ctrl Pts',(-7.17859038835048,-1.99780273753807,
-36.));
#24391=CARTESIAN_POINT('Ctrl Pts',(-7.23771363498118,-1.80701554492453,
-36.));
#24392=CARTESIAN_POINT('Ctrl Pts',(-7.25137682897175,-1.76292523236309,
-36.));
#24393=CARTESIAN_POINT('Ctrl Pts',(-7.26461960889502,-1.71871693832445,
-36.));
#24394=CARTESIAN_POINT('Ctrl Pts',(-7.27743943403625,-1.67439609022036,
-36.));
#24395=CARTESIAN_POINT('Ctrl Pts',(-7.33236404335992,-1.48451009410166,
-36.));
#24396=CARTESIAN_POINT('Ctrl Pts',(-7.37952880573868,-1.29256003410601,
-36.));
#24397=CARTESIAN_POINT('Ctrl Pts',(-7.41900478204454,-1.09903177851102,
-36.));
#24398=CARTESIAN_POINT('Ctrl Pts',(-7.45887446791156,-0.903573388902557,
-36.));
#24399=CARTESIAN_POINT('Ctrl Pts',(-7.49090138133267,-0.706504520118917,
-36.));
#24400=CARTESIAN_POINT('Ctrl Pts',(-7.51510912682397,-0.508306182126472,
-36.));
#24401=CARTESIAN_POINT('Ctrl Pts',(-7.53937145031977,-0.309660992535023,
-36.));
#24402=CARTESIAN_POINT('Ctrl Pts',(-7.55577940447303,-0.109880537467743,
-36.));
#24403=CARTESIAN_POINT('Ctrl Pts',(-7.56430545051381,0.0905602703403912,
-36.));
#24404=CARTESIAN_POINT('Ctrl Pts',(-7.56775676889125,0.171698120202889,
-36.));
#24405=CARTESIAN_POINT('Ctrl Pts',(-7.56991595964691,0.252944223882185,
-36.));
#24406=CARTESIAN_POINT('Ctrl Pts',(-7.57077875624231,0.334267110558196,
-36.));
#24407=CARTESIAN_POINT('Ctrl Pts',(-7.57111625441944,0.366077998731034,
-36.));
#24408=CARTESIAN_POINT('Ctrl Pts',(-7.57125537315957,0.39790063464037,-36.));
#24409=CARTESIAN_POINT('Ctrl Pts',(-7.57119579778133,0.429733129242087,
-36.));
#24410=CARTESIAN_POINT('Ctrl Pts',(-7.57115243537445,0.45290266040532,-36.));
#24411=CARTESIAN_POINT('Ctrl Pts',(-7.57100382199647,0.476067956682383,
-36.));
#24412=CARTESIAN_POINT('Ctrl Pts',(-7.57075011198204,0.499226838302265,
-36.));
#24413=CARTESIAN_POINT('Ctrl Pts',(-7.56852835775061,0.702030591829401,
-36.));
#24414=CARTESIAN_POINT('Ctrl Pts',(-7.55825116056467,0.904376836416967,
-36.));
#24415=CARTESIAN_POINT('Ctrl Pts',(-7.53999292732573,1.10576724548481,-36.));
#24416=CARTESIAN_POINT('Ctrl Pts',(-7.52160278416925,1.30861263608914,-36.));
#24417=CARTESIAN_POINT('Ctrl Pts',(-7.49511597555556,1.51048903114456,-36.));
#24418=CARTESIAN_POINT('Ctrl Pts',(-7.46055732979923,1.71089945545224,-36.));
#24419=CARTESIAN_POINT('Ctrl Pts',(-7.44239807242019,1.81620753095109,-36.));
#24420=CARTESIAN_POINT('Ctrl Pts',(-7.42200923698019,1.92111097525443,-36.));
#24421=CARTESIAN_POINT('Ctrl Pts',(-7.39938866576489,2.02553801505189,-36.));
#24422=CARTESIAN_POINT('Ctrl Pts',(-7.35650604167764,2.22350408096407,-36.));
#24423=CARTESIAN_POINT('Ctrl Pts',(-7.30560612447398,2.41975870171209,-36.));
#24424=CARTESIAN_POINT('Ctrl Pts',(-7.24693498701336,2.61389377398034,-36.));
#24425=CARTESIAN_POINT('Ctrl Pts',(-7.20801045153952,2.74268993908444,-36.));
#24426=CARTESIAN_POINT('Ctrl Pts',(-7.16566433956697,2.87055307976224,-36.));
#24427=CARTESIAN_POINT('Ctrl Pts',(-7.11995630029871,2.99736080966695,-36.));
#24428=CARTESIAN_POINT('Ctrl Pts',(-7.0956591489905,3.06476835218834,-36.));
#24429=CARTESIAN_POINT('Ctrl Pts',(-7.07041185875794,3.13187761376778,-36.));
#24430=CARTESIAN_POINT('Ctrl Pts',(-7.04422232586475,3.19866977263125,-36.));
#24431=CARTESIAN_POINT('Ctrl Pts',(-7.02727219339145,3.24189833823913,-36.));
#24432=CARTESIAN_POINT('Ctrl Pts',(-7.00992735853431,3.28499406894694,-36.));
#24433=CARTESIAN_POINT('Ctrl Pts',(-6.99218980245843,3.32795178036667,-36.));
#24434=CARTESIAN_POINT('Ctrl Pts',(-6.98238542220851,3.35169652488635,-36.));
#24435=CARTESIAN_POINT('Ctrl Pts',(-6.97246413601817,3.37539157447853,-36.));
#24436=CARTESIAN_POINT('Ctrl Pts',(-6.96242907172261,3.39903020671605,-36.));
#24437=CARTESIAN_POINT('Ctrl Pts',(-6.8820400364091,3.58839489693994,-36.));
#24438=CARTESIAN_POINT('Ctrl Pts',(-6.79430423304295,3.77425987667949,-36.));
#24439=CARTESIAN_POINT('Ctrl Pts',(-6.69953894329377,3.95622441588123,-36.));
#24440=CARTESIAN_POINT('Ctrl Pts',(-6.60408872841896,4.13950412105991,-36.));
#24441=CARTESIAN_POINT('Ctrl Pts',(-6.50150681992606,4.31882744677142,-36.));
#24442=CARTESIAN_POINT('Ctrl Pts',(-6.39206475516827,4.49377628022932,-36.));
#24443=CARTESIAN_POINT('Ctrl Pts',(-6.28276629228395,4.66849555862261,-36.));
#24444=CARTESIAN_POINT('Ctrl Pts',(-6.16662537039312,4.83885245890798,-36.));
#24445=CARTESIAN_POINT('Ctrl Pts',(-6.04386414064415,5.00441227621188,-36.));
#24446=CARTESIAN_POINT('Ctrl Pts',(-5.93619135704333,5.1496233205946,-36.));
#24447=CARTESIAN_POINT('Ctrl Pts',(-5.8234248145294,5.29114403181261,-36.));
#24448=CARTESIAN_POINT('Ctrl Pts',(-5.70568638354113,5.42866360742757,-36.));
#24449=CARTESIAN_POINT('Ctrl Pts',(-5.59912529758274,5.55312794073882,-36.));
#24450=CARTESIAN_POINT('Ctrl Pts',(-5.4884910261217,5.67431465864635,-36.));
#24451=CARTESIAN_POINT('Ctrl Pts',(-5.37397124395929,5.79208610573226,-36.));
#24452=CARTESIAN_POINT('Ctrl Pts',(-5.35469223029994,5.8119125260605,-36.));
#24453=CARTESIAN_POINT('Ctrl Pts',(-5.33530306689327,5.83164212072248,-36.));
#24454=CARTESIAN_POINT('Ctrl Pts',(-5.31580461121635,5.85127418954356,-36.));
#24455=CARTESIAN_POINT('Ctrl Pts',(-5.29758405791643,5.86961959916314,-36.));
#24456=CARTESIAN_POINT('Ctrl Pts',(-5.27927479958802,5.88787306572556,-36.));
#24457=CARTESIAN_POINT('Ctrl Pts',(-5.2608784327401,5.90603352499053,-36.));
#24458=CARTESIAN_POINT('Ctrl Pts',(-5.11313200936276,6.05188530787087,-36.));
#24459=CARTESIAN_POINT('Ctrl Pts',(-4.95975635606592,6.19175466572801,-36.));
#24460=CARTESIAN_POINT('Ctrl Pts',(-4.8012057401011,6.32542432410788,-36.));
#24461=CARTESIAN_POINT('Ctrl Pts',(-4.64119267814809,6.46032693042967,-36.));
#24462=CARTESIAN_POINT('Ctrl Pts',(-4.47590827252764,6.58891541157199,-36.));
#24463=CARTESIAN_POINT('Ctrl Pts',(-4.30577794008802,6.71093368313889,-36.));
#24464=CARTESIAN_POINT('Ctrl Pts',(-4.1678201015731,6.80987769131963,-36.));
#24465=CARTESIAN_POINT('Ctrl Pts',(-4.0266749161711,6.90450093600378,-36.));
#24466=CARTESIAN_POINT('Ctrl Pts',(-3.88255277813534,6.99464804083222,-36.));
#24467=CARTESIAN_POINT('Ctrl Pts',(-3.84870261918472,7.0158210116816,-36.));
#24468=CARTESIAN_POINT('Ctrl Pts',(-3.81468500239647,7.03674881166959,-36.));
#24469=CARTESIAN_POINT('Ctrl Pts',(-3.78052548560284,7.05741567578707,-36.));
#24470=CARTESIAN_POINT('Ctrl Pts',(-3.5993859527263,7.16700698338312,-36.));
#24471=CARTESIAN_POINT('Ctrl Pts',(-3.41413883495251,7.26934114557307,-36.));
#24472=CARTESIAN_POINT('Ctrl Pts',(-3.22522572651255,7.36416890252957,-36.));
#24473=CARTESIAN_POINT('Ctrl Pts',(-3.03641081725833,7.45894736693779,-36.));
#24474=CARTESIAN_POINT('Ctrl Pts',(-2.84393316488135,7.54622765878111,-36.));
#24475=CARTESIAN_POINT('Ctrl Pts',(-2.64820158305729,7.62572028826821,-36.));
#24476=CARTESIAN_POINT('Ctrl Pts',(-2.60498558090497,7.64327163902619,-36.));
#24477=CARTESIAN_POINT('Ctrl Pts',(-2.56161084699581,7.66044317611024,-36.));
#24478=CARTESIAN_POINT('Ctrl Pts',(-2.51808161300395,7.67723148371408,-36.));
#24479=CARTESIAN_POINT('Ctrl Pts',(-2.38090156124179,7.73013893681846,-36.));
#24480=CARTESIAN_POINT('Ctrl Pts',(-2.2421874023443,7.77924117058327,-36.));
#24481=CARTESIAN_POINT('Ctrl Pts',(-2.10210198597179,7.8245263256498,-36.));
#24482=CARTESIAN_POINT('Ctrl Pts',(-7.26313420453275,-0.000171068891272981,
-37.6717617050839));
#24483=CARTESIAN_POINT('Ctrl Pts',(-7.26336489575239,-0.232559497234902,
-37.6641226298359));
#24484=CARTESIAN_POINT('Ctrl Pts',(-7.25242649701633,-0.464926300116374,
-37.6564835545879));
#24485=CARTESIAN_POINT('Ctrl Pts',(-7.23015663558145,-0.696201981423296,
-37.6488444793398));
#24486=CARTESIAN_POINT('Ctrl Pts',(-7.11570891935093,-1.88475780709024,
-37.6095862774508));
#24487=CARTESIAN_POINT('Ctrl Pts',(-6.70198980977859,-3.04449639330636,
-37.5703280755617));
#24488=CARTESIAN_POINT('Ctrl Pts',(-6.03833144751466,-4.03712963681931,
-37.5310698736727));
#24489=CARTESIAN_POINT('Ctrl Pts',(-5.37467308525075,-5.02976288033225,
-37.4918116717836));
#24490=CARTESIAN_POINT('Ctrl Pts',(-4.46107547029526,-5.85529078114203,
-37.4525534698946));
#24491=CARTESIAN_POINT('Ctrl Pts',(-3.40647663535475,-6.41527697403055,
-37.4132952680055));
#24492=CARTESIAN_POINT('Ctrl Pts',(-2.35187780041423,-6.97526316691907,
-37.3740370661165));
#24493=CARTESIAN_POINT('Ctrl Pts',(-1.15627774548866,-7.26970765188633,
-37.3347788642275));
#24494=CARTESIAN_POINT('Ctrl Pts',(0.0377594009636062,-7.26350035865815,
-37.2955206623384));
#24495=CARTESIAN_POINT('Ctrl Pts',(1.23179654741588,-7.25729306542997,-37.2562624604494));
#24496=CARTESIAN_POINT('Ctrl Pts',(2.42427078539487,-6.95043399400635,-37.2170042585603));
#24497=CARTESIAN_POINT('Ctrl Pts',(3.47299056945607,-6.37951385491508,-37.1777460566713));
#24498=CARTESIAN_POINT('Ctrl Pts',(4.52171035351726,-5.80859371582382,-37.1384878547822));
#24499=CARTESIAN_POINT('Ctrl Pts',(5.42667568366067,-4.9736125090649,-37.0992296528932));
#24500=CARTESIAN_POINT('Ctrl Pts',(6.07997806244361,-3.97413270371123,-37.0599714510042));
#24501=CARTESIAN_POINT('Ctrl Pts',(6.73328044122656,-2.97465289835754,-37.0207132491151));
#24502=CARTESIAN_POINT('Ctrl Pts',(7.13491986864902,-1.81067449440914,-36.9814550472261));
#24503=CARTESIAN_POINT('Ctrl Pts',(7.23700419098927,-0.620993650955046,
-36.942196845337));
#24504=CARTESIAN_POINT('Ctrl Pts',(7.33908851332952,0.568687192499043,-36.902938643448));
#24505=CARTESIAN_POINT('Ctrl Pts',(7.14161773058753,1.78407047545882,-36.8636804415589));
#24506=CARTESIAN_POINT('Ctrl Pts',(6.66813919010376,2.88023828023689,-36.8244222396699));
#24507=CARTESIAN_POINT('Ctrl Pts',(6.19466064962,3.97640608501494,-36.7851640377808));
#24508=CARTESIAN_POINT('Ctrl Pts',(5.44517435139446,4.95335841161134,-36.7459058358918));
#24509=CARTESIAN_POINT('Ctrl Pts',(4.50904794363943,5.69459218095874,-36.7066476340028));
#24510=CARTESIAN_POINT('Ctrl Pts',(3.57292153588436,6.43582595030617,-36.6673894321137));
#24511=CARTESIAN_POINT('Ctrl Pts',(2.45015501859983,6.94134116240457,-36.6281312302247));
#24512=CARTESIAN_POINT('Ctrl Pts',(1.27463112652446,7.15088138706134,-36.5888730283356));
#24513=CARTESIAN_POINT('Ctrl Pts',(0.0991072344491403,7.36042161171811,
-36.5496148264466));
#24514=CARTESIAN_POINT('Ctrl Pts',(-1.12917403241698,7.27398684893325,-36.5103566245576));
#24515=CARTESIAN_POINT('Ctrl Pts',(-2.26375823861449,6.90183984953318,-36.4710984226685));
#24516=CARTESIAN_POINT('Ctrl Pts',(-3.39834244481199,6.5296928501331,-36.4318402207795));
#24517=CARTESIAN_POINT('Ctrl Pts',(-4.43922959034089,5.8718336141178,-36.3925820188904));
#24518=CARTESIAN_POINT('Ctrl Pts',(-5.2622898793444,5.00679491290259,-36.3533238170014));
#24519=CARTESIAN_POINT('Ctrl Pts',(-6.08535016834793,4.14175621168736,-36.3140656151123));
#24520=CARTESIAN_POINT('Ctrl Pts',(-6.69058360082606,3.06953804527219,-36.2748074132233));
#24521=CARTESIAN_POINT('Ctrl Pts',(-7.00585028884498,1.91780925814477,-36.2355492113343));
#24522=CARTESIAN_POINT('Ctrl Pts',(-7.17660081455138,1.29402532109461,-36.2142867092508));
#24523=CARTESIAN_POINT('Ctrl Pts',(-7.26229315301422,0.64691791887602,-36.1930242071674));
#24524=CARTESIAN_POINT('Ctrl Pts',(-7.26243100057087,-0.00011786593126363,
-36.1717617050839));
#24525=CARTESIAN_POINT('Ctrl Pts',(-2.10185380438476,7.82409821225381,-48.));
#24526=CARTESIAN_POINT('Ctrl Pts',(-2.30082761392273,7.75960640525413,-48.));
#24527=CARTESIAN_POINT('Ctrl Pts',(-2.49685179586882,7.68738676969109,-48.));
#24528=CARTESIAN_POINT('Ctrl Pts',(-2.6895559228274,7.60776024312852,-48.));
#24529=CARTESIAN_POINT('Ctrl Pts',(-2.88412187838993,7.52736439757352,-48.));
#24530=CARTESIAN_POINT('Ctrl Pts',(-3.07530391165674,7.43941750700123,-48.));
#24531=CARTESIAN_POINT('Ctrl Pts',(-3.26270174750119,7.34420014302048,-48.));
#24532=CARTESIAN_POINT('Ctrl Pts',(-3.45039148143023,7.2488344648074,-48.));
#24533=CARTESIAN_POINT('Ctrl Pts',(-3.63428579989924,7.14617524942011,-48.));
#24534=CARTESIAN_POINT('Ctrl Pts',(-3.81395475017913,7.03646034322168,-48.));
#24535=CARTESIAN_POINT('Ctrl Pts',(-3.991435635466,6.92808157966276,-48.));
#24536=CARTESIAN_POINT('Ctrl Pts',(-4.16479392090228,6.81281747740625,-48.));
#24537=CARTESIAN_POINT('Ctrl Pts',(-4.33358029554524,6.69086083083259,-48.));
#24538=CARTESIAN_POINT('Ctrl Pts',(-4.43066212905975,6.62071432236176,-48.));
#24539=CARTESIAN_POINT('Ctrl Pts',(-4.52623076734692,6.54835310014871,-48.));
#24540=CARTESIAN_POINT('Ctrl Pts',(-4.62019444968023,6.47380914459575,-48.));
#24541=CARTESIAN_POINT('Ctrl Pts',(-4.66632206375462,6.43721484850242,-48.));
#24542=CARTESIAN_POINT('Ctrl Pts',(-4.71206282220744,6.40009448292469,-48.));
#24543=CARTESIAN_POINT('Ctrl Pts',(-4.75740541705904,6.3624515606279,-48.));
#24544=CARTESIAN_POINT('Ctrl Pts',(-4.77704340810378,6.34614831699173,-48.));
#24545=CARTESIAN_POINT('Ctrl Pts',(-4.79660803540916,6.32974592678438,-48.));
#24546=CARTESIAN_POINT('Ctrl Pts',(-4.81609419498694,6.31324819669125,-48.));
#24547=CARTESIAN_POINT('Ctrl Pts',(-4.9746783621459,6.17898475825485,-48.));
#24548=CARTESIAN_POINT('Ctrl Pts',(-5.12764661424143,6.03876851300631,-48.));
#24549=CARTESIAN_POINT('Ctrl Pts',(-5.27461327719733,5.89285624935101,-48.));
#24550=CARTESIAN_POINT('Ctrl Pts',(-5.32270100774501,5.84511351996507,-48.));
#24551=CARTESIAN_POINT('Ctrl Pts',(-5.37014594422701,5.79676064522343,-48.));
#24552=CARTESIAN_POINT('Ctrl Pts',(-5.41693377234936,5.74780571127434,-48.));
#24553=CARTESIAN_POINT('Ctrl Pts',(-5.55998425669422,5.59812945371915,-48.));
#24554=CARTESIAN_POINT('Ctrl Pts',(-5.69689529217084,5.44282762220933,-48.));
#24555=CARTESIAN_POINT('Ctrl Pts',(-5.82744389958942,5.28234360952657,-48.));
#24556=CARTESIAN_POINT('Ctrl Pts',(-5.95822188709384,5.12157761883323,-48.));
#24557=CARTESIAN_POINT('Ctrl Pts',(-6.08261540116493,4.955610584521,-48.));
#24558=CARTESIAN_POINT('Ctrl Pts',(-6.20035569612236,4.78486113417545,-48.));
#24559=CARTESIAN_POINT('Ctrl Pts',(-6.31730043838319,4.61526541107098,-48.));
#24560=CARTESIAN_POINT('Ctrl Pts',(-6.42768183251017,4.44095104165386,-48.));
#24561=CARTESIAN_POINT('Ctrl Pts',(-6.53118823114018,4.2623110814615,-48.));
#24562=CARTESIAN_POINT('Ctrl Pts',(-6.57281072552227,4.19047551537149,-48.));
#24563=CARTESIAN_POINT('Ctrl Pts',(-6.61332093248692,4.11794034060233,-48.));
#24564=CARTESIAN_POINT('Ctrl Pts',(-6.65269621199041,4.04473068147045,-48.));
#24565=CARTESIAN_POINT('Ctrl Pts',(-6.66624687762794,4.01953620349232,-48.));
#24566=CARTESIAN_POINT('Ctrl Pts',(-6.67966311773293,3.99426184273103,-48.));
#24567=CARTESIAN_POINT('Ctrl Pts',(-6.69294397046647,3.96890861967423,-48.));
#24568=CARTESIAN_POINT('Ctrl Pts',(-6.70467566316242,3.94651275189961,-48.));
#24569=CARTESIAN_POINT('Ctrl Pts',(-6.7163021292488,3.92405442981521,-48.));
#24570=CARTESIAN_POINT('Ctrl Pts',(-6.72781505779003,3.90154957756383,-48.));
#24571=CARTESIAN_POINT('Ctrl Pts',(-6.82109913847309,3.71920288396099,-48.));
#24572=CARTESIAN_POINT('Ctrl Pts',(-6.90705463463742,3.5335738251812,-48.));
#24573=CARTESIAN_POINT('Ctrl Pts',(-6.98547177545329,3.3450880887619,-48.));
#24574=CARTESIAN_POINT('Ctrl Pts',(-7.06354639296283,3.15742565139383,-48.));
#24575=CARTESIAN_POINT('Ctrl Pts',(-7.13414861969922,2.96693079553113,-48.));
#24576=CARTESIAN_POINT('Ctrl Pts',(-7.1970241755622,2.77400364453458,-48.));
#24577=CARTESIAN_POINT('Ctrl Pts',(-7.2338482323043,2.66101282866221,-48.));
#24578=CARTESIAN_POINT('Ctrl Pts',(-7.26802110074051,2.54718739813178,-48.));
#24579=CARTESIAN_POINT('Ctrl Pts',(-7.29948358655117,2.43260584479025,-48.));
#24580=CARTESIAN_POINT('Ctrl Pts',(-7.35348963043526,2.23592410656683,-48.));
#24581=CARTESIAN_POINT('Ctrl Pts',(-7.39951248160726,2.03701428957662,-48.));
#24582=CARTESIAN_POINT('Ctrl Pts',(-7.43751275781667,1.83636816437194,-48.));
#24583=CARTESIAN_POINT('Ctrl Pts',(-7.46184105249056,1.70791178073268,-48.));
#24584=CARTESIAN_POINT('Ctrl Pts',(-7.48288005647684,1.57874367129889,-48.));
#24585=CARTESIAN_POINT('Ctrl Pts',(-7.50060825221396,1.44899399010199,-48.));
#24586=CARTESIAN_POINT('Ctrl Pts',(-7.50964567380242,1.38285062236542,-48.));
#24587=CARTESIAN_POINT('Ctrl Pts',(-7.5178225682247,1.31655614449737,-48.));
#24588=CARTESIAN_POINT('Ctrl Pts',(-7.52513521308343,1.25012800445878,-48.));
#24589=CARTESIAN_POINT('Ctrl Pts',(-7.52928146266447,1.2124634312263,-48.));
#24590=CARTESIAN_POINT('Ctrl Pts',(-7.53314985750579,1.17475589044629,-48.));
#24591=CARTESIAN_POINT('Ctrl Pts',(-7.53673963502003,1.13700858902824,-48.));
#24592=CARTESIAN_POINT('Ctrl Pts',(-7.53984577077182,1.10434688729227,-48.));
#24593=CARTESIAN_POINT('Ctrl Pts',(-7.54274366719671,1.07165020930486,-48.));
#24594=CARTESIAN_POINT('Ctrl Pts',(-7.54543044083257,1.03895170566994,-48.));
#24595=CARTESIAN_POINT('Ctrl Pts',(-7.56194124628142,0.838012324406245,
-48.));
#24596=CARTESIAN_POINT('Ctrl Pts',(-7.57050457306246,0.636810151048556,
-48.));
#24597=CARTESIAN_POINT('Ctrl Pts',(-7.5711534980168,0.435821641100334,-48.));
#24598=CARTESIAN_POINT('Ctrl Pts',(-7.57180231283319,0.234867243670862,
-48.));
#24599=CARTESIAN_POINT('Ctrl Pts',(-7.56453936589094,0.0341257262245018,
-48.));
#24600=CARTESIAN_POINT('Ctrl Pts',(-7.54934565132248,-0.165927071930631,
-48.));
#24601=CARTESIAN_POINT('Ctrl Pts',(-7.5343452687912,-0.363434303309763,
-48.));
#24602=CARTESIAN_POINT('Ctrl Pts',(-7.51161452717462,-0.56027087895125,
-48.));
#24603=CARTESIAN_POINT('Ctrl Pts',(-7.48108590954362,-0.755969183945798,
-48.));
#24604=CARTESIAN_POINT('Ctrl Pts',(-7.45371069442,-0.931453159778154,-48.));
#24605=CARTESIAN_POINT('Ctrl Pts',(-7.42006468953489,-1.10602206717178,
-48.));
#24606=CARTESIAN_POINT('Ctrl Pts',(-7.38006602431795,-1.27932562273681,
-48.));
#24607=CARTESIAN_POINT('Ctrl Pts',(-7.3459202615715,-1.42727011186773,-48.));
#24608=CARTESIAN_POINT('Ctrl Pts',(-7.30714419709347,-1.57429234976623,
-48.));
#24609=CARTESIAN_POINT('Ctrl Pts',(-7.26380600031078,-1.7201873188581,-48.));
#24610=CARTESIAN_POINT('Ctrl Pts',(-7.25535124039227,-1.74864966913019,
-48.));
#24611=CARTESIAN_POINT('Ctrl Pts',(-7.24672280776097,-1.77706908373106,
-48.));
#24612=CARTESIAN_POINT('Ctrl Pts',(-7.23792114978756,-1.80544399113884,
-48.));
#24613=CARTESIAN_POINT('Ctrl Pts',(-7.23013838133962,-1.83053418832141,
-48.));
#24614=CARTESIAN_POINT('Ctrl Pts',(-7.22222270787628,-1.85558137172037,
-48.));
#24615=CARTESIAN_POINT('Ctrl Pts',(-7.21417568267861,-1.88058154446126,
-48.));
#24616=CARTESIAN_POINT('Ctrl Pts',(-7.15325529115503,-2.06984655533421,
-48.));
#24617=CARTESIAN_POINT('Ctrl Pts',(-7.08479318222008,-2.25647534397251,
-48.));
#24618=CARTESIAN_POINT('Ctrl Pts',(-7.00902678423338,-2.44004180818918,
-48.));
#24619=CARTESIAN_POINT('Ctrl Pts',(-6.9317716169254,-2.62721525554879,-48.));
#24620=CARTESIAN_POINT('Ctrl Pts',(-6.84692204906886,-2.8112056027263,-48.));
#24621=CARTESIAN_POINT('Ctrl Pts',(-6.75468148462008,-2.99153370400441,
-48.));
#24622=CARTESIAN_POINT('Ctrl Pts',(-6.71535297813714,-3.06841999522078,
-48.));
#24623=CARTESIAN_POINT('Ctrl Pts',(-6.67468029006978,-3.14464012249059,
-48.));
#24624=CARTESIAN_POINT('Ctrl Pts',(-6.63267676414671,-3.22015495035686,
-48.));
#24625=CARTESIAN_POINT('Ctrl Pts',(-6.6040927348478,-3.27154392318225,-48.));
#24626=CARTESIAN_POINT('Ctrl Pts',(-6.57489236439856,-3.32260624538659,
-48.));
#24627=CARTESIAN_POINT('Ctrl Pts',(-6.54507950331467,-3.37332921731332,
-48.));
#24628=CARTESIAN_POINT('Ctrl Pts',(-6.52647856726046,-3.40497645689337,
-48.));
#24629=CARTESIAN_POINT('Ctrl Pts',(-6.50763776285718,-3.43649378986221,
-48.));
#24630=CARTESIAN_POINT('Ctrl Pts',(-6.48857066029989,-3.46785765893643,
-48.));
#24631=CARTESIAN_POINT('Ctrl Pts',(-6.38641005460389,-3.63590373997915,
-48.));
#24632=CARTESIAN_POINT('Ctrl Pts',(-6.27768399621447,-3.79967229895934,
-48.));
#24633=CARTESIAN_POINT('Ctrl Pts',(-6.16259227067162,-3.95873109139948,
-48.));
#24634=CARTESIAN_POINT('Ctrl Pts',(-6.0487757902373,-4.11602747263176,-48.));
#24635=CARTESIAN_POINT('Ctrl Pts',(-5.92873350940336,-4.26871839150529,
-48.));
#24636=CARTESIAN_POINT('Ctrl Pts',(-5.80262143945877,-4.4163511297274,-48.));
#24637=CARTESIAN_POINT('Ctrl Pts',(-5.77983952334256,-4.44302071543526,
-48.));
#24638=CARTESIAN_POINT('Ctrl Pts',(-5.75685943770476,-4.46952512978906,
-48.));
#24639=CARTESIAN_POINT('Ctrl Pts',(-5.73368198691278,-4.49586156146085,
-48.));
#24640=CARTESIAN_POINT('Ctrl Pts',(-5.64631443946142,-4.59513690733195,
-48.));
#24641=CARTESIAN_POINT('Ctrl Pts',(-5.55614289752022,-4.69202607158615,
-48.));
#24642=CARTESIAN_POINT('Ctrl Pts',(-5.46328272950438,-4.78643225728898,
-48.));
#24643=CARTESIAN_POINT('Origin',(0.,0.,-48.));
#24644=CARTESIAN_POINT('',(-12.,-1.46957615897682E-15,-48.));
#24645=CARTESIAN_POINT('Origin',(0.,0.,-48.));
#24646=CARTESIAN_POINT('Origin',(0.,0.,-48.));
#24647=CARTESIAN_POINT('Origin',(0.,0.,-48.));
#24648=CARTESIAN_POINT('',(-12.,-1.46957615897682E-15,-40.));
#24649=CARTESIAN_POINT('Origin',(0.,0.,-40.));
#24650=CARTESIAN_POINT('',(-12.,-1.46957615897682E-15,-48.));
#24651=CARTESIAN_POINT('Origin',(0.,0.,-40.));
#24652=CARTESIAN_POINT('',(-29.,75.,-40.));
#24653=CARTESIAN_POINT('',(-29.,-75.,-40.));
#24654=CARTESIAN_POINT('',(-29.,35.,-40.));
#24655=CARTESIAN_POINT('',(24.,75.,-40.));
#24656=CARTESIAN_POINT('',(12.,75.,-40.));
#24657=CARTESIAN_POINT('',(24.,-75.,-40.));
#24658=CARTESIAN_POINT('',(24.,-70.,-40.));
#24659=CARTESIAN_POINT('',(-12.,-75.,-40.));
#24660=CARTESIAN_POINT('Ctrl Pts',(20.7937992825328,-52.9692229537457,-40.));
#24661=CARTESIAN_POINT('Ctrl Pts',(20.8868641368446,-52.9351794143205,-40.));
#24662=CARTESIAN_POINT('Ctrl Pts',(20.9778637119143,-52.8963692338032,-40.));
#24663=CARTESIAN_POINT('Ctrl Pts',(21.0665893040918,-52.8531201756825,-40.));
#24664=CARTESIAN_POINT('Ctrl Pts',(21.1572747443127,-52.8089157947528,-40.));
#24665=CARTESIAN_POINT('Ctrl Pts',(21.2455853007886,-52.7600736546262,-40.));
#24666=CARTESIAN_POINT('Ctrl Pts',(21.3312692081619,-52.7068981949415,-40.));
#24667=CARTESIAN_POINT('Ctrl Pts',(21.4136986594278,-52.6557424517338,-40.));
#24668=CARTESIAN_POINT('Ctrl Pts',(21.493697487121,-52.6005754396168,-40.));
#24669=CARTESIAN_POINT('Ctrl Pts',(21.5710085728572,-52.5416381747672,-40.));
#24670=CARTESIAN_POINT('Ctrl Pts',(21.6386557728764,-52.4900680680238,-40.));
#24671=CARTESIAN_POINT('Ctrl Pts',(21.7042448803152,-52.4356106648705,-40.));
#24672=CARTESIAN_POINT('Ctrl Pts',(21.7675790260379,-52.3784147256319,-40.));
#24673=CARTESIAN_POINT('Ctrl Pts',(21.7817032133443,-52.3656594235787,-40.));
#24674=CARTESIAN_POINT('Ctrl Pts',(21.7957178825123,-52.352765201296,-40.));
#24675=CARTESIAN_POINT('Ctrl Pts',(21.8096013024796,-52.3397522015173,-40.));
#24676=CARTESIAN_POINT('Ctrl Pts',(21.8820339673279,-52.2718606982811,-40.));
#24677=CARTESIAN_POINT('Ctrl Pts',(21.9510009955896,-52.2006479598651,-40.));
#24678=CARTESIAN_POINT('Ctrl Pts',(22.0162623182284,-52.1264040004137,-40.));
#24679=CARTESIAN_POINT('Ctrl Pts',(22.0811616750937,-52.0525718280842,-40.));
#24680=CARTESIAN_POINT('Ctrl Pts',(22.1423968052921,-51.975741170508,-40.));
#24681=CARTESIAN_POINT('Ctrl Pts',(22.1996880080389,-51.8961704744865,-40.));
#24682=CARTESIAN_POINT('Ctrl Pts',(22.2548537759022,-51.8195517558178,-40.));
#24683=CARTESIAN_POINT('Ctrl Pts',(22.3063629816812,-51.7403917956857,-40.));
#24684=CARTESIAN_POINT('Ctrl Pts',(22.3539210639109,-51.6589077247976,-40.));
#24685=CARTESIAN_POINT('Ctrl Pts',(22.3738667733396,-51.6247335629137,-40.));
#24686=CARTESIAN_POINT('Ctrl Pts',(22.3931169356095,-51.5901504976334,-40.));
#24687=CARTESIAN_POINT('Ctrl Pts',(22.4116472377174,-51.5551742475532,-40.));
#24688=CARTESIAN_POINT('Ctrl Pts',(22.4245263808776,-51.5308646529568,-40.));
#24689=CARTESIAN_POINT('Ctrl Pts',(22.4370577496651,-51.5063651203315,-40.));
#24690=CARTESIAN_POINT('Ctrl Pts',(22.4492327155052,-51.4816809210378,-40.));
#24691=CARTESIAN_POINT('Ctrl Pts',(22.4571463279311,-51.4656364254049,-40.));
#24692=CARTESIAN_POINT('Ctrl Pts',(22.4649104788499,-51.4495112843647,-40.));
#24693=CARTESIAN_POINT('Ctrl Pts',(22.4725126070347,-51.4333291644309,-40.));
#24694=CARTESIAN_POINT('Ctrl Pts',(22.5146350497842,-51.3436660590602,-40.));
#24695=CARTESIAN_POINT('Ctrl Pts',(22.5518581247129,-51.2521171179474,-40.));
#24696=CARTESIAN_POINT('Ctrl Pts',(22.583890412798,-51.1589539662439,-40.));
#24697=CARTESIAN_POINT('Ctrl Pts',(22.6137693466924,-51.0720536597857,-40.));
#24698=CARTESIAN_POINT('Ctrl Pts',(22.6391317579652,-50.9837480859561,-40.));
#24699=CARTESIAN_POINT('Ctrl Pts',(22.6596906010889,-50.894248963726,-40.));
#24700=CARTESIAN_POINT('Ctrl Pts',(22.6611722627557,-50.8877988236176,-40.));
#24701=CARTESIAN_POINT('Ctrl Pts',(22.6626289522036,-50.8813424830588,-40.));
#24702=CARTESIAN_POINT('Ctrl Pts',(22.6640605513299,-50.8748800209782,-40.));
#24703=CARTESIAN_POINT('Ctrl Pts',(22.6846661151432,-50.781863287207,-40.));
#24704=CARTESIAN_POINT('Ctrl Pts',(22.7000779522779,-50.6875773770759,-40.));
#24705=CARTESIAN_POINT('Ctrl Pts',(22.7103730991959,-50.5924307647528,-40.));
#24706=CARTESIAN_POINT('Ctrl Pts',(22.7161681739401,-50.5388733231281,-40.));
#24707=CARTESIAN_POINT('Ctrl Pts',(22.7203410991825,-50.4850433569999,-40.));
#24708=CARTESIAN_POINT('Ctrl Pts',(22.7228988539051,-50.4310163552227,-40.));
#24709=CARTESIAN_POINT('Ctrl Pts',(22.7235594196372,-50.4170633417972,-40.));
#24710=CARTESIAN_POINT('Ctrl Pts',(22.7241121360516,-50.4030977822463,-40.));
#24711=CARTESIAN_POINT('Ctrl Pts',(22.7245568821007,-50.389134351788,-40.));
#24712=CARTESIAN_POINT('Ctrl Pts',(22.7275259772316,-50.2959154160083,-40.));
#24713=CARTESIAN_POINT('Ctrl Pts',(22.7256954800801,-50.202635958812,-40.));
#24714=CARTESIAN_POINT('Ctrl Pts',(22.7192004014839,-50.1096716609144,-40.));
#24715=CARTESIAN_POINT('Ctrl Pts',(22.712694547308,-50.0165531317502,-40.));
#24716=CARTESIAN_POINT('Ctrl Pts',(22.7015082431827,-49.9237498276012,-40.));
#24717=CARTESIAN_POINT('Ctrl Pts',(22.6857262377269,-49.8316513834847,-40.));
#24718=CARTESIAN_POINT('Ctrl Pts',(22.6701704615353,-49.7408731368111,-40.));
#24719=CARTESIAN_POINT('Ctrl Pts',(22.6501493336621,-49.6507788422637,-40.));
#24720=CARTESIAN_POINT('Ctrl Pts',(22.6257009917886,-49.5617668173943,-40.));
#24721=CARTESIAN_POINT('Ctrl Pts',(22.6166026728921,-49.5286414712221,-40.));
#24722=CARTESIAN_POINT('Ctrl Pts',(22.6068908241138,-49.4956663271259,-40.));
#24723=CARTESIAN_POINT('Ctrl Pts',(22.5965660505575,-49.4628631797602,-40.));
#24724=CARTESIAN_POINT('Ctrl Pts',(22.5895982917682,-49.4407257045769,-40.));
#24725=CARTESIAN_POINT('Ctrl Pts',(22.5823513715533,-49.418666577747,-40.));
#24726=CARTESIAN_POINT('Ctrl Pts',(22.5748252991941,-49.3966927085346,-40.));
#24727=CARTESIAN_POINT('Ctrl Pts',(22.5698112245824,-49.3820531177256,-40.));
#24728=CARTESIAN_POINT('Ctrl Pts',(22.564673834239,-49.3674532968898,-40.));
#24729=CARTESIAN_POINT('Ctrl Pts',(22.5594172561101,-49.3529059808729,-40.));
#24730=CARTESIAN_POINT('Ctrl Pts',(22.527768723656,-49.2653202565106,-40.));
#24731=CARTESIAN_POINT('Ctrl Pts',(22.4917659891604,-49.1795245866921,-40.));
#24732=CARTESIAN_POINT('Ctrl Pts',(22.4514723792244,-49.0959295354423,-40.));
#24733=CARTESIAN_POINT('Ctrl Pts',(22.4212521717724,-49.033233247005,-40.));
#24734=CARTESIAN_POINT('Ctrl Pts',(22.3886173177637,-48.971775295946,-40.));
#24735=CARTESIAN_POINT('Ctrl Pts',(22.3535788443229,-48.9117442537613,-40.));
#24736=CARTESIAN_POINT('Ctrl Pts',(22.339751300498,-48.8880536706635,-40.));
#24737=CARTESIAN_POINT('Ctrl Pts',(22.3255492797115,-48.8645854808741,-40.));
#24738=CARTESIAN_POINT('Ctrl Pts',(22.3109729414368,-48.8413519730355,-40.));
#24739=CARTESIAN_POINT('Ctrl Pts',(22.30148687725,-48.8262319516358,-40.));
#24740=CARTESIAN_POINT('Ctrl Pts',(22.2918421409525,-48.8112113122026,-40.));
#24741=CARTESIAN_POINT('Ctrl Pts',(22.2820470683987,-48.796305696781,-40.));
#24742=CARTESIAN_POINT('Ctrl Pts',(22.2348460902122,-48.7244777828469,-40.));
#24743=CARTESIAN_POINT('Ctrl Pts',(22.1841115061796,-48.6552447286811,-40.));
#24744=CARTESIAN_POINT('Ctrl Pts',(22.1298762142565,-48.5889589949056,-40.));
#24745=CARTESIAN_POINT('Ctrl Pts',(22.0811918382369,-48.5294575250427,-40.));
#24746=CARTESIAN_POINT('Ctrl Pts',(22.0296860640005,-48.4723310319801,-40.));
#24747=CARTESIAN_POINT('Ctrl Pts',(21.9753623932829,-48.4178640169946,-40.));
#24748=CARTESIAN_POINT('Ctrl Pts',(21.9562793980543,-48.3987306673266,-40.));
#24749=CARTESIAN_POINT('Ctrl Pts',(21.9368485049632,-48.3799257876768,-40.));
#24750=CARTESIAN_POINT('Ctrl Pts',(21.917080287283,-48.3614538548662,-40.));
#24751=CARTESIAN_POINT('Ctrl Pts',(18.086534003335,-48.364012796625,-40.));
#24752=CARTESIAN_POINT('Ctrl Pts',(18.0249120467864,-48.4219223043634,-40.));
#24753=CARTESIAN_POINT('Ctrl Pts',(17.9666585528288,-48.4829816337199,-40.));
#24754=CARTESIAN_POINT('Ctrl Pts',(17.9117715849683,-48.5468061809736,-40.));
#24755=CARTESIAN_POINT('Ctrl Pts',(17.8554328022428,-48.6123189509525,-40.));
#24756=CARTESIAN_POINT('Ctrl Pts',(17.80264055923,-48.6807455909207,-40.));
#24757=CARTESIAN_POINT('Ctrl Pts',(17.7534182575179,-48.7517187155437,-40.));
#24758=CARTESIAN_POINT('Ctrl Pts',(17.7028584818801,-48.8246203299024,-40.));
#24759=CARTESIAN_POINT('Ctrl Pts',(17.6560647570637,-48.9002092533494,-40.));
#24760=CARTESIAN_POINT('Ctrl Pts',(17.6130964864067,-48.9781302762513,-40.));
#24761=CARTESIAN_POINT('Ctrl Pts',(17.5941949709457,-49.0124073229323,-40.));
#24762=CARTESIAN_POINT('Ctrl Pts',(17.5760341928623,-49.0471361452102,-40.));
#24763=CARTESIAN_POINT('Ctrl Pts',(17.5586216279894,-49.0822885783659,-40.));
#24764=CARTESIAN_POINT('Ctrl Pts',(17.5486910755096,-49.1023363475942,-40.));
#24765=CARTESIAN_POINT('Ctrl Pts',(17.539003909918,-49.1225219182463,-40.));
#24766=CARTESIAN_POINT('Ctrl Pts',(17.5295617519229,-49.1428402140162,-40.));
#24767=CARTESIAN_POINT('Ctrl Pts',(17.5210540661992,-49.1611476470141,-40.));
#24768=CARTESIAN_POINT('Ctrl Pts',(17.5127429170722,-49.1795685600238,-40.));
#24769=CARTESIAN_POINT('Ctrl Pts',(17.5046431538033,-49.1980674925815,-40.));
#24770=CARTESIAN_POINT('Ctrl Pts',(17.4680646114337,-49.2816086981564,-40.));
#24771=CARTESIAN_POINT('Ctrl Pts',(17.4357469371754,-49.3668332960487,-40.));
#24772=CARTESIAN_POINT('Ctrl Pts',(17.407715666334,-49.4533428436751,-40.));
#24773=CARTESIAN_POINT('Ctrl Pts',(17.3792231832159,-49.541275775409,-40.));
#24774=CARTESIAN_POINT('Ctrl Pts',(17.3551588225761,-49.6305370435133,-40.));
#24775=CARTESIAN_POINT('Ctrl Pts',(17.3355884709166,-49.72074532758,-40.));
#24776=CARTESIAN_POINT('Ctrl Pts',(17.3166112065531,-49.808219813695,-40.));
#24777=CARTESIAN_POINT('Ctrl Pts',(17.3018595365194,-49.8965857029214,-40.));
#24778=CARTESIAN_POINT('Ctrl Pts',(17.2914342702294,-49.9855171579377,-40.));
#24779=CARTESIAN_POINT('Ctrl Pts',(17.2870630038552,-50.0228057094342,-40.));
#24780=CARTESIAN_POINT('Ctrl Pts',(17.2834528721364,-50.0601938842692,-40.));
#24781=CARTESIAN_POINT('Ctrl Pts',(17.2806136391016,-50.097658280858,-40.));
#24782=CARTESIAN_POINT('Ctrl Pts',(17.2788322041313,-50.1211647649707,-40.));
#24783=CARTESIAN_POINT('Ctrl Pts',(17.2773542809704,-50.1447012611546,-40.));
#24784=CARTESIAN_POINT('Ctrl Pts',(17.2761825773384,-50.1682620220258,-40.));
#24785=CARTESIAN_POINT('Ctrl Pts',(17.2754967486151,-50.1820527504206,-40.));
#24786=CARTESIAN_POINT('Ctrl Pts',(17.2749161233417,-50.1958468418363,-40.));
#24787=CARTESIAN_POINT('Ctrl Pts',(17.2744412045133,-50.2096353105391,-40.));
#24788=CARTESIAN_POINT('Ctrl Pts',(17.2711047392125,-50.3065039639283,-40.));
#24789=CARTESIAN_POINT('Ctrl Pts',(17.2729755345434,-50.4032090699245,-40.));
#24790=CARTESIAN_POINT('Ctrl Pts',(17.2801185032147,-50.4993314325988,-40.));
#24791=CARTESIAN_POINT('Ctrl Pts',(17.2872614718861,-50.5954537952731,-40.));
#24792=CARTESIAN_POINT('Ctrl Pts',(17.2996761825003,-50.6909944574365,-40.));
#24793=CARTESIAN_POINT('Ctrl Pts',(17.3174800113019,-50.7855530099381,-40.));
#24794=CARTESIAN_POINT('Ctrl Pts',(17.3345350799895,-50.8761347957937,-40.));
#24795=CARTESIAN_POINT('Ctrl Pts',(17.3565353752775,-50.965816309671,-40.));
#24796=CARTESIAN_POINT('Ctrl Pts',(17.3832059787172,-51.0543578996475,-40.));
#24797=CARTESIAN_POINT('Ctrl Pts',(17.3920732513301,-51.0837956443795,-40.));
#24798=CARTESIAN_POINT('Ctrl Pts',(17.4014572042998,-51.1131073476298,-40.));
#24799=CARTESIAN_POINT('Ctrl Pts',(17.4113489818483,-51.1422840281894,-40.));
#24800=CARTESIAN_POINT('Ctrl Pts',(17.4206503121436,-51.1697191318883,-40.));
#24801=CARTESIAN_POINT('Ctrl Pts',(17.4304006578653,-51.1970348520032,-40.));
#24802=CARTESIAN_POINT('Ctrl Pts',(17.4405931275984,-51.2242235977629,-40.));
#24803=CARTESIAN_POINT('Ctrl Pts',(17.4457734086336,-51.2380421665416,-40.));
#24804=CARTESIAN_POINT('Ctrl Pts',(17.4510648730829,-51.2518197891935,-40.));
#24805=CARTESIAN_POINT('Ctrl Pts',(17.456464709971,-51.2655518102258,-40.));
#24806=CARTESIAN_POINT('Ctrl Pts',(17.490715740235,-51.3526536760249,-40.));
#24807=CARTESIAN_POINT('Ctrl Pts',(17.529340743901,-51.4379689505696,-40.));
#24808=CARTESIAN_POINT('Ctrl Pts',(17.5720094560872,-51.5212629155659,-40.));
#24809=CARTESIAN_POINT('Ctrl Pts',(17.6162431165096,-51.6076118296556,-40.));
#24810=CARTESIAN_POINT('Ctrl Pts',(17.6648226743584,-51.6917891759745,-40.));
#24811=CARTESIAN_POINT('Ctrl Pts',(17.7174360338155,-51.7735300066221,-40.));
#24812=CARTESIAN_POINT('Ctrl Pts',(17.7706149150164,-51.8561494395403,-40.));
#24813=CARTESIAN_POINT('Ctrl Pts',(17.827915194887,-51.9362805192111,-40.));
#24814=CARTESIAN_POINT('Ctrl Pts',(17.8890661284005,-52.013634320114,-40.));
#24815=CARTESIAN_POINT('Ctrl Pts',(17.9117391701769,-52.0423149282203,-40.));
#24816=CARTESIAN_POINT('Ctrl Pts',(17.9349420408772,-52.0706135254148,-40.));
#24817=CARTESIAN_POINT('Ctrl Pts',(17.9586625307952,-52.0985144997782,-40.));
#24818=CARTESIAN_POINT('Ctrl Pts',(17.9792967362419,-52.1227852648073,-40.));
#24819=CARTESIAN_POINT('Ctrl Pts',(18.0003226424187,-52.14675513991,-40.));
#24820=CARTESIAN_POINT('Ctrl Pts',(18.021732691825,-52.1704134738951,-40.));
#24821=CARTESIAN_POINT('Ctrl Pts',(18.0322751898043,-52.1820630471163,-40.));
#24822=CARTESIAN_POINT('Ctrl Pts',(18.0429077480725,-52.1936336023933,-40.));
#24823=CARTESIAN_POINT('Ctrl Pts',(18.053623710656,-52.205118119964,-40.));
#24824=CARTESIAN_POINT('Ctrl Pts',(18.1224864208474,-52.2789197032564,-40.));
#24825=CARTESIAN_POINT('Ctrl Pts',(18.1948566984041,-52.3492444555942,-40.));
#24826=CARTESIAN_POINT('Ctrl Pts',(18.2704248223711,-52.4158013759963,-40.));
#24827=CARTESIAN_POINT('Ctrl Pts',(18.3329140343801,-52.4708389935967,-40.));
#24828=CARTESIAN_POINT('Ctrl Pts',(18.397591040769,-52.5233001055479,-40.));
#24829=CARTESIAN_POINT('Ctrl Pts',(18.4643035650292,-52.5730066630244,-40.));
#24830=CARTESIAN_POINT('Ctrl Pts',(18.4874416953864,-52.5902465564215,-40.));
#24831=CARTESIAN_POINT('Ctrl Pts',(18.5108248507278,-52.6071549623375,-40.));
#24832=CARTESIAN_POINT('Ctrl Pts',(18.5344471800034,-52.6237239909632,-40.));
#24833=CARTESIAN_POINT('Ctrl Pts',(18.5545056123854,-52.6377932529926,-40.));
#24834=CARTESIAN_POINT('Ctrl Pts',(18.5747397224013,-52.6516198045524,-40.));
#24835=CARTESIAN_POINT('Ctrl Pts',(18.5951234326702,-52.6651840620199,-40.));
#24836=CARTESIAN_POINT('Ctrl Pts',(18.6800750900225,-52.7217147984472,-40.));
#24837=CARTESIAN_POINT('Ctrl Pts',(18.7676928928528,-52.773743896814,-40.));
#24838=CARTESIAN_POINT('Ctrl Pts',(18.857686322517,-52.8209628481135,-40.));
#24839=CARTESIAN_POINT('Ctrl Pts',(18.9406316584209,-52.8644837117052,-40.));
#24840=CARTESIAN_POINT('Ctrl Pts',(19.0255959104309,-52.9039185971562,-40.));
#24841=CARTESIAN_POINT('Ctrl Pts',(19.1123786609832,-52.9389975140129,-40.));
#24842=CARTESIAN_POINT('Ctrl Pts',(19.1428109210872,-52.951298699619,-40.));
#24843=CARTESIAN_POINT('Ctrl Pts',(19.173467007344,-52.9630639420694,-40.));
#24844=CARTESIAN_POINT('Ctrl Pts',(19.2043340224364,-52.9742969733088,-40.));
#24845=CARTESIAN_POINT('Ctrl Pts',(20.7937992825328,47.0307770462543,-40.));
#24846=CARTESIAN_POINT('Ctrl Pts',(20.8868641717184,47.0648205984365,-40.));
#24847=CARTESIAN_POINT('Ctrl Pts',(20.9778637814419,47.1036307868822,-40.));
#24848=CARTESIAN_POINT('Ctrl Pts',(21.0665894075274,47.1468798494389,-40.));
#24849=CARTESIAN_POINT('Ctrl Pts',(21.1572748647162,47.1910842262801,-40.));
#24850=CARTESIAN_POINT('Ctrl Pts',(21.245585438308,47.23992635686,-40.));
#24851=CARTESIAN_POINT('Ctrl Pts',(21.3312693624983,47.2931018031361,-40.));
#24852=CARTESIAN_POINT('Ctrl Pts',(21.4136988092816,47.3442575206223,-40.));
#24853=CARTESIAN_POINT('Ctrl Pts',(21.4936976334333,47.3994245014315,-40.));
#24854=CARTESIAN_POINT('Ctrl Pts',(21.5710087163438,47.4583617309845,-40.));
#24855=CARTESIAN_POINT('Ctrl Pts',(21.6386559138905,47.5099318068434,-40.));
#24856=CARTESIAN_POINT('Ctrl Pts',(21.7042450194051,47.5643891760566,-40.));
#24857=CARTESIAN_POINT('Ctrl Pts',(21.7675791636027,47.6215850793763,-40.));
#24858=CARTESIAN_POINT('Ctrl Pts',(21.7817033221825,47.6343403477839,-40.));
#24859=CARTESIAN_POINT('Ctrl Pts',(21.7957179630638,47.6472345357438,-40.));
#24860=CARTESIAN_POINT('Ctrl Pts',(21.8096013552832,47.6602475006384,-40.));
#24861=CARTESIAN_POINT('Ctrl Pts',(21.8820340261626,47.7281389632204,-40.));
#24862=CARTESIAN_POINT('Ctrl Pts',(21.9510010606037,47.7993516594532,-40.));
#24863=CARTESIAN_POINT('Ctrl Pts',(22.0162623892813,47.8735955768846,-40.));
#24864=CARTESIAN_POINT('Ctrl Pts',(22.0811617452106,47.9474276995307,-40.));
#24865=CARTESIAN_POINT('Ctrl Pts',(22.1423968751173,48.0242583069407,-40.));
#24866=CARTESIAN_POINT('Ctrl Pts',(22.1996880780212,48.1038289540701,-40.));
#24867=CARTESIAN_POINT('Ctrl Pts',(22.2548538529654,48.1804476352851,-40.));
#24868=CARTESIAN_POINT('Ctrl Pts',(22.306363065324,48.2596075597805,-40.));
#24869=CARTESIAN_POINT('Ctrl Pts',(22.3539211533538,48.3410915983807,-40.));
#24870=CARTESIAN_POINT('Ctrl Pts',(22.3738668610994,48.3752657396715,-40.));
#24871=CARTESIAN_POINT('Ctrl Pts',(22.3931170218359,48.4098487847799,-40.));
#24872=CARTESIAN_POINT('Ctrl Pts',(22.4116473225538,48.4448250152362,-40.));
#24873=CARTESIAN_POINT('Ctrl Pts',(22.4245264566452,48.4691345808995,-40.));
#24874=CARTESIAN_POINT('Ctrl Pts',(22.4370578168709,48.4936340846175,-40.));
#24875=CARTESIAN_POINT('Ctrl Pts',(22.4492327746705,48.5183182550832,-40.));
#24876=CARTESIAN_POINT('Ctrl Pts',(22.4571464007594,48.5343627702754,-40.));
#24877=CARTESIAN_POINT('Ctrl Pts',(22.4649105648593,48.5504879313153,-40.));
#24878=CARTESIAN_POINT('Ctrl Pts',(22.4725127056892,48.5666700716157,-40.));
#24879=CARTESIAN_POINT('Ctrl Pts',(22.5146351538768,48.6563331522688,-40.));
#24880=CARTESIAN_POINT('Ctrl Pts',(22.5518582329025,48.7478820741464,-40.));
#24881=CARTESIAN_POINT('Ctrl Pts',(22.5838905234092,48.8410452138574,-40.));
#24882=CARTESIAN_POINT('Ctrl Pts',(22.6137694553261,48.9279454968081,-40.));
#24883=CARTESIAN_POINT('Ctrl Pts',(22.6391318644434,49.0162510530317,-40.));
#24884=CARTESIAN_POINT('Ctrl Pts',(22.6596907050679,49.1057501651513,-40.));
#24885=CARTESIAN_POINT('Ctrl Pts',(22.6611723696795,49.1122003181352,-40.));
#24886=CARTESIAN_POINT('Ctrl Pts',(22.6626290619652,49.1186566716347,-40.));
#24887=CARTESIAN_POINT('Ctrl Pts',(22.6640606638213,49.1251191467213,-40.));
#24888=CARTESIAN_POINT('Ctrl Pts',(22.6846662259577,49.2181358827524,-40.));
#24889=CARTESIAN_POINT('Ctrl Pts',(22.7000780597252,49.3124218036144,-40.));
#24890=CARTESIAN_POINT('Ctrl Pts',(22.7103732018717,49.4075684336347,-40.));
#24891=CARTESIAN_POINT('Ctrl Pts',(22.7161682730423,49.4611258770159,-40.));
#24892=CARTESIAN_POINT('Ctrl Pts',(22.7203411947628,49.514955847025,-40.));
#24893=CARTESIAN_POINT('Ctrl Pts',(22.7228989460627,49.5689828545753,-40.));
#24894=CARTESIAN_POINT('Ctrl Pts',(22.7235595110321,49.5829358720506,-40.));
#24895=CARTESIAN_POINT('Ctrl Pts',(22.7241122266512,49.5969014357913,-40.));
#24896=CARTESIAN_POINT('Ctrl Pts',(22.7245569718737,49.61086487056,-40.));
#24897=CARTESIAN_POINT('Ctrl Pts',(22.7275260613783,49.7040838317261,-40.));
#24898=CARTESIAN_POINT('Ctrl Pts',(22.7256955575492,49.797363319751,-40.));
#24899=CARTESIAN_POINT('Ctrl Pts',(22.7192004715102,49.8903276524339,-40.));
#24900=CARTESIAN_POINT('Ctrl Pts',(22.7126946099576,49.9834462153179,-40.));
#24901=CARTESIAN_POINT('Ctrl Pts',(22.7015082978001,50.0762495571672,-40.));
#24902=CARTESIAN_POINT('Ctrl Pts',(22.6857262839338,50.1683480415187,-40.));
#24903=CARTESIAN_POINT('Ctrl Pts',(22.6701705009221,50.2591263192725,-40.));
#24904=CARTESIAN_POINT('Ctrl Pts',(22.6501493667039,50.3492206474941,-40.));
#24905=CARTESIAN_POINT('Ctrl Pts',(22.6257010192203,50.4382327073517,-40.));
#24906=CARTESIAN_POINT('Ctrl Pts',(22.6166027019945,50.4713580528603,-40.));
#24907=CARTESIAN_POINT('Ctrl Pts',(22.6068908554958,50.5043331965987,-40.));
#24908=CARTESIAN_POINT('Ctrl Pts',(22.5965660848416,50.5371363438728,-40.));
#24909=CARTESIAN_POINT('Ctrl Pts',(22.5895984002548,50.5592735894651,-40.));
#24910=CARTESIAN_POINT('Ctrl Pts',(22.5823515603147,50.5813324884496,-40.));
#24911=CARTESIAN_POINT('Ctrl Pts',(22.5748255743073,50.6033061317659,-40.));
#24912=CARTESIAN_POINT('Ctrl Pts',(22.5698115155151,50.6179456938587,-40.));
#24913=CARTESIAN_POINT('Ctrl Pts',(22.5646741414619,50.6325454866863,-40.));
#24914=CARTESIAN_POINT('Ctrl Pts',(22.5594175802594,50.647092774896,-40.));
#24915=CARTESIAN_POINT('Ctrl Pts',(22.5277690412619,50.734678631977,-40.));
#24916=CARTESIAN_POINT('Ctrl Pts',(22.4917662925164,50.8204744325049,-40.));
#24917=CARTESIAN_POINT('Ctrl Pts',(22.4514726612107,50.9040696099987,-40.));
#24918=CARTESIAN_POINT('Ctrl Pts',(22.4212524377315,50.9667659931192,-40.));
#24919=CARTESIAN_POINT('Ctrl Pts',(22.3886175636867,51.028224036349,-40.));
#24920=CARTESIAN_POINT('Ctrl Pts',(22.353579066392,51.0882551670977,-40.));
#24921=CARTESIAN_POINT('Ctrl Pts',(22.3397516120993,51.1119456156231,-40.));
#24922=CARTESIAN_POINT('Ctrl Pts',(22.325549685609,51.1354136734597,-40.));
#24923=CARTESIAN_POINT('Ctrl Pts',(22.310973446402,51.1586470521603,-40.));
#24924=CARTESIAN_POINT('Ctrl Pts',(22.3014872869241,51.1737672441684,-40.));
#24925=CARTESIAN_POINT('Ctrl Pts',(22.291842451823,51.1887880523519,-40.));
#24926=CARTESIAN_POINT('Ctrl Pts',(22.2820472773129,51.2036938339823,-40.));
#24927=CARTESIAN_POINT('Ctrl Pts',(22.2348463161877,51.2755217752358,-40.));
#24928=CARTESIAN_POINT('Ctrl Pts',(22.1841117513564,51.3447548552043,-40.));
#24929=CARTESIAN_POINT('Ctrl Pts',(22.1298764810566,51.4110406123198,-40.));
#24930=CARTESIAN_POINT('Ctrl Pts',(22.0811919981176,51.4705422575325,-40.));
#24931=CARTESIAN_POINT('Ctrl Pts',(22.0296861042788,51.5276689116495,-40.));
#24932=CARTESIAN_POINT('Ctrl Pts',(21.9753623015053,51.5821360704448,-40.));
#24933=CARTESIAN_POINT('Ctrl Pts',(21.9562793052671,51.6012694251315,-40.));
#24934=CARTESIAN_POINT('Ctrl Pts',(21.9368484112827,51.6200743092308,-40.));
#24935=CARTESIAN_POINT('Ctrl Pts',(21.9170801928212,51.6385462459494,-40.));
#24936=CARTESIAN_POINT('Ctrl Pts',(18.086534003335,51.635987203375,-40.));
#24937=CARTESIAN_POINT('Ctrl Pts',(18.0249120118231,51.5780776627796,-40.));
#24938=CARTESIAN_POINT('Ctrl Pts',(17.9666584811321,51.517018302892,-40.));
#24939=CARTESIAN_POINT('Ctrl Pts',(17.9117714759284,51.4531937268802,-40.));
#24940=CARTESIAN_POINT('Ctrl Pts',(17.8554326587671,51.387680931912,-40.));
#24941=CARTESIAN_POINT('Ctrl Pts',(17.8026403801833,51.3192542692251,-40.));
#24942=CARTESIAN_POINT('Ctrl Pts',(17.753418042989,51.2482811234662,-40.));
#24943=CARTESIAN_POINT('Ctrl Pts',(17.7028582625625,51.1753795330443,-40.));
#24944=CARTESIAN_POINT('Ctrl Pts',(17.6560645283358,51.0997906385659,-40.));
#24945=CARTESIAN_POINT('Ctrl Pts',(17.6130962448594,51.0218696482571,-40.));
#24946=CARTESIAN_POINT('Ctrl Pts',(17.5941947509285,50.9875926651839,-40.));
#24947=CARTESIAN_POINT('Ctrl Pts',(17.5760339915857,50.9528639085148,-40.));
#24948=CARTESIAN_POINT('Ctrl Pts',(17.5586214427303,50.9177115427326,-40.));
#24949=CARTESIAN_POINT('Ctrl Pts',(17.5486908909937,50.8976637949869,-40.));
#24950=CARTESIAN_POINT('Ctrl Pts',(17.5390037256709,50.8774782461587,-40.));
#24951=CARTESIAN_POINT('Ctrl Pts',(17.5295615674849,50.857159972524,-40.));
#24952=CARTESIAN_POINT('Ctrl Pts',(17.5210538764243,50.8388525483564,-40.));
#24953=CARTESIAN_POINT('Ctrl Pts',(17.5127427218279,50.8204316443034,-40.));
#24954=CARTESIAN_POINT('Ctrl Pts',(17.5046429529782,50.801932720795,-40.));
#24955=CARTESIAN_POINT('Ctrl Pts',(17.4680643678851,50.7183915160718,-40.));
#24956=CARTESIAN_POINT('Ctrl Pts',(17.4357466526846,50.6331669193299,-40.));
#24957=CARTESIAN_POINT('Ctrl Pts',(17.4077153439705,50.54665737229,-40.));
#24958=CARTESIAN_POINT('Ctrl Pts',(17.3792228278356,50.4587244580619,-40.));
#24959=CARTESIAN_POINT('Ctrl Pts',(17.3551584356458,50.3694632073917,-40.));
#24960=CARTESIAN_POINT('Ctrl Pts',(17.335588055227,50.2792549395642,-40.));
#24961=CARTESIAN_POINT('Ctrl Pts',(17.3166107688801,50.191780496411,-40.));
#24962=CARTESIAN_POINT('Ctrl Pts',(17.3018590768574,50.1034146495783,-40.));
#24963=CARTESIAN_POINT('Ctrl Pts',(17.2914337897018,50.0144832350641,-40.));
#24964=CARTESIAN_POINT('Ctrl Pts',(17.2870625173661,49.9771947243273,-40.));
#24965=CARTESIAN_POINT('Ctrl Pts',(17.2834523789126,49.9398065900466,-40.));
#24966=CARTESIAN_POINT('Ctrl Pts',(17.2806131384336,49.9023422336642,-40.));
#24967=CARTESIAN_POINT('Ctrl Pts',(17.2788316977985,49.8788357616608,-40.));
#24968=CARTESIAN_POINT('Ctrl Pts',(17.2773537690321,49.8552992774157,-40.));
#24969=CARTESIAN_POINT('Ctrl Pts',(17.2761820598737,49.8317385282873,-40.));
#24970=CARTESIAN_POINT('Ctrl Pts',(17.2754962276114,49.8179478006491,-40.));
#24971=CARTESIAN_POINT('Ctrl Pts',(17.2749155989209,49.8041537099236,-40.));
#24972=CARTESIAN_POINT('Ctrl Pts',(17.2744406768029,49.7903652418327,-40.));
#24973=CARTESIAN_POINT('Ctrl Pts',(17.2711041892475,49.6934966175952,-40.));
#24974=CARTESIAN_POINT('Ctrl Pts',(17.2729749659192,49.5967915369097,-40.));
#24975=CARTESIAN_POINT('Ctrl Pts',(17.2801179208972,49.5006691942515,-40.));
#24976=CARTESIAN_POINT('Ctrl Pts',(17.2872608758751,49.4045468515933,-40.));
#24977=CARTESIAN_POINT('Ctrl Pts',(17.2996755777587,49.3090062041544,-40.));
#24978=CARTESIAN_POINT('Ctrl Pts',(17.3174794041662,49.214447659627,-40.));
#24979=CARTESIAN_POINT('Ctrl Pts',(17.334534466704,49.1238659018917,-40.));
#24980=CARTESIAN_POINT('Ctrl Pts',(17.3565347594197,49.0341844095363,-40.));
#24981=CARTESIAN_POINT('Ctrl Pts',(17.3832053630372,48.9456428353218,-40.));
#24982=CARTESIAN_POINT('Ctrl Pts',(17.3920726307165,48.9162051124052,-40.));
#24983=CARTESIAN_POINT('Ctrl Pts',(17.4014565784749,48.8868934301911,-40.));
#24984=CARTESIAN_POINT('Ctrl Pts',(17.4113483505188,48.8577167699025,-40.));
#24985=CARTESIAN_POINT('Ctrl Pts',(17.4206496316742,48.8302818149405,-40.));
#24986=CARTESIAN_POINT('Ctrl Pts',(17.4303999237523,48.8029662417575,-40.));
#24987=CARTESIAN_POINT('Ctrl Pts',(17.4405923354209,48.7757776410274,-40.));
#24988=CARTESIAN_POINT('Ctrl Pts',(17.4457726757404,48.7619589090953,-40.));
#24989=CARTESIAN_POINT('Ctrl Pts',(17.4510642023782,48.7481811235908,-40.));
#24990=CARTESIAN_POINT('Ctrl Pts',(17.45646410399,48.7344489408886,-40.));
#24991=CARTESIAN_POINT('Ctrl Pts',(17.4907151349945,48.6473470917609,-40.));
#24992=CARTESIAN_POINT('Ctrl Pts',(17.5293401405757,48.5620318281544,-40.));
#24993=CARTESIAN_POINT('Ctrl Pts',(17.5720088551052,48.4787378691761,-40.));
#24994=CARTESIAN_POINT('Ctrl Pts',(17.6162425271352,48.3923889434079,-40.));
#24995=CARTESIAN_POINT('Ctrl Pts',(17.6648220988544,48.3082115810238,-40.));
#24996=CARTESIAN_POINT('Ctrl Pts',(17.7174354734165,48.2264707309132,-40.));
#24997=CARTESIAN_POINT('Ctrl Pts',(17.7706143764448,48.1438512681309,-40.));
#24998=CARTESIAN_POINT('Ctrl Pts',(17.8279146804215,48.0637201557371,-40.));
#24999=CARTESIAN_POINT('Ctrl Pts',(17.8890656391782,47.9863663203166,-40.));
#25000=CARTESIAN_POINT('Ctrl Pts',(17.9117386404853,47.9576857624437,-40.));
#25001=CARTESIAN_POINT('Ctrl Pts',(17.9349414685443,47.9293872135568,-40.));
#25002=CARTESIAN_POINT('Ctrl Pts',(17.9586619136712,47.9014862855243,-40.));
#25003=CARTESIAN_POINT('Ctrl Pts',(17.9792958092928,47.8772158793964,-40.));
#25004=CARTESIAN_POINT('Ctrl Pts',(18.0003213937351,47.8532463538005,-40.));
#25005=CARTESIAN_POINT('Ctrl Pts',(18.0217311098025,47.8295883594692,-40.));
#25006=CARTESIAN_POINT('Ctrl Pts',(18.0322734470095,47.8179389497762,-40.));
#25007=CARTESIAN_POINT('Ctrl Pts',(18.0429058427987,47.8063685545443,-40.));
#25008=CARTESIAN_POINT('Ctrl Pts',(18.0536216401407,47.7948841947313,-40.));
#25009=CARTESIAN_POINT('Ctrl Pts',(18.1224843127581,47.7210825274562,-40.));
#25010=CARTESIAN_POINT('Ctrl Pts',(18.1948545546408,47.6507576872252,-40.));
#25011=CARTESIAN_POINT('Ctrl Pts',(18.2704226433781,47.5842006758549,-40.));
#25012=CARTESIAN_POINT('Ctrl Pts',(18.332912008939,47.5291628221304,-40.));
#25013=CARTESIAN_POINT('Ctrl Pts',(18.3975891819685,47.4767014870064,-40.));
#25014=CARTESIAN_POINT('Ctrl Pts',(18.4643018838579,47.4269947212888,-40.));
#25015=CARTESIAN_POINT('Ctrl Pts',(18.487439448026,47.40975522343,-40.));
#25016=CARTESIAN_POINT('Ctrl Pts',(18.5108220252072,47.3928471968628,-40.));
#25017=CARTESIAN_POINT('Ctrl Pts',(18.534443764743,47.3762785308372,-40.));
#25018=CARTESIAN_POINT('Ctrl Pts',(18.5545032544247,47.3622084838503,-40.));
#25019=CARTESIAN_POINT('Ctrl Pts',(18.5747384411063,47.3483811726599,-40.));
#25020=CARTESIAN_POINT('Ctrl Pts',(18.5951232442218,47.3348161834234,-40.));
#25021=CARTESIAN_POINT('Ctrl Pts',(18.6800749291183,47.2782854097527,-40.));
#25022=CARTESIAN_POINT('Ctrl Pts',(18.7676927569613,47.2262562766525,-40.));
#25023=CARTESIAN_POINT('Ctrl Pts',(18.8576862078851,47.1790372942811,-40.));
#25024=CARTESIAN_POINT('Ctrl Pts',(18.9406316367841,47.1355163635382,-40.));
#25025=CARTESIAN_POINT('Ctrl Pts',(19.0255959821725,47.0960814212715,-40.));
#25026=CARTESIAN_POINT('Ctrl Pts',(19.1123788250024,47.0610024595712,-40.));
#25027=CARTESIAN_POINT('Ctrl Pts',(19.1428110902835,47.0487012692271,-40.));
#25028=CARTESIAN_POINT('Ctrl Pts',(19.1734671811829,47.0369360225547,-40.));
#25029=CARTESIAN_POINT('Ctrl Pts',(19.2043342004084,47.0257029875827,-40.));
#25030=CARTESIAN_POINT('Ctrl Pts',(-19.2062007174672,47.0307770462543,-40.));
#25031=CARTESIAN_POINT('Ctrl Pts',(-19.113135789485,47.0648206126285,-40.));
#25032=CARTESIAN_POINT('Ctrl Pts',(-19.0221361412093,47.1036308098944,-40.));
#25033=CARTESIAN_POINT('Ctrl Pts',(-18.9334104774012,47.1468798773863,-40.));
#25034=CARTESIAN_POINT('Ctrl Pts',(-18.8427250013391,47.1910842496773,-40.));
#25035=CARTESIAN_POINT('Ctrl Pts',(-18.7544144087091,47.2399263696347,-40.));
#25036=CARTESIAN_POINT('Ctrl Pts',(-18.6687304658127,47.2931018009917,-40.));
#25037=CARTESIAN_POINT('Ctrl Pts',(-18.5863010240148,47.3442574898636,-40.));
#25038=CARTESIAN_POINT('Ctrl Pts',(-18.5063022038013,47.3994244358441,-40.));
#25039=CARTESIAN_POINT('Ctrl Pts',(-18.4289911240327,47.4583616261313,-40.));
#25040=CARTESIAN_POINT('Ctrl Pts',(-18.3613439292353,47.5099316676326,-40.));
#25041=CARTESIAN_POINT('Ctrl Pts',(-18.29575482586,47.5643889990892,-40.));
#25042=CARTESIAN_POINT('Ctrl Pts',(-18.2324206833574,47.6215848624513,-40.));
#25043=CARTESIAN_POINT('Ctrl Pts',(-18.2182965567006,47.6343400934602,-40.));
#25044=CARTESIAN_POINT('Ctrl Pts',(-18.2042819472534,47.6472342432689,-40.));
#25045=CARTESIAN_POINT('Ctrl Pts',(-18.1903985858695,47.6602471693883,-40.));
#25046=CARTESIAN_POINT('Ctrl Pts',(-18.1179659082848,47.7281385867458,-40.));
#25047=CARTESIAN_POINT('Ctrl Pts',(-18.0489988669731,47.7993512360535,-40.));
#25048=CARTESIAN_POINT('Ctrl Pts',(-17.9837375315815,47.8735951067416,-40.));
#25049=CARTESIAN_POINT('Ctrl Pts',(-17.9188381766974,47.9474271741188,-40.));
#25050=CARTESIAN_POINT('Ctrl Pts',(-17.8576030471192,48.024257725723,-40.));
#25051=CARTESIAN_POINT('Ctrl Pts',(-17.8003118440444,48.1038283184647,-40.));
#25052=CARTESIAN_POINT('Ctrl Pts',(-17.7451460612301,48.1804469580116,-40.));
#25053=CARTESIAN_POINT('Ctrl Pts',(-17.6936368415585,48.2596068428605,-40.));
#25054=CARTESIAN_POINT('Ctrl Pts',(-17.6460787470823,48.34109084554,-40.));
#25055=CARTESIAN_POINT('Ctrl Pts',(-17.6261330412026,48.3752649639367,-40.));
#25056=CARTESIAN_POINT('Ctrl Pts',(-17.6068828821661,48.4098479866198,-40.));
#25057=CARTESIAN_POINT('Ctrl Pts',(-17.5883525829892,48.444824195261,-40.));
#25058=CARTESIAN_POINT('Ctrl Pts',(-17.5754734589502,48.4691337288093,-40.));
#25059=CARTESIAN_POINT('Ctrl Pts',(-17.5629421082152,48.4936332004423,-40.));
#25060=CARTESIAN_POINT('Ctrl Pts',(-17.5507671593283,48.5183173389123,-40.));
#25061=CARTESIAN_POINT('Ctrl Pts',(-17.5428535180885,48.5343618757708,-40.));
#25062=CARTESIAN_POINT('Ctrl Pts',(-17.5350893393722,48.5504870589659,-40.));
#25063=CARTESIAN_POINT('Ctrl Pts',(-17.5274871845203,48.5666692218289,-40.));
#25064=CARTESIAN_POINT('Ctrl Pts',(-17.485364730287,48.6563322749854,-40.));
#25065=CARTESIAN_POINT('Ctrl Pts',(-17.4481416467071,48.7478811754663,-40.));
#25066=CARTESIAN_POINT('Ctrl Pts',(-17.4161093535095,48.8410443018387,-40.));
#25067=CARTESIAN_POINT('Ctrl Pts',(-17.3862304237933,48.927944558647,-40.));
#25068=CARTESIAN_POINT('Ctrl Pts',(-17.3608680170749,49.0162500952945,-40.));
#25069=CARTESIAN_POINT('Ctrl Pts',(-17.340309179232,49.1057491961777,-40.));
#25070=CARTESIAN_POINT('Ctrl Pts',(-17.338827511346,49.112199363479,-40.));
#25071=CARTESIAN_POINT('Ctrl Pts',(-17.337370815905,49.1186557313683,-40.));
#25072=CARTESIAN_POINT('Ctrl Pts',(-17.3359392110137,49.1251182209172,-40.));
#25073=CARTESIAN_POINT('Ctrl Pts',(-17.3153336507421,49.2181349594804,-40.));
#25074=CARTESIAN_POINT('Ctrl Pts',(-17.2999218207206,49.3124208922995,-40.));
#25075=CARTESIAN_POINT('Ctrl Pts',(-17.2896266838834,49.4075675420277,-40.));
#25076=CARTESIAN_POINT('Ctrl Pts',(-17.2838316166888,49.4611249873763,-40.));
#25077=CARTESIAN_POINT('Ctrl Pts',(-17.2796586988872,49.5149549617163,-40.));
#25078=CARTESIAN_POINT('Ctrl Pts',(-17.2771009513959,49.568981975703,-40.));
#25079=CARTESIAN_POINT('Ctrl Pts',(-17.2764403872718,49.5829349977661,-40.));
#25080=CARTESIAN_POINT('Ctrl Pts',(-17.2758876725352,49.5969005662504,-40.));
#25081=CARTESIAN_POINT('Ctrl Pts',(-17.2754429282314,49.6108640058968,-40.));
#25082=CARTESIAN_POINT('Ctrl Pts',(-17.2724738449968,49.7040829953194,-40.));
#25083=CARTESIAN_POINT('Ctrl Pts',(-17.2743043562655,49.7973625176552,-40.));
#25084=CARTESIAN_POINT('Ctrl Pts',(-17.2807994505954,49.8903268890503,-40.));
#25085=CARTESIAN_POINT('Ctrl Pts',(-17.287305320365,49.9834454894571,-40.));
#25086=CARTESIAN_POINT('Ctrl Pts',(-17.2984916414684,50.0762488732571,-40.));
#25087=CARTESIAN_POINT('Ctrl Pts',(-17.3142736647013,50.1683474023781,-40.));
#25088=CARTESIAN_POINT('Ctrl Pts',(-17.3298294553088,50.2591257147104,-40.));
#25089=CARTESIAN_POINT('Ctrl Pts',(-17.3498505965932,50.3492200803956,-40.));
#25090=CARTESIAN_POINT('Ctrl Pts',(-17.3742989503246,50.4382321791774,-40.));
#25091=CARTESIAN_POINT('Ctrl Pts',(-17.3833972657162,50.4713575240284,-40.));
#25092=CARTESIAN_POINT('Ctrl Pts',(-17.3931091097062,50.5043326674485,-40.));
#25093=CARTESIAN_POINT('Ctrl Pts',(-17.4034338771622,50.5371358146991,-40.));
#25094=CARTESIAN_POINT('Ctrl Pts',(-17.4104014795578,50.5592728060012,-40.));
#25095=CARTESIAN_POINT('Ctrl Pts',(-17.4176482305802,50.5813314526292,-40.));
#25096=CARTESIAN_POINT('Ctrl Pts',(-17.4251741209375,50.6033048457485,-40.));
#25097=CARTESIAN_POINT('Ctrl Pts',(-17.430188162207,50.6179443760499,-40.));
#25098=CARTESIAN_POINT('Ctrl Pts',(-17.4353255182162,50.6325441378708,-40.));
#25099=CARTESIAN_POINT('Ctrl Pts',(-17.4405820606693,50.6470913952962,-40.));
#25100=CARTESIAN_POINT('Ctrl Pts',(-17.472230606961,50.7346773996235,-40.));
#25101=CARTESIAN_POINT('Ctrl Pts',(-17.5082333715373,50.8204733451689,-40.));
#25102=CARTESIAN_POINT('Ctrl Pts',(-17.548527026559,50.9040686627239,-40.));
#25103=CARTESIAN_POINT('Ctrl Pts',(-17.5787472678254,50.9667651508901,-40.));
#25104=CARTESIAN_POINT('Ctrl Pts',(-17.6113821640973,51.0282232963771,-40.));
#25105=CARTESIAN_POINT('Ctrl Pts',(-17.6464206878467,51.0882545253784,-40.));
#25106=CARTESIAN_POINT('Ctrl Pts',(-17.6602480429408,51.1119448248349,-40.));
#25107=CARTESIAN_POINT('Ctrl Pts',(-17.6744498649535,51.1354127365043,-40.));
#25108=CARTESIAN_POINT('Ctrl Pts',(-17.6890259943953,51.1586459721552,-40.));
#25109=CARTESIAN_POINT('Ctrl Pts',(-17.6985122595296,51.1737663533366,-40.));
#25110=CARTESIAN_POINT('Ctrl Pts',(-17.708157204181,51.1887873486326,-40.));
#25111=CARTESIAN_POINT('Ctrl Pts',(-17.7179524917366,51.2036933145573,-40.));
#25112=CARTESIAN_POINT('Ctrl Pts',(-17.7651534339424,51.275521286134,-40.));
#25113=CARTESIAN_POINT('Ctrl Pts',(-17.8158879774711,51.3447543947345,-40.));
#25114=CARTESIAN_POINT('Ctrl Pts',(-17.8701232237717,51.4110401777378,-40.));
#25115=CARTESIAN_POINT('Ctrl Pts',(-17.9188078251789,51.4705420173089,-40.));
#25116=CARTESIAN_POINT('Ctrl Pts',(-17.9703138515323,51.5276688499289,-40.));
#25117=CARTESIAN_POINT('Ctrl Pts',(-18.0246378006122,51.5821361680994,-40.));
#25118=CARTESIAN_POINT('Ctrl Pts',(-18.0437207979735,51.6012695283674,-40.));
#25119=CARTESIAN_POINT('Ctrl Pts',(-18.0631516929516,51.6200744174145,-40.));
#25120=CARTESIAN_POINT('Ctrl Pts',(-18.0829199122823,51.6385463584782,-40.));
#25121=CARTESIAN_POINT('Ctrl Pts',(-21.913465996665,51.635987203375,-40.));
#25122=CARTESIAN_POINT('Ctrl Pts',(-21.9750878942349,51.5780777510621,-40.));
#25123=CARTESIAN_POINT('Ctrl Pts',(-22.0333413262282,51.5170184732071,-40.));
#25124=CARTESIAN_POINT('Ctrl Pts',(-22.0882282310954,51.4531939744632,-40.));
#25125=CARTESIAN_POINT('Ctrl Pts',(-22.1445669557314,51.3876812466377,-40.));
#25126=CARTESIAN_POINT('Ctrl Pts',(-22.1973591387396,51.3192546449921,-40.));
#25127=CARTESIAN_POINT('Ctrl Pts',(-22.2465813805965,51.2482815560211,-40.));
#25128=CARTESIAN_POINT('Ctrl Pts',(-22.2971411481564,51.175379901281,-40.));
#25129=CARTESIAN_POINT('Ctrl Pts',(-22.3439348570983,51.0997909289638,-40.));
#25130=CARTESIAN_POINT('Ctrl Pts',(-22.3869031061299,51.0218698510766,-40.));
#25131=CARTESIAN_POINT('Ctrl Pts',(-22.4058046579096,50.9875926970939,-40.));
#25132=CARTESIAN_POINT('Ctrl Pts',(-22.4239654676059,50.9528637641387,-40.));
#25133=CARTESIAN_POINT('Ctrl Pts',(-22.4413780594982,50.9177112173285,-40.));
#25134=CARTESIAN_POINT('Ctrl Pts',(-22.4513086132313,50.8976634118604,-40.));
#25135=CARTESIAN_POINT('Ctrl Pts',(-22.4609957792757,50.8774778043928,-40.));
#25136=CARTESIAN_POINT('Ctrl Pts',(-22.4704379369484,50.8571594712822,-40.));
#25137=CARTESIAN_POINT('Ctrl Pts',(-22.4789456136821,50.8388520233592,-40.));
#25138=CARTESIAN_POINT('Ctrl Pts',(-22.4872567535947,50.8204310952107,-40.));
#25139=CARTESIAN_POINT('Ctrl Pts',(-22.4953565074608,50.801932147358,-40.));
#25140=CARTESIAN_POINT('Ctrl Pts',(-22.5319349777541,50.7183909403439,-40.));
#25141=CARTESIAN_POINT('Ctrl Pts',(-22.5642525829406,50.6331663405078,-40.));
#25142=CARTESIAN_POINT('Ctrl Pts',(-22.5922837898878,50.5466567918879,-40.));
#25143=CARTESIAN_POINT('Ctrl Pts',(-22.6207762173038,50.4587238306182,-40.));
#25144=CARTESIAN_POINT('Ctrl Pts',(-22.6448405247148,50.3694625330981,-40.));
#25145=CARTESIAN_POINT('Ctrl Pts',(-22.6644108278527,50.2792542216303,-40.));
#25146=CARTESIAN_POINT('Ctrl Pts',(-22.6833880551243,50.1917796630377,-40.));
#25147=CARTESIAN_POINT('Ctrl Pts',(-22.6981396880567,50.1034137022911,-40.));
#25148=CARTESIAN_POINT('Ctrl Pts',(-22.7085649191393,50.0144821789446,-40.));
#25149=CARTESIAN_POINT('Ctrl Pts',(-22.712936175452,49.9771935586975,-40.));
#25150=CARTESIAN_POINT('Ctrl Pts',(-22.7165462958052,49.9398053154584,-40.));
#25151=CARTESIAN_POINT('Ctrl Pts',(-22.719385516278,49.9023408510524,-40.));
#25152=CARTESIAN_POINT('Ctrl Pts',(-22.7211669416888,49.878834346527,-40.));
#25153=CARTESIAN_POINT('Ctrl Pts',(-22.7226448553907,49.8552978302179,-40.));
#25154=CARTESIAN_POINT('Ctrl Pts',(-22.7238165496974,49.8317370495525,-40.));
#25155=CARTESIAN_POINT('Ctrl Pts',(-22.7245023724455,49.817946319965,-40.));
#25156=CARTESIAN_POINT('Ctrl Pts',(-22.7250829919506,49.8041522274683,-40.));
#25157=CARTESIAN_POINT('Ctrl Pts',(-22.725557905227,49.7903637578166,-40.));
#25158=CARTESIAN_POINT('Ctrl Pts',(-22.7288943329894,49.6934950551849,-40.));
#25159=CARTESIAN_POINT('Ctrl Pts',(-22.7270235061783,49.5967899064236,-40.));
#25160=CARTESIAN_POINT('Ctrl Pts',(-22.7198805143962,49.5006675099145,-40.));
#25161=CARTESIAN_POINT('Ctrl Pts',(-22.712737522614,49.4045451134053,-40.));
#25162=CARTESIAN_POINT('Ctrl Pts',(-22.7003227972537,49.3090044263321,-40.));
#25163=CARTESIAN_POINT('Ctrl Pts',(-22.6825189643874,49.2144458603069,-40.));
#25164=CARTESIAN_POINT('Ctrl Pts',(-22.665463885311,49.1238640270008,-40.));
#25165=CARTESIAN_POINT('Ctrl Pts',(-22.6434635856682,49.0341824768018,-40.));
#25166=CARTESIAN_POINT('Ctrl Pts',(-22.616792982512,48.9456408602185,-40.));
#25167=CARTESIAN_POINT('Ctrl Pts',(-22.6079257015727,48.9162030786856,-40.));
#25168=CARTESIAN_POINT('Ctrl Pts',(-22.5985417398083,48.8868913399485,-40.));
#25169=CARTESIAN_POINT('Ctrl Pts',(-22.5886499529707,48.8577146251926,-40.));
#25170=CARTESIAN_POINT('Ctrl Pts',(-22.5793485397899,48.8302792706246,-40.));
#25171=CARTESIAN_POINT('Ctrl Pts',(-22.5695981035871,48.802963302685,-40.));
#25172=CARTESIAN_POINT('Ctrl Pts',(-22.5594055359165,48.7757743123091,-40.));
#25173=CARTESIAN_POINT('Ctrl Pts',(-22.5542253548657,48.7619560186967,-40.));
#25174=CARTESIAN_POINT('Ctrl Pts',(-22.5489339952992,48.7481786707038,-40.));
#25175=CARTESIAN_POINT('Ctrl Pts',(-22.5435342675695,48.7344469223358,-40.));
#25176=CARTESIAN_POINT('Ctrl Pts',(-22.5092832385399,48.6473450284018,-40.));
#25177=CARTESIAN_POINT('Ctrl Pts',(-22.4706582380904,48.5620297353929,-40.));
#25178=CARTESIAN_POINT('Ctrl Pts',(-22.427989529844,48.4787357602314,-40.));
#25179=CARTESIAN_POINT('Ctrl Pts',(-22.3837558889833,48.3923868658173,-40.));
#25180=CARTESIAN_POINT('Ctrl Pts',(-22.3351763545133,48.3082095465738,-40.));
#25181=CARTESIAN_POINT('Ctrl Pts',(-22.2825630205183,48.2264687487337,-40.));
#25182=CARTESIAN_POINT('Ctrl Pts',(-22.2293841761177,48.1438493661654,-40.));
#25183=CARTESIAN_POINT('Ctrl Pts',(-22.1720839368917,48.063718341668,-40.));
#25184=CARTESIAN_POINT('Ctrl Pts',(-22.1109330459416,47.9863645989668,-40.));
#25185=CARTESIAN_POINT('Ctrl Pts',(-22.088259935904,47.9576839061292,-40.));
#25186=CARTESIAN_POINT('Ctrl Pts',(-22.0650569932795,47.9293852274522,-40.));
#25187=CARTESIAN_POINT('Ctrl Pts',(-22.0413364278114,47.9014841749402,-40.));
#25188=CARTESIAN_POINT('Ctrl Pts',(-22.0207016997641,47.87721280453,-40.));
#25189=CARTESIAN_POINT('Ctrl Pts',(-21.9996752508981,47.8532423398925,-40.));
#25190=CARTESIAN_POINT('Ctrl Pts',(-21.978264639229,47.8295834329929,-40.));
#25191=CARTESIAN_POINT('Ctrl Pts',(-21.9677218695906,47.8179335834141,-40.));
#25192=CARTESIAN_POINT('Ctrl Pts',(-21.9570890367767,47.8063627576625,-40.));
#25193=CARTESIAN_POINT('Ctrl Pts',(-21.9463727949803,47.794877973483,-40.));
#25194=CARTESIAN_POINT('Ctrl Pts',(-21.8775100213453,47.7210765318742,-40.));
#25195=CARTESIAN_POINT('Ctrl Pts',(-21.8051396835538,47.6507519278206,-40.));
#25196=CARTESIAN_POINT('Ctrl Pts',(-21.7295715001049,47.5841951608942,-40.));
#25197=CARTESIAN_POINT('Ctrl Pts',(-21.6670825471831,47.5291579417198,-40.));
#25198=CARTESIAN_POINT('Ctrl Pts',(-21.60240582197,47.4766972063418,-40.));
#25199=CARTESIAN_POINT('Ctrl Pts',(-21.535693597432,47.4269910002443,-40.));
#25200=CARTESIAN_POINT('Ctrl Pts',(-21.5125545115,47.4097504392795,-40.));
#25201=CARTESIAN_POINT('Ctrl Pts',(-21.4891703803795,47.3928413931205,-40.));
#25202=CARTESIAN_POINT('Ctrl Pts',(-21.4655470557819,47.3762717525203,-40.));
#25203=CARTESIAN_POINT('Ctrl Pts',(-21.4454904073927,47.362203814958,-40.));
#25204=CARTESIAN_POINT('Ctrl Pts',(-21.4252581140449,47.3483785451348,-40.));
#25205=CARTESIAN_POINT('Ctrl Pts',(-21.4048762477445,47.334815522396,-40.));
#25206=CARTESIAN_POINT('Ctrl Pts',(-21.3199246368295,47.2782848488273,-40.));
#25207=CARTESIAN_POINT('Ctrl Pts',(-21.2323068761709,47.2262558090893,-40.));
#25208=CARTESIAN_POINT('Ctrl Pts',(-21.1423134823526,47.1790369102475,-40.));
#25209=CARTESIAN_POINT('Ctrl Pts',(-21.0593683036803,47.1355161601684,-40.));
#25210=CARTESIAN_POINT('Ctrl Pts',(-20.9744042095711,47.0960813707627,-40.));
#25211=CARTESIAN_POINT('Ctrl Pts',(-20.8876216150834,47.0610025297207,-40.));
#25212=CARTESIAN_POINT('Ctrl Pts',(-20.8571893637145,47.0487013521099,-40.));
#25213=CARTESIAN_POINT('Ctrl Pts',(-20.8265332852914,47.0369361167847,-40.));
#25214=CARTESIAN_POINT('Ctrl Pts',(-20.7956662771738,47.0257030918457,-40.));
#25215=CARTESIAN_POINT('Ctrl Pts',(-19.2062007174672,-52.9692229537457,
-40.));
#25216=CARTESIAN_POINT('Ctrl Pts',(-19.1131357468007,-52.9351793717574,
-40.));
#25217=CARTESIAN_POINT('Ctrl Pts',(-19.0221360561095,-52.8963691647869,
-40.));
#25218=CARTESIAN_POINT('Ctrl Pts',(-18.9334103507984,-52.8531200918645,
-40.));
#25219=CARTESIAN_POINT('Ctrl Pts',(-18.8427248539677,-52.8089157245768,
-40.));
#25220=CARTESIAN_POINT('Ctrl Pts',(-18.7544142403876,-52.7600736163027,
-40.));
#25221=CARTESIAN_POINT('Ctrl Pts',(-18.6687302769065,-52.706898201355,-40.));
#25222=CARTESIAN_POINT('Ctrl Pts',(-18.5863008405935,-52.6557425439628,
-40.));
#25223=CARTESIAN_POINT('Ctrl Pts',(-18.5063020247127,-52.6005756362984,
-40.));
#25224=CARTESIAN_POINT('Ctrl Pts',(-18.4289909484007,-52.5416384892086,
-40.));
#25225=CARTESIAN_POINT('Ctrl Pts',(-18.3613437566276,-52.4900684855051,
-40.));
#25226=CARTESIAN_POINT('Ctrl Pts',(-18.2957546556056,-52.4356111955853,
-40.));
#25227=CARTESIAN_POINT('Ctrl Pts',(-18.2324205149676,-52.3784153761812,
-40.));
#25228=CARTESIAN_POINT('Ctrl Pts',(-18.2182964234727,-52.3656601863538,
-40.));
#25229=CARTESIAN_POINT('Ctrl Pts',(-18.2042818486488,-52.3527660785552,
-40.));
#25230=CARTESIAN_POINT('Ctrl Pts',(-18.1903985212288,-52.3397531951332,
-40.));
#25231=CARTESIAN_POINT('Ctrl Pts',(-18.1179658362636,-52.2718618275319,
-40.));
#25232=CARTESIAN_POINT('Ctrl Pts',(-18.0489987873894,-52.200649229851,-40.));
#25233=CARTESIAN_POINT('Ctrl Pts',(-17.9837374446072,-52.1264054105887,
-40.));
#25234=CARTESIAN_POINT('Ctrl Pts',(-17.9188380908689,-52.0525734040167,
-40.));
#25235=CARTESIAN_POINT('Ctrl Pts',(-17.8576029616476,-51.9757429138075,
-40.));
#25236=CARTESIAN_POINT('Ctrl Pts',(-17.8003117583802,-51.8961723809,-40.));
#25237=CARTESIAN_POINT('Ctrl Pts',(-17.7451459668942,-51.8195537871811,
-40.));
#25238=CARTESIAN_POINT('Ctrl Pts',(-17.693636739165,-51.7403939459348,-40.));
#25239=CARTESIAN_POINT('Ctrl Pts',(-17.6460786375857,-51.6589099827569,
-40.));
#25240=CARTESIAN_POINT('Ctrl Pts',(-17.6261329337694,-51.6247358895667,
-40.));
#25241=CARTESIAN_POINT('Ctrl Pts',(-17.6068827766128,-51.5901528915744,
-40.));
#25242=CARTESIAN_POINT('Ctrl Pts',(-17.5883524791399,-51.5551767069529,
-40.));
#25243=CARTESIAN_POINT('Ctrl Pts',(-17.5754733662171,-51.5308672088453,
-40.));
#25244=CARTESIAN_POINT('Ctrl Pts',(-17.5629420259769,-51.5063677726217,
-40.));
#25245=CARTESIAN_POINT('Ctrl Pts',(-17.5507670869457,-51.4816836694644,
-40.));
#25246=CARTESIAN_POINT('Ctrl Pts',(-17.5428534289798,-51.4656391086596,
-40.));
#25247=CARTESIAN_POINT('Ctrl Pts',(-17.5350892341274,-51.4495139009789,
-40.));
#25248=CARTESIAN_POINT('Ctrl Pts',(-17.5274870637955,-51.433331713181,-40.));
#25249=CARTESIAN_POINT('Ctrl Pts',(-17.4853646028894,-51.3436686902377,
-40.));
#25250=CARTESIAN_POINT('Ctrl Pts',(-17.4481415142809,-51.2521198132569,
-40.));
#25251=CARTESIAN_POINT('Ctrl Pts',(-17.4161092181085,-51.1589567015166,
-40.));
#25252=CARTESIAN_POINT('Ctrl Pts',(-17.3862302908103,-51.0720564734599,
-40.));
#25253=CARTESIAN_POINT('Ctrl Pts',(-17.360867886728,-50.9837509583388,-40.));
#25254=CARTESIAN_POINT('Ctrl Pts',(-17.3403090519426,-50.8942518698057,
-40.));
#25255=CARTESIAN_POINT('Ctrl Pts',(-17.3388273804463,-50.8878016867186,
-40.));
#25256=CARTESIAN_POINT('Ctrl Pts',(-17.3373706815264,-50.8813453029637,
-40.));
#25257=CARTESIAN_POINT('Ctrl Pts',(-17.3359390732883,-50.8748827974692,
-40.));
#25258=CARTESIAN_POINT('Ctrl Pts',(-17.3153335150716,-50.781866056118,-40.));
#25259=CARTESIAN_POINT('Ctrl Pts',(-17.2999216891736,-50.6875801101407,
-40.));
#25260=CARTESIAN_POINT('Ctrl Pts',(-17.2896265581787,-50.5924334387263,
-40.));
#25261=CARTESIAN_POINT('Ctrl Pts',(-17.2838314953604,-50.538875991223,-40.));
#25262=CARTESIAN_POINT('Ctrl Pts',(-17.279658581871,-50.4850460121277,-40.));
#25263=CARTESIAN_POINT('Ctrl Pts',(-17.27710083857,-50.4310189910692,-40.));
#25264=CARTESIAN_POINT('Ctrl Pts',(-17.2764402753775,-50.4170659640024,
-40.));
#25265=CARTESIAN_POINT('Ctrl Pts',(-17.275887561613,-50.4031003903426,-40.));
#25266=CARTESIAN_POINT('Ctrl Pts',(-17.2754428183204,-50.3891369453735,
-40.));
#25267=CARTESIAN_POINT('Ctrl Pts',(-17.2724737419776,-50.2959179248492,
-40.));
#25268=CARTESIAN_POINT('Ctrl Pts',(-17.2743042614248,-50.2026383647503,
-40.));
#25269=CARTESIAN_POINT('Ctrl Pts',(-17.2807993648699,-50.1096739507498,
-40.));
#25270=CARTESIAN_POINT('Ctrl Pts',(-17.2873052436734,-50.0165553090462,
-40.));
#25271=CARTESIAN_POINT('Ctrl Pts',(-17.2984915746125,-49.923751879078,-40.));
#25272=CARTESIAN_POINT('Ctrl Pts',(-17.3142736081437,-49.8316533006875,
-40.));
#25273=CARTESIAN_POINT('Ctrl Pts',(-17.3298294071013,-49.7408749502994,
-40.));
#25274=CARTESIAN_POINT('Ctrl Pts',(-17.3498505561529,-49.6507805433845,
-40.));
#25275=CARTESIAN_POINT('Ctrl Pts',(-17.3742989167507,-49.5617684017665,
-40.));
#25276=CARTESIAN_POINT('Ctrl Pts',(-17.3833972300998,-49.5286430577144,
-40.));
#25277=CARTESIAN_POINT('Ctrl Pts',(-17.3931090713021,-49.4956679147191,
-40.));
#25278=CARTESIAN_POINT('Ctrl Pts',(-17.4034338352087,-49.4628647675681,
-40.));
#25279=CARTESIAN_POINT('Ctrl Pts',(-17.4104013467753,-49.4407280572992,
-40.));
#25280=CARTESIAN_POINT('Ctrl Pts',(-17.417647999536,-49.4186696895679,-40.));
#25281=CARTESIAN_POINT('Ctrl Pts',(-17.4251737841929,-49.3966965729596,
-40.));
#25282=CARTESIAN_POINT('Ctrl Pts',(-17.4301878061034,-49.382057077792,-40.));
#25283=CARTESIAN_POINT('Ctrl Pts',(-17.4353251421779,-49.3674573502381,
-40.));
#25284=CARTESIAN_POINT('Ctrl Pts',(-17.4405816639177,-49.3529101268342,
-40.));
#25285=CARTESIAN_POINT('Ctrl Pts',(-17.4722302182215,-49.2653239600375,
-40.));
#25286=CARTESIAN_POINT('Ctrl Pts',(-17.5082330002425,-49.179527854485,-40.));
#25287=CARTESIAN_POINT('Ctrl Pts',(-17.5485266814233,-49.0959323823922,
-40.));
#25288=CARTESIAN_POINT('Ctrl Pts',(-17.5787469423089,-49.0332357783227,
-40.));
#25289=CARTESIAN_POINT('Ctrl Pts',(-17.6113818631069,-48.9717775200094,
-40.));
#25290=CARTESIAN_POINT('Ctrl Pts',(-17.6464204160553,-48.9117461825991,
-40.));
#25291=CARTESIAN_POINT('Ctrl Pts',(-17.660247661566,-48.8880560478515,-40.));
#25292=CARTESIAN_POINT('Ctrl Pts',(-17.6744493681646,-48.8645882976847,
-40.));
#25293=CARTESIAN_POINT('Ctrl Pts',(-17.6890253763523,-48.841355220092,-40.));
#25294=CARTESIAN_POINT('Ctrl Pts',(-17.6985117582113,-48.8262346299435,
-40.));
#25295=CARTESIAN_POINT('Ctrl Pts',(-17.7081568238899,-48.8112134279567,
-40.));
#25296=CARTESIAN_POINT('Ctrl Pts',(-17.7179522363345,-48.7963072584545,
-40.));
#25297=CARTESIAN_POINT('Ctrl Pts',(-17.7651531576604,-48.7244792534651,
-40.));
#25298=CARTESIAN_POINT('Ctrl Pts',(-17.8158876776876,-48.6552461133118,
-40.));
#25299=CARTESIAN_POINT('Ctrl Pts',(-17.8701228975197,-48.5889603017741,
-40.));
#25300=CARTESIAN_POINT('Ctrl Pts',(-17.9188076297135,-48.5294582477039,
-40.));
#25301=CARTESIAN_POINT('Ctrl Pts',(-17.9703138023661,-48.472331218078,-40.));
#25302=CARTESIAN_POINT('Ctrl Pts',(-18.0246379129771,-48.4178637240035,
-40.));
#25303=CARTESIAN_POINT('Ctrl Pts',(-18.0437209115739,-48.3987303575976,
-40.));
#25304=CARTESIAN_POINT('Ctrl Pts',(-18.0631518076453,-48.3799254631098,
-40.));
#25305=CARTESIAN_POINT('Ctrl Pts',(-18.0829200279321,-48.3614535172687,
-40.));
#25306=CARTESIAN_POINT('Ctrl Pts',(-21.913465996665,-48.364012796625,-40.));
#25307=CARTESIAN_POINT('Ctrl Pts',(-21.9750879218973,-48.4219222749338,
-40.));
#25308=CARTESIAN_POINT('Ctrl Pts',(-22.0333413829535,-48.482981576944,-40.));
#25309=CARTESIAN_POINT('Ctrl Pts',(-22.0882283173664,-48.5468060984396,
-40.));
#25310=CARTESIAN_POINT('Ctrl Pts',(-22.1445670692492,-48.612318846037,-40.));
#25311=CARTESIAN_POINT('Ctrl Pts',(-22.1973592804025,-48.6807454656577,
-40.));
#25312=CARTESIAN_POINT('Ctrl Pts',(-22.2465815503343,-48.751718571351,-40.));
#25313=CARTESIAN_POINT('Ctrl Pts',(-22.2971413216833,-48.8246202071501,
-40.));
#25314=CARTESIAN_POINT('Ctrl Pts',(-22.3439350380711,-48.9002091565446,
-40.));
#25315=CARTESIAN_POINT('Ctrl Pts',(-22.3869032972462,-48.9781302086408,
-40.));
#25316=CARTESIAN_POINT('Ctrl Pts',(-22.4058048319915,-49.0124073122952,
-40.));
#25317=CARTESIAN_POINT('Ctrl Pts',(-22.4239656268606,-49.0471361933387,
-40.));
#25318=CARTESIAN_POINT('Ctrl Pts',(-22.4413782060802,-49.0822886868408,
-40.));
#25319=CARTESIAN_POINT('Ctrl Pts',(-22.4513087592254,-49.1023364753106,
-40.));
#25320=CARTESIAN_POINT('Ctrl Pts',(-22.4609959250573,-49.1225220655097,
-40.));
#25321=CARTESIAN_POINT('Ctrl Pts',(-22.4704380828812,-49.1428403811056,
-40.));
#25322=CARTESIAN_POINT('Ctrl Pts',(-22.4789457638369,-49.161147822039,-40.));
#25323=CARTESIAN_POINT('Ctrl Pts',(-22.4872569080763,-49.1795687430977,
-40.));
#25324=CARTESIAN_POINT('Ctrl Pts',(-22.4953566663574,-49.1980676837875,
-40.));
#25325=CARTESIAN_POINT('Ctrl Pts',(-22.5319351704572,-49.2816088901274,
-40.));
#25326=CARTESIAN_POINT('Ctrl Pts',(-22.5642528080409,-49.3668334890526,
-40.));
#25327=CARTESIAN_POINT('Ctrl Pts',(-22.5922840449568,-49.4533430372071,
-40.));
#25328=CARTESIAN_POINT('Ctrl Pts',(-22.620776498499,-49.5412759846236,-40.));
#25329=CARTESIAN_POINT('Ctrl Pts',(-22.6448408308761,-49.6305372683465,
-40.));
#25330=CARTESIAN_POINT('Ctrl Pts',(-22.6644111567722,-49.7207455669619,
-40.));
#25331=CARTESIAN_POINT('Ctrl Pts',(-22.6833884014399,-49.8082200915544,
-40.));
#25332=CARTESIAN_POINT('Ctrl Pts',(-22.6981400517734,-49.8965860187497,
-40.));
#25333=CARTESIAN_POINT('Ctrl Pts',(-22.7085652993693,-49.9855175100408,
-40.));
#25334=CARTESIAN_POINT('Ctrl Pts',(-22.7129365604003,-50.0228060980321,
-40.));
#25335=CARTESIAN_POINT('Ctrl Pts',(-22.7165466860838,-50.0601943091777,
-40.));
#25336=CARTESIAN_POINT('Ctrl Pts',(-22.7193859124485,-50.0976587417654,
-40.));
#25337=CARTESIAN_POINT('Ctrl Pts',(-22.721167342343,-50.1211652367108,-40.));
#25338=CARTESIAN_POINT('Ctrl Pts',(-22.7226452604816,-50.1447017435747,
-40.));
#25339=CARTESIAN_POINT('Ctrl Pts',(-22.7238169591624,-50.1682625149501,
-40.));
#25340=CARTESIAN_POINT('Ctrl Pts',(-22.7245027847159,-50.1820532440298,
-40.));
#25341=CARTESIAN_POINT('Ctrl Pts',(-22.7250834069287,-50.1958473360712,
-40.));
#25342=CARTESIAN_POINT('Ctrl Pts',(-22.7255583228104,-50.2096358053294,
-40.));
#25343=CARTESIAN_POINT('Ctrl Pts',(-22.7288947681752,-50.3065044848366,
-40.));
#25344=CARTESIAN_POINT('Ctrl Pts',(-22.7270239561279,-50.4032096135111,
-40.));
#25345=CARTESIAN_POINT('Ctrl Pts',(-22.7198809751868,-50.4993319941221,
-40.));
#25346=CARTESIAN_POINT('Ctrl Pts',(-22.7127379942457,-50.5954543747331,
-40.));
#25347=CARTESIAN_POINT('Ctrl Pts',(-22.7003232758061,-50.6909950500943,
-40.));
#25348=CARTESIAN_POINT('Ctrl Pts',(-22.6825194448535,-50.7855536097484,
-40.));
#25349=CARTESIAN_POINT('Ctrl Pts',(-22.6654643706524,-50.8761354207948,
-40.));
#25350=CARTESIAN_POINT('Ctrl Pts',(-22.643464073055,-50.9658169539538,-40.));
#25351=CARTESIAN_POINT('Ctrl Pts',(-22.6167934697688,-51.0543585580536,
-40.));
#25352=CARTESIAN_POINT('Ctrl Pts',(-22.6079261927359,-51.0837963223242,
-40.));
#25353=CARTESIAN_POINT('Ctrl Pts',(-22.5985422350976,-51.1131080444153,
-40.));
#25354=CARTESIAN_POINT('Ctrl Pts',(-22.588650452618,-51.1422847431305,-40.));
#25355=CARTESIAN_POINT('Ctrl Pts',(-22.5793490783144,-51.1697199800305,
-40.));
#25356=CARTESIAN_POINT('Ctrl Pts',(-22.5695986845515,-51.1970358317301,
-40.));
#25357=CARTESIAN_POINT('Ctrl Pts',(-22.5594061628182,-51.2242247073709,
-40.));
#25358=CARTESIAN_POINT('Ctrl Pts',(-22.5542259348717,-51.238043130045,-40.));
#25359=CARTESIAN_POINT('Ctrl Pts',(-22.5489345261121,-51.2518206068617,
-40.));
#25360=CARTESIAN_POINT('Ctrl Pts',(-22.543534747184,-51.2655524831179,-40.));
#25361=CARTESIAN_POINT('Ctrl Pts',(-22.5092837175801,-51.3526543638479,
-40.));
#25362=CARTESIAN_POINT('Ctrl Pts',(-22.4706587156271,-51.4379696481888,
-40.));
#25363=CARTESIAN_POINT('Ctrl Pts',(-22.4279900055383,-51.5212636185752,
-40.));
#25364=CARTESIAN_POINT('Ctrl Pts',(-22.3837563555061,-51.6076125222142,
-40.));
#25365=CARTESIAN_POINT('Ctrl Pts',(-22.3351768100742,-51.6917898541535,
-40.));
#25366=CARTESIAN_POINT('Ctrl Pts',(-22.2825634641401,-51.7735306673781,
-40.));
#25367=CARTESIAN_POINT('Ctrl Pts',(-22.2293846024825,-51.8561500735585,
-40.));
#25368=CARTESIAN_POINT('Ctrl Pts',(-22.1720843441963,-51.9362811239307,
-40.));
#25369=CARTESIAN_POINT('Ctrl Pts',(-22.1109334332859,-52.0136348939272,
-40.));
#25370=CARTESIAN_POINT('Ctrl Pts',(-22.0882603552691,-52.0423155470182,
-40.));
#25371=CARTESIAN_POINT('Ctrl Pts',(-22.0650574463836,-52.0706141874726,
-40.));
#25372=CARTESIAN_POINT('Ctrl Pts',(-22.0413369163553,-52.0985152033257,
-40.));
#25373=CARTESIAN_POINT('Ctrl Pts',(-22.0207024334489,-52.1227862897646,
-40.));
#25374=CARTESIAN_POINT('Ctrl Pts',(-21.9996762391468,-52.146756477864,-40.));
#25375=CARTESIAN_POINT('Ctrl Pts',(-21.9782658912232,-52.1704151160217,
-40.));
#25376=CARTESIAN_POINT('Ctrl Pts',(-21.9677232491215,-52.1820648358488,
-40.));
#25377=CARTESIAN_POINT('Ctrl Pts',(-21.9570905451999,-52.19363553461,-40.));
#25378=CARTESIAN_POINT('Ctrl Pts',(-21.9463744344869,-52.2051201936141,
-40.));
#25379=CARTESIAN_POINT('Ctrl Pts',(-21.8775116906258,-52.2789217016908,
-40.));
#25380=CARTESIAN_POINT('Ctrl Pts',(-21.805141381102,-52.349246375309,-40.));
#25381=CARTESIAN_POINT('Ctrl Pts',(-21.7295732255667,-52.415803214236,-40.));
#25382=CARTESIAN_POINT('Ctrl Pts',(-21.6670841510965,-52.4708406203331,
-40.));
#25383=CARTESIAN_POINT('Ctrl Pts',(-21.6024072939712,-52.5233015323814,
-40.));
#25384=CARTESIAN_POINT('Ctrl Pts',(-21.5356949288188,-52.5730079033295,
-40.));
#25385=CARTESIAN_POINT('Ctrl Pts',(-21.5125562912412,-52.5902481510713,
-40.));
#25386=CARTESIAN_POINT('Ctrl Pts',(-21.4891726179549,-52.6071568968281,
-40.));
#25387=CARTESIAN_POINT('Ctrl Pts',(-21.465549760361,-52.6237262502898,-40.));
#25388=CARTESIAN_POINT('Ctrl Pts',(-21.4454922749805,-52.637794809248,-40.));
#25389=CARTESIAN_POINT('Ctrl Pts',(-21.4252591293115,-52.6516206804198,
-40.));
#25390=CARTESIAN_POINT('Ctrl Pts',(-21.4048763978817,-52.6651842824533,
-40.));
#25391=CARTESIAN_POINT('Ctrl Pts',(-21.3199247651891,-52.7217149855095,
-40.));
#25392=CARTESIAN_POINT('Ctrl Pts',(-21.232306984753,-52.7737440527519,-40.));
#25393=CARTESIAN_POINT('Ctrl Pts',(-21.1423135741234,-52.8209629762043,
-40.));
#25394=CARTESIAN_POINT('Ctrl Pts',(-21.0593683216558,-52.8644837795565,
-40.));
#25395=CARTESIAN_POINT('Ctrl Pts',(-20.9744041534344,-52.9039186140383,
-40.));
#25396=CARTESIAN_POINT('Ctrl Pts',(-20.887621485693,-52.9389974906628,-40.));
#25397=CARTESIAN_POINT('Ctrl Pts',(-20.8571892302267,-52.9512986720242,
-40.));
#25398=CARTESIAN_POINT('Ctrl Pts',(-20.8265331481289,-52.9630639106919,
-40.));
#25399=CARTESIAN_POINT('Ctrl Pts',(-20.7956661367394,-52.9742969385866,
-40.));
#25400=CARTESIAN_POINT('Origin',(-20.,-50.,-25.));
#25401=CARTESIAN_POINT('Ctrl Pts',(-18.0865340033349,-48.3640127966251,
-25.));
#25402=CARTESIAN_POINT('Ctrl Pts',(-18.0243832850997,-48.4224192105103,
-25.));
#25403=CARTESIAN_POINT('Ctrl Pts',(-17.9656071264269,-48.4840785138675,
-25.));
#25404=CARTESIAN_POINT('Ctrl Pts',(-17.9102179711386,-48.5486144685222,
-25.));
#25405=CARTESIAN_POINT('Ctrl Pts',(-17.8534755897244,-48.6147271170159,
-25.));
#25406=CARTESIAN_POINT('Ctrl Pts',(-17.8002872616887,-48.6838591854776,
-25.));
#25407=CARTESIAN_POINT('Ctrl Pts',(-17.7506952446208,-48.7556524546743,
-25.));
#25408=CARTESIAN_POINT('Ctrl Pts',(-17.737728064412,-48.7744247554294,-25.));
#25409=CARTESIAN_POINT('Ctrl Pts',(-17.7250069365578,-48.7933792207731,
-25.));
#25410=CARTESIAN_POINT('Ctrl Pts',(-17.7125329944118,-48.8125098826575,
-25.));
#25411=CARTESIAN_POINT('Ctrl Pts',(-17.702405577042,-48.8280417967225,-25.));
#25412=CARTESIAN_POINT('Ctrl Pts',(-17.6924406896447,-48.8436907013992,
-25.));
#25413=CARTESIAN_POINT('Ctrl Pts',(-17.6826476852539,-48.8594389743045,
-25.));
#25414=CARTESIAN_POINT('Ctrl Pts',(-17.6351883455804,-48.9357590292394,
-25.));
#25415=CARTESIAN_POINT('Ctrl Pts',(-17.5917124377679,-49.0144857272152,
-25.));
#25416=CARTESIAN_POINT('Ctrl Pts',(-17.5522551555271,-49.095226864203,-25.));
#25417=CARTESIAN_POINT('Ctrl Pts',(-17.5204200254773,-49.1603708490493,
-25.));
#25418=CARTESIAN_POINT('Ctrl Pts',(-17.4912013880664,-49.226827255453,-25.));
#25419=CARTESIAN_POINT('Ctrl Pts',(-17.4646348766623,-49.2944078866059,
-25.));
#25420=CARTESIAN_POINT('Ctrl Pts',(-17.4539839348206,-49.3215020489175,
-25.));
#25421=CARTESIAN_POINT('Ctrl Pts',(-17.4437594637069,-49.3487770650009,
-25.));
#25422=CARTESIAN_POINT('Ctrl Pts',(-17.4339645308892,-49.3762213605602,
-25.));
#25423=CARTESIAN_POINT('Ctrl Pts',(-17.4287329400572,-49.3908796872388,
-25.));
#25424=CARTESIAN_POINT('Ctrl Pts',(-17.4236243316885,-49.4055852979435,
-25.));
#25425=CARTESIAN_POINT('Ctrl Pts',(-17.4186430808377,-49.4203242086228,
-25.));
#25426=CARTESIAN_POINT('Ctrl Pts',(-17.3890982615448,-49.5077437073873,
-25.));
#25427=CARTESIAN_POINT('Ctrl Pts',(-17.3639901618958,-49.5964439977786,
-25.));
#25428=CARTESIAN_POINT('Ctrl Pts',(-17.3433519062038,-49.6860276500902,
-25.));
#25429=CARTESIAN_POINT('Ctrl Pts',(-17.3223954629373,-49.7769924464998,
-25.));
#25430=CARTESIAN_POINT('Ctrl Pts',(-17.306047251885,-49.8688688586223,-25.));
#25431=CARTESIAN_POINT('Ctrl Pts',(-17.2943837746448,-49.9612739444462,
-25.));
#25432=CARTESIAN_POINT('Ctrl Pts',(-17.2828119061749,-50.0529532504608,
-25.));
#25433=CARTESIAN_POINT('Ctrl Pts',(-17.2758511252064,-50.1451538869544,
-25.));
#25434=CARTESIAN_POINT('Ctrl Pts',(-17.2736230843733,-50.2375210507824,
-25.));
#25435=CARTESIAN_POINT('Ctrl Pts',(-17.2725148765619,-50.283463661413,-25.));
#25436=CARTESIAN_POINT('Ctrl Pts',(-17.272578302097,-50.3294476832055,-25.));
#25437=CARTESIAN_POINT('Ctrl Pts',(-17.2738331202707,-50.375430153216,-25.));
#25438=CARTESIAN_POINT('Ctrl Pts',(-17.2742439451017,-50.3904847171926,
-25.));
#25439=CARTESIAN_POINT('Ctrl Pts',(-17.2747825691208,-50.4055406251206,
-25.));
#25440=CARTESIAN_POINT('Ctrl Pts',(-17.2754495535264,-50.4205916673977,
-25.));
#25441=CARTESIAN_POINT('Ctrl Pts',(-17.2796905507083,-50.516293197071,-25.));
#25442=CARTESIAN_POINT('Ctrl Pts',(-17.2891001105497,-50.6114301979472,
-25.));
#25443=CARTESIAN_POINT('Ctrl Pts',(-17.3037427186582,-50.7056047140635,
-25.));
#25444=CARTESIAN_POINT('Ctrl Pts',(-17.3078986693771,-50.7323338763174,
-25.));
#25445=CARTESIAN_POINT('Ctrl Pts',(-17.3124764735867,-50.758985634219,-25.));
#25446=CARTESIAN_POINT('Ctrl Pts',(-17.3174783250881,-50.7855511504669,
-25.));
#25447=CARTESIAN_POINT('Ctrl Pts',(-17.3344205238429,-50.8755334812447,
-25.));
#25448=CARTESIAN_POINT('Ctrl Pts',(-17.3562236803317,-50.9645262383779,
-25.));
#25449=CARTESIAN_POINT('Ctrl Pts',(-17.382584962494,-51.0522968717463,-25.));
#25450=CARTESIAN_POINT('Ctrl Pts',(-17.4095434902992,-51.1420560513483,
-25.));
#25451=CARTESIAN_POINT('Ctrl Pts',(-17.44126923195,-51.2305378030409,-25.));
#25452=CARTESIAN_POINT('Ctrl Pts',(-17.4774925519387,-51.3174897503804,
-25.));
#25453=CARTESIAN_POINT('Ctrl Pts',(-17.4899691547968,-51.3474391011035,
-25.));
#25454=CARTESIAN_POINT('Ctrl Pts',(-17.502979781103,-51.3772068812893,-25.));
#25455=CARTESIAN_POINT('Ctrl Pts',(-17.5165147798695,-51.4067824406253,
-25.));
#25456=CARTESIAN_POINT('Ctrl Pts',(-17.5231905157176,-51.4213697062096,
-25.));
#25457=CARTESIAN_POINT('Ctrl Pts',(-17.5299938239586,-51.4359102074969,
-25.));
#25458=CARTESIAN_POINT('Ctrl Pts',(-17.5369236053827,-51.4504026443194,
-25.));
#25459=CARTESIAN_POINT('Ctrl Pts',(-17.5430251409841,-51.46316294855,-25.));
#25460=CARTESIAN_POINT('Ctrl Pts',(-17.549223964339,-51.4758842663769,-25.));
#25461=CARTESIAN_POINT('Ctrl Pts',(-17.5555138729846,-51.488555244485,-25.));
#25462=CARTESIAN_POINT('Ctrl Pts',(-17.5983732491784,-51.5748951657893,
-25.));
#25463=CARTESIAN_POINT('Ctrl Pts',(-17.645521751679,-51.6590337918885,-25.));
#25464=CARTESIAN_POINT('Ctrl Pts',(-17.6966168151664,-51.7407208715959,
-25.));
#25465=CARTESIAN_POINT('Ctrl Pts',(-17.7487215795578,-51.8240221878382,
-25.));
#25466=CARTESIAN_POINT('Ctrl Pts',(-17.8049307394874,-51.9047748826328,
-25.));
#25467=CARTESIAN_POINT('Ctrl Pts',(-17.8649359851474,-51.9827064087797,
-25.));
#25468=CARTESIAN_POINT('Ctrl Pts',(-17.9254196422576,-52.061259269512,-25.));
#25469=CARTESIAN_POINT('Ctrl Pts',(-17.9897606186624,-52.1369466346382,
-25.));
#25470=CARTESIAN_POINT('Ctrl Pts',(-18.0576924116876,-52.2094699519837,
-25.));
#25471=CARTESIAN_POINT('Ctrl Pts',(-18.0946383138793,-52.2489130355524,
-25.));
#25472=CARTESIAN_POINT('Ctrl Pts',(-18.1326471623705,-52.2874198090281,
-25.));
#25473=CARTESIAN_POINT('Ctrl Pts',(-18.1716813643735,-52.3249384844083,
-25.));
#25474=CARTESIAN_POINT('Ctrl Pts',(-18.184337849379,-52.3371035736892,-25.));
#25475=CARTESIAN_POINT('Ctrl Pts',(-18.1971021587896,-52.3491647575441,
-25.));
#25476=CARTESIAN_POINT('Ctrl Pts',(-18.2099730859135,-52.3611201963401,
-25.));
#25477=CARTESIAN_POINT('Ctrl Pts',(-18.221458568745,-52.371788735266,-25.));
#25478=CARTESIAN_POINT('Ctrl Pts',(-18.2330235730151,-52.3823680223885,
-25.));
#25479=CARTESIAN_POINT('Ctrl Pts',(-18.2446616724208,-52.392852287093,-25.));
#25480=CARTESIAN_POINT('Ctrl Pts',(-18.320476523519,-52.4611506354522,-25.));
#25481=CARTESIAN_POINT('Ctrl Pts',(-18.3994575544252,-52.5254816235113,
-25.));
#25482=CARTESIAN_POINT('Ctrl Pts',(-18.4812783860139,-52.5855621951249,
-25.));
#25483=CARTESIAN_POINT('Ctrl Pts',(-18.563171620063,-52.6456959314536,-25.));
#25484=CARTESIAN_POINT('Ctrl Pts',(-18.6479102599513,-52.7015725637526,
-25.));
#25485=CARTESIAN_POINT('Ctrl Pts',(-18.7352120289865,-52.7528820895473,
-25.));
#25486=CARTESIAN_POINT('Ctrl Pts',(-18.8207515374939,-52.8031558888842,
-25.));
#25487=CARTESIAN_POINT('Ctrl Pts',(-18.9087524063426,-52.8490457775827,
-25.));
#25488=CARTESIAN_POINT('Ctrl Pts',(-18.9989828629694,-52.8902240100431,
-25.));
#25489=CARTESIAN_POINT('Ctrl Pts',(-19.0364028600903,-52.9073012741701,
-25.));
#25490=CARTESIAN_POINT('Ctrl Pts',(-19.0742066724074,-52.9235676922614,
-25.));
#25491=CARTESIAN_POINT('Ctrl Pts',(-19.1123791172294,-52.9389975882857,
-25.));
#25492=CARTESIAN_POINT('Ctrl Pts',(-19.1428008541822,-52.9512945276158,
-25.));
#25493=CARTESIAN_POINT('Ctrl Pts',(-19.1734567410254,-52.9630601291729,
-25.));
#25494=CARTESIAN_POINT('Ctrl Pts',(-19.2043345174297,-52.9742970828256,
-25.));
#25495=CARTESIAN_POINT('Ctrl Pts',(-20.7937992825329,-52.9692229537457,
-25.));
#25496=CARTESIAN_POINT('Ctrl Pts',(-20.8886442409227,-52.934528244297,-25.));
#25497=CARTESIAN_POINT('Ctrl Pts',(-20.981446133513,-52.8948452065297,-25.));
#25498=CARTESIAN_POINT('Ctrl Pts',(-21.0719638298413,-52.8504935643273,
-25.));
#25499=CARTESIAN_POINT('Ctrl Pts',(-21.1637466263856,-52.805522051377,-25.));
#25500=CARTESIAN_POINT('Ctrl Pts',(-21.2531815997536,-52.7557498214297,
-25.));
#25501=CARTESIAN_POINT('Ctrl Pts',(-21.3399833391246,-52.7014695233431,
-25.));
#25502=CARTESIAN_POINT('Ctrl Pts',(-21.3644995059587,-52.6861386687618,
-25.));
#25503=CARTESIAN_POINT('Ctrl Pts',(-21.3888053754925,-52.6704479886835,
-25.));
#25504=CARTESIAN_POINT('Ctrl Pts',(-21.4128939207048,-52.6544036208027,
-25.));
#25505=CARTESIAN_POINT('Ctrl Pts',(-21.4322113951179,-52.6415370627237,
-25.));
#25506=CARTESIAN_POINT('Ctrl Pts',(-21.4513911998519,-52.6284414304985,
-25.));
#25507=CARTESIAN_POINT('Ctrl Pts',(-21.4704104548933,-52.6151336299332,
-25.));
#25508=CARTESIAN_POINT('Ctrl Pts',(-21.5531190662063,-52.5572622936485,
-25.));
#25509=CARTESIAN_POINT('Ctrl Pts',(-21.6328730890496,-52.4953306936023,
-25.));
#25510=CARTESIAN_POINT('Ctrl Pts',(-21.7094060419017,-52.429635446766,-25.));
#25511=CARTESIAN_POINT('Ctrl Pts',(-21.7684006977073,-52.3789949274767,
-25.));
#25512=CARTESIAN_POINT('Ctrl Pts',(-21.825480777475,-52.3261171605589,-25.));
#25513=CARTESIAN_POINT('Ctrl Pts',(-21.8805066584147,-52.2711262352939,
-25.));
#25514=CARTESIAN_POINT('Ctrl Pts',(-21.9097989368823,-52.2418525650037,
-25.));
#25515=CARTESIAN_POINT('Ctrl Pts',(-21.9385088158922,-52.2119799147563,
-25.));
#25516=CARTESIAN_POINT('Ctrl Pts',(-21.9666132103813,-52.1815261718079,
-25.));
#25517=CARTESIAN_POINT('Ctrl Pts',(-21.9762498256991,-52.1710839967989,
-25.));
#25518=CARTESIAN_POINT('Ctrl Pts',(-21.9858145141289,-52.1605742164994,
-25.));
#25519=CARTESIAN_POINT('Ctrl Pts',(-21.995299714842,-52.150005155917,-25.));
#25520=CARTESIAN_POINT('Ctrl Pts',(-22.0610979628759,-52.0766882393088,
-25.));
#25521=CARTESIAN_POINT('Ctrl Pts',(-22.1231641141855,-52.000424838082,-25.));
#25522=CARTESIAN_POINT('Ctrl Pts',(-22.1812542925625,-51.9214927964729,
-25.));
#25523=CARTESIAN_POINT('Ctrl Pts',(-22.2388180795722,-51.8432760073639,
-25.));
#25524=CARTESIAN_POINT('Ctrl Pts',(-22.2924780587685,-51.7624379398908,
-25.));
#25525=CARTESIAN_POINT('Ctrl Pts',(-22.3419511803801,-51.6792265585039,
-25.));
#25526=CARTESIAN_POINT('Ctrl Pts',(-22.3900085390461,-51.5983964214488,
-25.));
#25527=CARTESIAN_POINT('Ctrl Pts',(-22.434115448639,-51.5153261622487,-25.));
#25528=CARTESIAN_POINT('Ctrl Pts',(-22.4739646868754,-51.4302327126893,
-25.));
#25529=CARTESIAN_POINT('Ctrl Pts',(-22.4947697706581,-51.3858058572261,
-25.));
#25530=CARTESIAN_POINT('Ctrl Pts',(-22.5144134671897,-51.3408274043328,
-25.));
#25531=CARTESIAN_POINT('Ctrl Pts',(-22.5328463597941,-51.2953279864297,
-25.));
#25532=CARTESIAN_POINT('Ctrl Pts',(-22.5399054107244,-51.2779035530991,
-25.));
#25533=CARTESIAN_POINT('Ctrl Pts',(-22.5467868448816,-51.2604027172689,
-25.));
#25534=CARTESIAN_POINT('Ctrl Pts',(-22.5534877247282,-51.242827207983,-25.));
#25535=CARTESIAN_POINT('Ctrl Pts',(-22.5587291589222,-51.22907962894,-25.));
#25536=CARTESIAN_POINT('Ctrl Pts',(-22.563860220659,-51.2152858632226,-25.));
#25537=CARTESIAN_POINT('Ctrl Pts',(-22.5688743760763,-51.2014614459675,
-25.));
#25538=CARTESIAN_POINT('Ctrl Pts',(-22.6005568065216,-51.1141105161159,
-25.));
#25539=CARTESIAN_POINT('Ctrl Pts',(-22.6276304308536,-51.0253962670702,
-25.));
#25540=CARTESIAN_POINT('Ctrl Pts',(-22.6498439278908,-50.9355415828215,
-25.));
#25541=CARTESIAN_POINT('Ctrl Pts',(-22.6548287984448,-50.9153775371108,
-25.));
#25542=CARTESIAN_POINT('Ctrl Pts',(-22.659568716376,-50.8951560208944,-25.));
#25543=CARTESIAN_POINT('Ctrl Pts',(-22.6640604805451,-50.8748794971407,
-25.));
#25544=CARTESIAN_POINT('Ctrl Pts',(-22.6844253433926,-50.7829493312365,
-25.));
#25545=CARTESIAN_POINT('Ctrl Pts',(-22.6996934291485,-50.6898881391101,
-25.));
#25546=CARTESIAN_POINT('Ctrl Pts',(-22.709974675792,-50.5960881004475,-25.));
#25547=CARTESIAN_POINT('Ctrl Pts',(-22.7207065967185,-50.4981763750765,
-25.));
#25548=CARTESIAN_POINT('Ctrl Pts',(-22.726004891523,-50.3994583705262,-25.));
#25549=CARTESIAN_POINT('Ctrl Pts',(-22.7259371354055,-50.3003947692319,
-25.));
#25550=CARTESIAN_POINT('Ctrl Pts',(-22.7259106318212,-50.2616449026909,
-25.));
#25551=CARTESIAN_POINT('Ctrl Pts',(-22.7250624840214,-50.2228424140868,
-25.));
#25552=CARTESIAN_POINT('Ctrl Pts',(-22.7233945124232,-50.1840161029993,
-25.));
#25553=CARTESIAN_POINT('Ctrl Pts',(-22.7228610952776,-50.1715994527069,
-25.));
#25554=CARTESIAN_POINT('Ctrl Pts',(-22.7222438367581,-50.1591816778759,
-25.));
#25555=CARTESIAN_POINT('Ctrl Pts',(-22.7215434984435,-50.146773388563,-25.));
#25556=CARTESIAN_POINT('Ctrl Pts',(-22.7163011580038,-50.0538918832931,
-25.));
#25557=CARTESIAN_POINT('Ctrl Pts',(-22.706402037016,-49.9613918757547,-25.));
#25558=CARTESIAN_POINT('Ctrl Pts',(-22.6919697095793,-49.8696455402477,
-25.));
#25559=CARTESIAN_POINT('Ctrl Pts',(-22.6775715875303,-49.7781166484613,
-25.));
#25560=CARTESIAN_POINT('Ctrl Pts',(-22.6586613112021,-49.6873369139881,
-25.));
#25561=CARTESIAN_POINT('Ctrl Pts',(-22.6353129020366,-49.5976928152581,
-25.));
#25562=CARTESIAN_POINT('Ctrl Pts',(-22.6123616860385,-49.5095737036597,
-25.));
#25563=CARTESIAN_POINT('Ctrl Pts',(-22.5851215841949,-49.4225511325324,
-25.));
#25564=CARTESIAN_POINT('Ctrl Pts',(-22.5536224723794,-49.3370212909107,
-25.));
#25565=CARTESIAN_POINT('Ctrl Pts',(-22.5377791669639,-49.2940018111589,
-25.));
#25566=CARTESIAN_POINT('Ctrl Pts',(-22.5208577966156,-49.251360504603,-25.));
#25567=CARTESIAN_POINT('Ctrl Pts',(-22.5028587458779,-49.2091515771324,
-25.));
#25568=CARTESIAN_POINT('Ctrl Pts',(-22.4972963310614,-49.1961073579137,
-25.));
#25569=CARTESIAN_POINT('Ctrl Pts',(-22.4916309765552,-49.1831044539104,
-25.));
#25570=CARTESIAN_POINT('Ctrl Pts',(-22.4858626529295,-49.1701445225163,
-25.));
#25571=CARTESIAN_POINT('Ctrl Pts',(-22.4801786597127,-49.1573740597418,
-25.));
#25572=CARTESIAN_POINT('Ctrl Pts',(-22.4743981571289,-49.1446531657103,
-25.));
#25573=CARTESIAN_POINT('Ctrl Pts',(-22.4685229605677,-49.1319863864487,
-25.));
#25574=CARTESIAN_POINT('Ctrl Pts',(-22.4310411834156,-49.0511765969249,
-25.));
#25575=CARTESIAN_POINT('Ctrl Pts',(-22.389689647437,-48.9725239641082,-25.));
#25576=CARTESIAN_POINT('Ctrl Pts',(-22.344538126016,-48.89637657445,-25.));
#25577=CARTESIAN_POINT('Ctrl Pts',(-22.3001458379325,-48.8215096208652,
-25.));
#25578=CARTESIAN_POINT('Ctrl Pts',(-22.2520798308501,-48.7490636963479,
-25.));
#25579=CARTESIAN_POINT('Ctrl Pts',(-22.2003702171762,-48.6794038046902,
-25.));
#25580=CARTESIAN_POINT('Ctrl Pts',(-22.150240791408,-48.6118726413384,-25.));
#25581=CARTESIAN_POINT('Ctrl Pts',(-22.0966866025685,-48.5469593952847,
-25.));
#25582=CARTESIAN_POINT('Ctrl Pts',(-22.039707393449,-48.4850369103578,-25.));
#25583=CARTESIAN_POINT('Ctrl Pts',(-22.018724090908,-48.4622331850097,-25.));
#25584=CARTESIAN_POINT('Ctrl Pts',(-21.9972760520149,-48.439835493521,-25.));
#25585=CARTESIAN_POINT('Ctrl Pts',(-21.9753624510336,-48.4178640718566,
-25.));
#25586=CARTESIAN_POINT('Ctrl Pts',(-21.9562845909508,-48.3987358734061,
-25.));
#25587=CARTESIAN_POINT('Ctrl Pts',(-21.9368538444216,-48.3799307827435,
-25.));
#25588=CARTESIAN_POINT('Ctrl Pts',(-21.9170803467229,-48.3614539181488,
-25.));
#25589=CARTESIAN_POINT('Origin',(-20.,-50.,-42.2084234471774));
#25590=CARTESIAN_POINT('Ctrl Pts',(-16.9232551256392,-49.9980895495447,
-39.7084234471775));
#25591=CARTESIAN_POINT('Ctrl Pts',(-16.9223299842891,-49.8748204265296,
-39.7020198504182));
#25592=CARTESIAN_POINT('Ctrl Pts',(-16.9848355034282,-48.7389612450556,
-39.6429667459281));
#25593=CARTESIAN_POINT('Ctrl Pts',(-18.3975850141438,-46.7464741122942,
-39.5312641337071));
#25594=CARTESIAN_POINT('Ctrl Pts',(-21.8481508174258,-46.8799262317611,
-39.3733156105146));
#25595=CARTESIAN_POINT('Ctrl Pts',(-23.623022297825,-49.8417650665615,-39.2153670873222));
#25596=CARTESIAN_POINT('Ctrl Pts',(-22.1130258164637,-52.9473164300811,
-39.0574185641297));
#25597=CARTESIAN_POINT('Ctrl Pts',(-18.6872049726298,-53.380502213004,-38.8994700409372));
#25598=CARTESIAN_POINT('Ctrl Pts',(-17.0406886962336,-51.4421741378802,
-38.7831383352865));
#25599=CARTESIAN_POINT('Ctrl Pts',(-16.923813258856,-50.2155563656135,-38.7194561373666));
#25600=CARTESIAN_POINT('Ctrl Pts',(-16.9257450511401,-50.0026845218917,
-38.7084234471775));
#25601=CARTESIAN_POINT('Ctrl Pts',(-16.9296932342852,-50.0033456701988,
-39.7915765528225));
#25602=CARTESIAN_POINT('Ctrl Pts',(-16.93470303559,-49.3102257217221,-39.7557520197534));
#25603=CARTESIAN_POINT('Ctrl Pts',(-17.5071826427202,-47.5885966321291,
-39.6672779789534));
#25604=CARTESIAN_POINT('Ctrl Pts',(-20.3515248249563,-46.3913860864081,
-39.5261544304226));
#25605=CARTESIAN_POINT('Ctrl Pts',(-23.2138549612499,-48.3201943023511,
-39.3682059072301));
#25606=CARTESIAN_POINT('Ctrl Pts',(-23.1634850140729,-51.7735630043146,
-39.2102573840376));
#25607=CARTESIAN_POINT('Ctrl Pts',(-20.2442744821096,-53.6181272821323,
-39.0523088608452));
#25608=CARTESIAN_POINT('Ctrl Pts',(-17.469492581831,-52.3497510624684,-38.9127485837735));
#25609=CARTESIAN_POINT('Ctrl Pts',(-16.9339707214102,-50.6610395236483,
-38.8258378144326));
#25610=CARTESIAN_POINT('Ctrl Pts',(-16.9296186885438,-49.9978504047438,
-38.7915765528226));
#25611=CARTESIAN_POINT('Ctrl Pts',(-21.913465996665,-48.364012796625,-40.));
#25612=CARTESIAN_POINT('Ctrl Pts',(-22.4546613829867,-48.9970000028465,
-39.9473504922692));
#25613=CARTESIAN_POINT('Ctrl Pts',(-22.8504302036551,-50.831572053257,-39.8420514768075));
#25614=CARTESIAN_POINT('Ctrl Pts',(-20.8590118257495,-52.8453303030972,
-39.6841029536151));
#25615=CARTESIAN_POINT('Ctrl Pts',(-18.0884180617819,-52.2727938259679,
-39.5261544304226));
#25616=CARTESIAN_POINT('Ctrl Pts',(-17.0511987917854,-49.6427658750915,
-39.3682059072301));
#25617=CARTESIAN_POINT('Ctrl Pts',(-18.6874638923401,-47.3350410208884,
-39.2102573840377));
#25618=CARTESIAN_POINT('Ctrl Pts',(-21.5138180194792,-47.4443514847759,
-39.0523088608452));
#25619=CARTESIAN_POINT('Ctrl Pts',(-22.9676130257929,-49.8703899642324,
-38.8943603376527));
#25620=CARTESIAN_POINT('Ctrl Pts',(-21.7307767993972,-52.4141431959425,
-38.7364118144602));
#25621=CARTESIAN_POINT('Ctrl Pts',(-18.9246912375453,-52.7689651281072,
-38.5784632912678));
#25622=CARTESIAN_POINT('Ctrl Pts',(-17.0935587667564,-50.6133013619587,
-38.4205147680753));
#25623=CARTESIAN_POINT('Ctrl Pts',(-17.8976064891825,-47.9015504057097,
-38.2625662448829));
#25624=CARTESIAN_POINT('Ctrl Pts',(-20.6078313089819,-47.09241268106,-38.1046177216904));
#25625=CARTESIAN_POINT('Ctrl Pts',(-22.7669535441375,-48.9194895166619,
-37.9466691984979));
#25626=CARTESIAN_POINT('Ctrl Pts',(-22.4173633664285,-51.726235575411,-37.7887206753054));
#25627=CARTESIAN_POINT('Ctrl Pts',(-19.876023238429,-52.9678547167293,-37.630772152113));
#25628=CARTESIAN_POINT('Ctrl Pts',(-17.4470891231681,-51.5186110643773,
-37.4728236289205));
#25629=CARTESIAN_POINT('Ctrl Pts',(-17.3328016297339,-48.6924885372187,
-37.314875105728));
#25630=CARTESIAN_POINT('Ctrl Pts',(-19.6367817929697,-47.0518470927161,
-37.1569265825355));
#25631=CARTESIAN_POINT('Ctrl Pts',(-22.2700808509466,-48.0842061220133,
-36.9989780593431));
#25632=CARTESIAN_POINT('Ctrl Pts',(-22.845166646169,-50.8535572460832,-36.8410295361506));
#25633=CARTESIAN_POINT('Ctrl Pts',(-20.840626373429,-52.8490139488643,-36.6830810129582));
#25634=CARTESIAN_POINT('Ctrl Pts',(-18.0739157352567,-52.2613563661284,
-36.5251324897657));
#25635=CARTESIAN_POINT('Ctrl Pts',(-17.0535271202902,-49.6233957357017,
-36.3671839665733));
#25636=CARTESIAN_POINT('Ctrl Pts',(-18.7046158526517,-47.3268907411116,
-36.2092354433807));
#25637=CARTESIAN_POINT('Ctrl Pts',(-21.530189993977,-47.454012610956,-36.0512869201883));
#25638=CARTESIAN_POINT('Ctrl Pts',(-22.9683874064431,-49.8895038145725,
-35.8933383969959));
#25639=CARTESIAN_POINT('Ctrl Pts',(-21.7152382368816,-52.4251785485085,
-35.7353898738033));
#25640=CARTESIAN_POINT('Ctrl Pts',(-18.9069347245663,-52.7620176511933,
-35.5774413506109));
#25641=CARTESIAN_POINT('Ctrl Pts',(-17.0896802534022,-50.5946193524052,
-35.4194928274184));
#25642=CARTESIAN_POINT('Ctrl Pts',(-17.9111241831078,-47.8880977713745,
-35.261544304226));
#25643=CARTESIAN_POINT('Ctrl Pts',(-20.6264882857017,-47.096373710409,-35.1035957810335));
#25644=CARTESIAN_POINT('Ctrl Pts',(-22.7738345134306,-48.9372792964274,
-34.945647257841));
#25645=CARTESIAN_POINT('Ctrl Pts',(-22.4062293501948,-51.7417214231792,
-34.7876987346485));
#25646=CARTESIAN_POINT('Ctrl Pts',(-19.8569692172952,-52.9669977076003,
-34.6297502114561));
#25647=CARTESIAN_POINT('Ctrl Pts',(-17.4373907449893,-51.5021874076948,
-34.4718016882636));
#25648=CARTESIAN_POINT('Ctrl Pts',(-17.3412521459643,-48.675389472198,-34.3138531650712));
#25649=CARTESIAN_POINT('Ctrl Pts',(-19.6557193640327,-47.0495756160508,
-34.1559046418787));
#25650=CARTESIAN_POINT('Ctrl Pts',(-22.2823353639105,-48.0988218157291,
-33.9979561186862));
#25651=CARTESIAN_POINT('Ctrl Pts',(-22.839627303423,-50.8718084533652,-33.8400075954937));
#25652=CARTESIAN_POINT('Ctrl Pts',(-20.8223155302823,-52.8543528811905,
-33.6820590723013));
#25653=CARTESIAN_POINT('Ctrl Pts',(-18.059435275431,-52.2489423628591,-33.5241105491088));
#25654=CARTESIAN_POINT('Ctrl Pts',(-17.0560060367383,-49.6044842026135,
-33.3661620259163));
#25655=CARTESIAN_POINT('Ctrl Pts',(-18.7218065870059,-47.318628186789,-33.2082135027239));
#25656=CARTESIAN_POINT('Ctrl Pts',(-21.54650623034,-47.4638904437655,-33.0502649795314));
#25657=CARTESIAN_POINT('Ctrl Pts',(-22.9690357094856,-49.9085661030944,
-32.8923164563389));
#25658=CARTESIAN_POINT('Ctrl Pts',(-21.6996308099799,-52.4361420959114,
-32.7343679331465));
#25659=CARTESIAN_POINT('Ctrl Pts',(-18.8892223469998,-52.754942142278,-32.576419409954));
#25660=CARTESIAN_POINT('Ctrl Pts',(-17.0859221992198,-50.575919936019,-32.4184708867615));
#25661=CARTESIAN_POINT('Ctrl Pts',(-17.9247277657372,-47.8747286395846,
-32.260522363569));
#25662=CARTESIAN_POINT('Ctrl Pts',(-20.6451195505088,-47.1004562484323,
-32.1025738403766));
#25663=CARTESIAN_POINT('Ctrl Pts',(-22.7806010592582,-48.9551119911895,
-31.9446253171841));
#25664=CARTESIAN_POINT('Ctrl Pts',(-22.3949961557367,-51.757135912703,-31.7866767939917));
#25665=CARTESIAN_POINT('Ctrl Pts',(-19.8379210783241,-52.9660181430417,
-31.6287282707992));
#25666=CARTESIAN_POINT('Ctrl Pts',(-17.4277980297875,-51.4857019304486,
-31.4707797476067));
#25667=CARTESIAN_POINT('Ctrl Pts',(-17.3498122776559,-48.6583449630995,
-31.3128312244143));
#25668=CARTESIAN_POINT('Ctrl Pts',(-19.6746711315577,-47.0474258131146,
-31.1548827012217));
#25669=CARTESIAN_POINT('Ctrl Pts',(-22.2944957760458,-48.1135158798941,
-30.9969341780293));
#25670=CARTESIAN_POINT('Ctrl Pts',(-22.8339708843277,-50.8900237235527,
-30.8389856548368));
#25671=CARTESIAN_POINT('Ctrl Pts',(-20.803970783118,-52.8595741259139,-30.6810371316444));
#25672=CARTESIAN_POINT('Ctrl Pts',(-18.0450348245211,-52.2364356383248,
-30.5230886084519));
#25673=CARTESIAN_POINT('Ctrl Pts',(-17.058606332953,-49.5855889755817,-30.3651400852594));
#25674=CARTESIAN_POINT('Ctrl Pts',(-18.7390500208516,-47.3104761849374,
-30.207191562067));
#25675=CARTESIAN_POINT('Ctrl Pts',(-21.5627587047845,-47.4738728392405,
-30.0492430388745));
#25676=CARTESIAN_POINT('Ctrl Pts',(-22.9695616002458,-49.9276321615209,
-29.891294515682));
#25677=CARTESIAN_POINT('Ctrl Pts',(-21.6839533078998,-52.4470052019794,
-29.7333459924896));
#25678=CARTESIAN_POINT('Ctrl Pts',(-18.8715557664016,-52.7477530481074,
-29.5753974692971));
#25679=CARTESIAN_POINT('Ctrl Pts',(-17.0822842914354,-50.5571967746374,
-29.4174489461046));
#25680=CARTESIAN_POINT('Ctrl Pts',(-17.9384169110962,-47.8614471319982,
-29.2595004229121));
#25681=CARTESIAN_POINT('Ctrl Pts',(-20.6637242172836,-47.1046583335895,
-29.1015518997197));
#25682=CARTESIAN_POINT('Ctrl Pts',(-22.7872529618541,-48.9729877663616,
-28.9436033765272));
#25683=CARTESIAN_POINT('Ctrl Pts',(-22.3836642165086,-51.7724779560436,
-28.7856548533348));
#25684=CARTESIAN_POINT('Ctrl Pts',(-19.8188796216655,-52.9649162907898,
-28.6277063301422));
#25685=CARTESIAN_POINT('Ctrl Pts',(-17.4183113658474,-51.469155197875,-28.4697578069498));
#25686=CARTESIAN_POINT('Ctrl Pts',(-17.3584816750768,-48.641355770686,-28.3118092837573));
#25687=CARTESIAN_POINT('Ctrl Pts',(-19.6936363134129,-47.0453977423244,
-28.1538607605649));
#25688=CARTESIAN_POINT('Ctrl Pts',(-22.3065615846713,-48.1282877259989,
-27.9959122373724));
#25689=CARTESIAN_POINT('Ctrl Pts',(-22.8281976261233,-50.9082022926661,
-27.8379637141799));
#25690=CARTESIAN_POINT('Ctrl Pts',(-20.7855928795529,-52.8646774827825,
-27.6800151909875));
#25691=CARTESIAN_POINT('Ctrl Pts',(-18.0307149939936,-52.2238366836986,
-27.522066667795));
#25692=CARTESIAN_POINT('Ctrl Pts',(-17.0613278662217,-49.5667108796552,
-27.3641181446025));
#25693=CARTESIAN_POINT('Ctrl Pts',(-18.7563455140292,-47.3024349814285,
-27.2061696214101));
#25694=CARTESIAN_POINT('Ctrl Pts',(-21.5789466062486,-47.4839595647848,
-27.0482210982176));
#25695=CARTESIAN_POINT('Ctrl Pts',(-22.9699653377665,-49.9467008477527,
-26.8902725750251));
#25696=CARTESIAN_POINT('Ctrl Pts',(-21.6682058180543,-52.457768127515,-26.7323240518326));
#25697=CARTESIAN_POINT('Ctrl Pts',(-18.8539368241228,-52.7404492541073,
-26.5743755286402));
#25698=CARTESIAN_POINT('Ctrl Pts',(-17.078764464007,-50.5384534495725,-26.4164270054477));
#25699=CARTESIAN_POINT('Ctrl Pts',(-17.9521954671408,-47.8482482024917,
-26.2584784822553));
#25700=CARTESIAN_POINT('Ctrl Pts',(-20.682292733498,-47.1089909302976,-26.1005299590627));
#25701=CARTESIAN_POINT('Ctrl Pts',(-22.7938074397502,-48.990883708662,-25.9425814358704));
#25702=CARTESIAN_POINT('Ctrl Pts',(-22.3721991697247,-51.7877910759886,
-25.7846329126778));
#25703=CARTESIAN_POINT('Ctrl Pts',(-19.7999149827311,-52.9636042777895,
-25.6266843894854));
#25704=CARTESIAN_POINT('Ctrl Pts',(-17.4087930587084,-51.4527229542004,
-25.4687358662929));
#25705=CARTESIAN_POINT('Ctrl Pts',(-17.3675349459595,-48.6240739391879,
-25.3107873431004));
#25706=CARTESIAN_POINT('Ctrl Pts',(-19.7120663609263,-47.0441868290824,
-25.152838819908));
#25707=CARTESIAN_POINT('Ctrl Pts',(-22.3196265018743,-48.1417377089596,
-24.9948902967155));
#25708=CARTESIAN_POINT('Ctrl Pts',(-22.8200820083521,-50.9293018303199,
-24.836941773523));
#25709=CARTESIAN_POINT('Ctrl Pts',(-21.4547503964622,-52.2169963426693,
-24.7316427580614));
#25710=CARTESIAN_POINT('Ctrl Pts',(-20.6501999979751,-52.4320868020351,
-24.6789932503306));
#25711=CARTESIAN_POINT('Ctrl Pts',(-22.0543315503421,-48.2435746787731,
-40.1070022498898));
#25712=CARTESIAN_POINT('Ctrl Pts',(-22.6353686625551,-48.9231611417519,
-40.054352742159));
#25713=CARTESIAN_POINT('Ctrl Pts',(-23.0602731951456,-50.8927907307295,
-39.9490537266973));
#25714=CARTESIAN_POINT('Ctrl Pts',(-20.9222505645932,-53.0547978500713,
-39.7911052035049));
#25715=CARTESIAN_POINT('Ctrl Pts',(-17.9476912087333,-52.4401123783993,
-39.6331566803124));
#25716=CARTESIAN_POINT('Ctrl Pts',(-16.8341139229649,-49.6164670106824,
-39.4752081571199));
#25717=CARTESIAN_POINT('Ctrl Pts',(-18.590837599608,-47.138852051357,-39.3172596339275));
#25718=CARTESIAN_POINT('Ctrl Pts',(-21.6252622854614,-47.2562097337709,
-39.159311110735));
#25719=CARTESIAN_POINT('Ctrl Pts',(-23.1860827831369,-49.8608483316754,
-39.0013625875425));
#25720=CARTESIAN_POINT('Ctrl Pts',(-21.8581931384194,-52.5918676073221,
-38.84341406435));
#25721=CARTESIAN_POINT('Ctrl Pts',(-18.8455291492401,-52.9728108230729,
-38.6854655411576));
#25722=CARTESIAN_POINT('Ctrl Pts',(-16.8795923548817,-50.6584513860896,
-38.5275170179651));
#25723=CARTESIAN_POINT('Ctrl Pts',(-17.7428324683928,-47.7470667281956,
-38.3695684947727));
#25724=CARTESIAN_POINT('Ctrl Pts',(-20.652578638713,-46.8783618966402,-38.2116199715802));
#25725=CARTESIAN_POINT('Ctrl Pts',(-22.9706511502998,-48.8399444880308,
-38.0536714483877));
#25726=CARTESIAN_POINT('Ctrl Pts',(-22.5953248403423,-51.8533175985726,
-37.8957229251952));
#25727=CARTESIAN_POINT('Ctrl Pts',(-19.8668963162929,-53.1863422668785,
-37.7377744020028));
#25728=CARTESIAN_POINT('Ctrl Pts',(-17.2591489116463,-51.6304081847737,
-37.5798258788103));
#25729=CARTESIAN_POINT('Ctrl Pts',(-17.1364478006882,-48.5962321488299,
-37.4218773556179));
#25730=CARTESIAN_POINT('Ctrl Pts',(-19.6100423923594,-46.8348099505181,
-37.2639288324254));
#25731=CARTESIAN_POINT('Ctrl Pts',(-22.4371996795631,-47.9431691943522,
-37.1059803092329));
#25732=CARTESIAN_POINT('Ctrl Pts',(-23.0546221450462,-50.9163944296412,
-36.9480317860405));
#25733=CARTESIAN_POINT('Ctrl Pts',(-20.9025116119098,-53.0587526784993,
-36.790083262848));
#25734=CARTESIAN_POINT('Ctrl Pts',(-17.9321212498284,-52.427832915558,-36.6321347396555));
#25735=CARTESIAN_POINT('Ctrl Pts',(-16.8366136583745,-49.5956708802301,
-36.474186216463));
#25736=CARTESIAN_POINT('Ctrl Pts',(-18.6092522530588,-47.1301017642242,
-36.3162376932706));
#25737=CARTESIAN_POINT('Ctrl Pts',(-21.6428395320971,-47.2665820928086,
-36.1582891700781));
#25738=CARTESIAN_POINT('Ctrl Pts',(-23.1869141721474,-49.881369305589,-36.0003406468857));
#25739=CARTESIAN_POINT('Ctrl Pts',(-21.8415106578954,-52.6037153605536,
-35.8423921236932));
#25740=CARTESIAN_POINT('Ctrl Pts',(-18.8264654371594,-52.9653518867529,
-35.6844436005007));
#25741=CARTESIAN_POINT('Ctrl Pts',(-16.8754283131031,-50.6383940442208,
-35.5264950773082));
#25742=CARTESIAN_POINT('Ctrl Pts',(-17.7573453080079,-47.7326237377279,
-35.3685465541157));
#25743=CARTESIAN_POINT('Ctrl Pts',(-20.6726091048808,-46.8826145290767,
-35.2105980309233));
#25744=CARTESIAN_POINT('Ctrl Pts',(-22.9780386828404,-48.8590439159327,
-35.0526495077308));
#25745=CARTESIAN_POINT('Ctrl Pts',(-22.5833711600205,-51.8699434835947,
-34.8947009845384));
#25746=CARTESIAN_POINT('Ctrl Pts',(-19.8464395760924,-53.1854221664451,
-34.7367524613459));
#25747=CARTESIAN_POINT('Ctrl Pts',(-17.248736558192,-51.6127754512139,-34.5788039381534));
#25748=CARTESIAN_POINT('Ctrl Pts',(-17.1455204270839,-48.577874284716,-34.4208554149609));
#25749=CARTESIAN_POINT('Ctrl Pts',(-19.6303741096669,-46.8323712522672,
-34.2629068917685));
#25750=CARTESIAN_POINT('Ctrl Pts',(-22.4503563453516,-47.9588608663144,
-34.104958368576));
#25751=CARTESIAN_POINT('Ctrl Pts',(-23.0486750069255,-50.9359892544338,
-33.9470098453836));
#25752=CARTESIAN_POINT('Ctrl Pts',(-20.882852760979,-53.0644846523845,-33.789061322191));
#25753=CARTESIAN_POINT('Ctrl Pts',(-17.9165747674058,-52.4145050181057,
-33.6311127989986));
#25754=CARTESIAN_POINT('Ctrl Pts',(-16.8392750677116,-49.5753671177612,
-33.4731642758062));
#25755=CARTESIAN_POINT('Ctrl Pts',(-18.6277085350199,-47.1212309371173,
-33.3152157526137));
#25756=CARTESIAN_POINT('Ctrl Pts',(-21.6603569372674,-47.2771871119858,
-33.1572672294212));
#25757=CARTESIAN_POINT('Ctrl Pts',(-23.1876102019681,-49.9018349218062,
-32.9993187062287));
#25758=CARTESIAN_POINT('Ctrl Pts',(-21.8247542433263,-52.615486022469,-32.8413701830363));
#25759=CARTESIAN_POINT('Ctrl Pts',(-18.8074491096521,-52.9577554929707,
-32.6834216598438));
#25760=CARTESIAN_POINT('Ctrl Pts',(-16.8713935984606,-50.6183180140628,
-32.5254731366514));
#25761=CARTESIAN_POINT('Ctrl Pts',(-17.7719503592824,-47.7182703970965,
-32.3675246134588));
#25762=CARTESIAN_POINT('Ctrl Pts',(-20.6926119662761,-46.8869976154139,
-32.2095760902664));
#25763=CARTESIAN_POINT('Ctrl Pts',(-22.9853033682881,-48.8781894181476,
-32.0516275670739));
#25764=CARTESIAN_POINT('Ctrl Pts',(-22.5713110001709,-51.8864927571205,
-31.8936790438815));
#25765=CARTESIAN_POINT('Ctrl Pts',(-19.8259891510878,-53.1843704882957,
-31.735730520689));
#25766=CARTESIAN_POINT('Ctrl Pts',(-17.2384376464126,-51.5950763459838,
-31.5777819974965));
#25767=CARTESIAN_POINT('Ctrl Pts',(-17.1547107386128,-48.5595749928225,
-31.4198334743041));
#25768=CARTESIAN_POINT('Ctrl Pts',(-19.6507210685515,-46.8300631851227,
-31.2618849511116));
#25769=CARTESIAN_POINT('Ctrl Pts',(-22.4634119827961,-47.9746366782021,
-31.1039364279191));
#25770=CARTESIAN_POINT('Ctrl Pts',(-23.0426021735282,-50.9555454965146,
-30.9459879047266));
#25771=CARTESIAN_POINT('Ctrl Pts',(-20.8631575100844,-53.07009027474,-30.7880393815342));
#25772=CARTESIAN_POINT('Ctrl Pts',(-17.901114183996,-52.4010775734335,-30.6300908583417));
#25773=CARTESIAN_POINT('Ctrl Pts',(-16.8420667925521,-49.5550808617682,
-30.4721423351492));
#25774=CARTESIAN_POINT('Ctrl Pts',(-18.6462213961039,-47.112478801134,-30.3141938119568));
#25775=CARTESIAN_POINT('Ctrl Pts',(-21.6778058864939,-47.2879043915235,
-30.1562452887643));
#25776=CARTESIAN_POINT('Ctrl Pts',(-23.1881748077581,-49.9223045854607,
-29.9982967655718));
#25777=CARTESIAN_POINT('Ctrl Pts',(-21.8079225947839,-52.6271488487587,
-29.8403482423794));
#25778=CARTESIAN_POINT('Ctrl Pts',(-18.7884819505949,-52.9500371520131,
-29.6823997191869));
#25779=CARTESIAN_POINT('Ctrl Pts',(-16.8674878751545,-50.5982164908504,
-29.5244511959945));
#25780=CARTESIAN_POINT('Ctrl Pts',(-17.7866472722441,-47.704011131388,-29.366502672802));
#25781=CARTESIAN_POINT('Ctrl Pts',(-20.7125862715451,-46.8915090497067,
-29.2085541496095));
#25782=CARTESIAN_POINT('Ctrl Pts',(-22.9924449706976,-48.8973811722666,
-29.0506056264171));
#25783=CARTESIAN_POINT('Ctrl Pts',(-22.5591448261582,-51.9029642511193,
-28.8926571032245));
#25784=CARTESIAN_POINT('Ctrl Pts',(-19.8055459003343,-53.1831875198767,
-28.7347085800321));
#25785=CARTESIAN_POINT('Ctrl Pts',(-17.2282525931775,-51.5773114759311,
-28.5767600568396));
#25786=CARTESIAN_POINT('Ctrl Pts',(-17.1640183597962,-48.5413350899183,
-28.4188115336472));
#25787=CARTESIAN_POINT('Ctrl Pts',(-19.6710824293027,-46.8278858118023,
-28.2608630104547));
#25788=CARTESIAN_POINT('Ctrl Pts',(-22.4763660522088,-47.990495998181,-28.1029144872622));
#25789=CARTESIAN_POINT('Ctrl Pts',(-23.0364038995592,-50.9750623356614,
-27.9449659640698));
#25790=CARTESIAN_POINT('Ctrl Pts',(-20.8434266618807,-53.0755693305717,
-27.7870174408773));
#25791=CARTESIAN_POINT('Ctrl Pts',(-17.8857401560804,-52.3875511088739,
-27.6290689176848));
#25792=CARTESIAN_POINT('Ctrl Pts',(-16.8449886796767,-49.5348129980383,
-27.4711203944923));
#25793=CARTESIAN_POINT('Ctrl Pts',(-18.6647901490243,-47.1038456202467,
-27.3131718712999));
#25794=CARTESIAN_POINT('Ctrl Pts',(-21.6951855090058,-47.2987336817025,
-27.1552233481074));
#25795=CARTESIAN_POINT('Ctrl Pts',(-23.1886082676306,-49.9427770703744,
-26.9972748249149));
#25796=CARTESIAN_POINT('Ctrl Pts',(-21.7910158061163,-52.6387041194248,
-26.8393263017225));
#25797=CARTESIAN_POINT('Ctrl Pts',(-18.769565936895,-52.9421956672531,-26.68137777853));
#25798=CARTESIAN_POINT('Ctrl Pts',(-16.8637089250448,-50.5780933195443,
-26.5234292553376));
#25799=CARTESIAN_POINT('Ctrl Pts',(-17.8014401781279,-47.6898405229929,
-26.365480732145));
#25800=CARTESIAN_POINT('Ctrl Pts',(-20.7325217649214,-46.8961606035508,
-26.2075322089526));
#25801=CARTESIAN_POINT('Ctrl Pts',(-22.9994819761952,-48.9165945781775,
-26.0495836857601));
#25802=CARTESIAN_POINT('Ctrl Pts',(-22.5468357454767,-51.9194046924401,
-25.8916351625677));
#25803=CARTESIAN_POINT('Ctrl Pts',(-19.7851851224727,-53.1817789190938,
-25.7336866393752));
#25804=CARTESIAN_POINT('Ctrl Pts',(-17.2180335672343,-51.559669523222,-25.5757381161827));
#25805=CARTESIAN_POINT('Ctrl Pts',(-17.1737381144405,-48.522781004423,-25.4177895929902));
#25806=CARTESIAN_POINT('Ctrl Pts',(-19.6908692601881,-46.8265857535405,
-25.2598410697978));
#25807=CARTESIAN_POINT('Ctrl Pts',(-22.4903927825817,-48.0049361420853,
-25.1018925466053));
#25808=CARTESIAN_POINT('Ctrl Pts',(-23.0276908261798,-50.9977151792319,
-24.9439440234128));
#25809=CARTESIAN_POINT('Ctrl Pts',(-21.561846221743,-52.3802071955689,-24.8386450079512));
#25810=CARTESIAN_POINT('Ctrl Pts',(-20.698066426161,-52.6111321859386,-24.7859955002204));
#25811=CARTESIAN_POINT('Ctrl Pts',(-22.1951971040191,-48.1231365609212,
-40.2140044997796));
#25812=CARTESIAN_POINT('Ctrl Pts',(-22.8160759421236,-48.8493222806572,
-40.1613549920488));
#25813=CARTESIAN_POINT('Ctrl Pts',(-23.2701161866361,-50.9540094082019,
-40.0560559765871));
#25814=CARTESIAN_POINT('Ctrl Pts',(-20.9854893034369,-53.2642653970455,
-39.8981074533947));
#25815=CARTESIAN_POINT('Ctrl Pts',(-17.8069643556847,-52.6074309308307,
-39.7401589302022));
#25816=CARTESIAN_POINT('Ctrl Pts',(-16.6170290541443,-49.5901681462734,
-39.5822104070097));
#25817=CARTESIAN_POINT('Ctrl Pts',(-18.4942113068759,-46.9426630818256,
-39.4242618838173));
#25818=CARTESIAN_POINT('Ctrl Pts',(-21.7367065514436,-47.068067982766,-39.2663133606248));
#25819=CARTESIAN_POINT('Ctrl Pts',(-23.4045525404809,-49.8513066991185,
-39.1083648374324));
#25820=CARTESIAN_POINT('Ctrl Pts',(-21.9856094774415,-52.7695920187016,
-38.9504163142398));
#25821=CARTESIAN_POINT('Ctrl Pts',(-18.7663670609349,-53.1766565180384,
-38.7924677910474));
#25822=CARTESIAN_POINT('Ctrl Pts',(-16.665625943007,-50.7036014102206,-38.6345192678549));
#25823=CARTESIAN_POINT('Ctrl Pts',(-17.5880584476031,-47.5925830506814,
-38.4765707446625));
#25824=CARTESIAN_POINT('Ctrl Pts',(-20.697325968444,-46.6643111122205,-38.31862222147));
#25825=CARTESIAN_POINT('Ctrl Pts',(-23.1743487564621,-48.7603994593997,
-38.1606736982775));
#25826=CARTESIAN_POINT('Ctrl Pts',(-22.7732863142562,-51.9803996217343,
-38.002725175085));
#25827=CARTESIAN_POINT('Ctrl Pts',(-19.8577693941567,-53.4048298170276,
-37.8447766518926));
#25828=CARTESIAN_POINT('Ctrl Pts',(-17.0712087001245,-51.7422053051701,
-37.6868281287001));
#25829=CARTESIAN_POINT('Ctrl Pts',(-16.9400939716425,-48.4999757604411,
-37.5288796055077));
#25830=CARTESIAN_POINT('Ctrl Pts',(-19.5833029917492,-46.6177728083202,
-37.3709310823152));
#25831=CARTESIAN_POINT('Ctrl Pts',(-22.6043185081796,-47.802132266691,-37.2129825591227));
#25832=CARTESIAN_POINT('Ctrl Pts',(-23.2640776439233,-50.9792316131993,
-37.0550340359303));
#25833=CARTESIAN_POINT('Ctrl Pts',(-20.9643968503907,-53.2684914081344,
-36.8970855127378));
#25834=CARTESIAN_POINT('Ctrl Pts',(-17.7903267644001,-52.5943094649876,
-36.7391369895453));
#25835=CARTESIAN_POINT('Ctrl Pts',(-16.6197001964587,-49.5679460247584,
-36.5811884663529));
#25836=CARTESIAN_POINT('Ctrl Pts',(-18.5138886534658,-46.9333127873368,
-36.4232399431604));
#25837=CARTESIAN_POINT('Ctrl Pts',(-21.755489070217,-47.0791515746612,-36.2652914199679));
#25838=CARTESIAN_POINT('Ctrl Pts',(-23.4054409378518,-49.8732347966055,
-36.1073428967755));
#25839=CARTESIAN_POINT('Ctrl Pts',(-21.9677830789091,-52.7822521725988,
-35.9493943735829));
#25840=CARTESIAN_POINT('Ctrl Pts',(-18.7459961497524,-53.1686861223123,
-35.7914458503905));
#25841=CARTESIAN_POINT('Ctrl Pts',(-16.6611763728041,-50.6821687360365,
-35.633497327198));
#25842=CARTESIAN_POINT('Ctrl Pts',(-17.603566432908,-47.5771497040813,-35.4755488040056));
#25843=CARTESIAN_POINT('Ctrl Pts',(-20.7187299240599,-46.6688553477443,
-35.3176002808131));
#25844=CARTESIAN_POINT('Ctrl Pts',(-23.1822428522502,-48.780808535438,-35.1596517576206));
#25845=CARTESIAN_POINT('Ctrl Pts',(-22.7605129698462,-51.9981655440101,
-35.0017032344282));
#25846=CARTESIAN_POINT('Ctrl Pts',(-19.8359099348896,-53.4038466252901,
-34.8437547112357));
#25847=CARTESIAN_POINT('Ctrl Pts',(-17.0600823713948,-51.7233634947331,
-34.6858061880432));
#25848=CARTESIAN_POINT('Ctrl Pts',(-16.9497887082035,-48.4803590972339,
-34.5278576648508));
#25849=CARTESIAN_POINT('Ctrl Pts',(-19.6050288553011,-46.6151668884836,
-34.3699091416583));
#25850=CARTESIAN_POINT('Ctrl Pts',(-22.6183773267928,-47.8188999168997,
-34.2119606184658));
#25851=CARTESIAN_POINT('Ctrl Pts',(-23.2577227104281,-51.0001700555025,
-34.0540120952734));
#25852=CARTESIAN_POINT('Ctrl Pts',(-20.9433899916757,-53.2746164235783,
-33.8960635720809));
#25853=CARTESIAN_POINT('Ctrl Pts',(-17.7737142593806,-52.5800676733523,
-33.7381150488884));
#25854=CARTESIAN_POINT('Ctrl Pts',(-16.622544098685,-49.5462500329089,-33.580166525696));
#25855=CARTESIAN_POINT('Ctrl Pts',(-18.5336104830338,-46.9238336874456,
-33.4222180025035));
#25856=CARTESIAN_POINT('Ctrl Pts',(-21.7742076441947,-47.0904837802061,
-33.264269479311));
#25857=CARTESIAN_POINT('Ctrl Pts',(-23.4061846944506,-49.895103740518,-33.1063209561185));
#25858=CARTESIAN_POINT('Ctrl Pts',(-21.9498776766727,-52.7948299490266,
-32.9483724329261));
#25859=CARTESIAN_POINT('Ctrl Pts',(-18.7256758723045,-53.1605688436634,
-32.7904239097336));
#25860=CARTESIAN_POINT('Ctrl Pts',(-16.6568649977014,-50.6607160921068,
-32.6324753865411));
#25861=CARTESIAN_POINT('Ctrl Pts',(-17.6191729528276,-47.5618121546085,
-32.4745268633487));
#25862=CARTESIAN_POINT('Ctrl Pts',(-20.7401043820435,-46.6735389823955,
-32.3165783401562));
#25863=CARTESIAN_POINT('Ctrl Pts',(-23.1900056773179,-48.8012668451058,
-32.1586298169638));
#25864=CARTESIAN_POINT('Ctrl Pts',(-22.7476258446051,-52.0158496015379,
-32.0006812937712));
#25865=CARTESIAN_POINT('Ctrl Pts',(-19.8140572238516,-53.4027228335498,
-31.8427327705788));
#25866=CARTESIAN_POINT('Ctrl Pts',(-17.0490772630378,-51.7044507615189,
-31.6847842473863));
#25867=CARTESIAN_POINT('Ctrl Pts',(-16.9596091995696,-48.4608050225456,
-31.5268357241939));
#25868=CARTESIAN_POINT('Ctrl Pts',(-19.6267710055454,-46.6127005571309,
-31.3688872010014));
#25869=CARTESIAN_POINT('Ctrl Pts',(-22.6323281895464,-47.83575747651,-31.2109386778089));
#25870=CARTESIAN_POINT('Ctrl Pts',(-23.2512334627286,-51.0210672694766,
-31.0529901546164));
#25871=CARTESIAN_POINT('Ctrl Pts',(-20.9223442370508,-53.2806064235659,
-30.895041631424));
#25872=CARTESIAN_POINT('Ctrl Pts',(-17.7571935434708,-52.5657195085423,
-30.7370931082315));
#25873=CARTESIAN_POINT('Ctrl Pts',(-16.6255272521511,-49.5245727479546,
-30.5791445850391));
#25874=CARTESIAN_POINT('Ctrl Pts',(-18.5533927713563,-46.9144814173307,
-30.4211960618466));
#25875=CARTESIAN_POINT('Ctrl Pts',(-21.7928530682033,-47.1019359438065,
-30.2632475386541));
#25876=CARTESIAN_POINT('Ctrl Pts',(-23.4067880152704,-49.9169770094005,
-30.1052990154616));
#25877=CARTESIAN_POINT('Ctrl Pts',(-21.931891881668,-52.807292495538,-29.9473504922692));
#25878=CARTESIAN_POINT('Ctrl Pts',(-18.7054081347881,-53.1523212559188,
-29.7894019690767));
#25879=CARTESIAN_POINT('Ctrl Pts',(-16.6526914588735,-50.6392362070634,
-29.6314534458842));
#25880=CARTESIAN_POINT('Ctrl Pts',(-17.6348776333921,-47.5465751307778,
-29.4735049226918));
#25881=CARTESIAN_POINT('Ctrl Pts',(-20.7614483258065,-46.6783597658239,
-29.3155563994993));
#25882=CARTESIAN_POINT('Ctrl Pts',(-23.1976369795411,-48.8217745781716,
-29.1576078763068));
#25883=CARTESIAN_POINT('Ctrl Pts',(-22.7346254358078,-52.0334505461951,
-28.9996593531144));
#25884=CARTESIAN_POINT('Ctrl Pts',(-19.7922121790031,-53.4014587489637,
-28.8417108299219));
#25885=CARTESIAN_POINT('Ctrl Pts',(-17.0381938205077,-51.6854677539872,
-28.6837623067294));
#25886=CARTESIAN_POINT('Ctrl Pts',(-16.9695550445155,-48.4413144091505,
-28.525813783537));
#25887=CARTESIAN_POINT('Ctrl Pts',(-19.6485285451925,-46.6103738812803,
-28.3678652603445));
#25888=CARTESIAN_POINT('Ctrl Pts',(-22.6461705197463,-47.8527042703631,
-28.209916737152));
#25889=CARTESIAN_POINT('Ctrl Pts',(-23.2446101729951,-51.0419223786568,
-28.0519682139596));
#25890=CARTESIAN_POINT('Ctrl Pts',(-20.9012604442086,-53.2864611783608,
-27.8940196907671));
#25891=CARTESIAN_POINT('Ctrl Pts',(-17.7407653181672,-52.5512655340492,
-27.7360711675746));
#25892=CARTESIAN_POINT('Ctrl Pts',(-16.6286494931318,-49.5029151164213,
-27.5781226443821));
#25893=CARTESIAN_POINT('Ctrl Pts',(-18.5732347840193,-46.9052562590649,
-27.4201741211897));
#25894=CARTESIAN_POINT('Ctrl Pts',(-21.8114244117631,-47.11350779862,-27.2622255979972));
#25895=CARTESIAN_POINT('Ctrl Pts',(-23.4072511974946,-49.9388532929962,
-27.1042770748047));
#25896=CARTESIAN_POINT('Ctrl Pts',(-21.9138257941783,-52.8196401113345,
-26.9463285516123));
#25897=CARTESIAN_POINT('Ctrl Pts',(-18.6851950496672,-53.1439420803989,
-26.7883800284198));
#25898=CARTESIAN_POINT('Ctrl Pts',(-16.6486533860826,-50.6177331895161,
-26.6304315052273));
#25899=CARTESIAN_POINT('Ctrl Pts',(-17.6506848891151,-47.5314328434942,
-26.4724829820349));
#25900=CARTESIAN_POINT('Ctrl Pts',(-20.7827507963447,-46.6833302768041,
-26.3145344588424));
#25901=CARTESIAN_POINT('Ctrl Pts',(-23.2051565126403,-48.842305447693,-26.1565859356499));
#25902=CARTESIAN_POINT('Ctrl Pts',(-22.7214723212287,-52.0510183088916,
-25.9986374124575));
#25903=CARTESIAN_POINT('Ctrl Pts',(-19.7704552622143,-53.3999535603981,
-25.840688889265));
#25904=CARTESIAN_POINT('Ctrl Pts',(-17.0272740757602,-51.6666160922435,
-25.6827403660725));
#25905=CARTESIAN_POINT('Ctrl Pts',(-16.9799412829216,-48.4214880696582,
-25.5247918428801));
#25906=CARTESIAN_POINT('Ctrl Pts',(-19.66967215945,-46.6089846779987,-25.3668433196876));
#25907=CARTESIAN_POINT('Ctrl Pts',(-22.661159063289,-47.8681345752109,-25.2088947964951));
#25908=CARTESIAN_POINT('Ctrl Pts',(-23.2352996440075,-51.0661285281439,
-25.0509462733027));
#25909=CARTESIAN_POINT('Ctrl Pts',(-21.6689420470237,-52.5434180484685,
-24.945647257841));
#25910=CARTESIAN_POINT('Ctrl Pts',(-20.7459328543469,-52.7901775698422,
-24.8929977501102));
#25911=CARTESIAN_POINT('Ctrl Pts',(-22.3360626576961,-48.0026984430693,
-40.3210067496694));
#25912=CARTESIAN_POINT('Ctrl Pts',(-22.996783221692,-48.7754834195626,-40.2683572419386));
#25913=CARTESIAN_POINT('Ctrl Pts',(-23.4799591781266,-51.0152280856744,
-40.1630582264769));
#25914=CARTESIAN_POINT('Ctrl Pts',(-21.0487280422805,-53.4737329440196,
-40.0051097032845));
#25915=CARTESIAN_POINT('Ctrl Pts',(-17.6662375026362,-52.7747494832621,
-39.847161180092));
#25916=CARTESIAN_POINT('Ctrl Pts',(-16.3999441853237,-49.5638692818644,
-39.6892126568996));
#25917=CARTESIAN_POINT('Ctrl Pts',(-18.3975850141438,-46.7464741122942,
-39.5312641337071));
#25918=CARTESIAN_POINT('Ctrl Pts',(-21.8481508174258,-46.8799262317611,
-39.3733156105146));
#25919=CARTESIAN_POINT('Ctrl Pts',(-23.623022297825,-49.8417650665615,-39.2153670873222));
#25920=CARTESIAN_POINT('Ctrl Pts',(-22.1130258164637,-52.9473164300811,
-39.0574185641297));
#25921=CARTESIAN_POINT('Ctrl Pts',(-18.6872049726298,-53.380502213004,-38.8994700409372));
#25922=CARTESIAN_POINT('Ctrl Pts',(-16.4516595311324,-50.7487514343516,
-38.7415215177447));
#25923=CARTESIAN_POINT('Ctrl Pts',(-17.4332844268133,-47.4380993731673,
-38.5835729945523));
#25924=CARTESIAN_POINT('Ctrl Pts',(-20.7420732981751,-46.4502603278007,
-38.4256244713598));
#25925=CARTESIAN_POINT('Ctrl Pts',(-23.3780463626243,-48.6808544307687,
-38.2676759481674));
#25926=CARTESIAN_POINT('Ctrl Pts',(-22.95124778817,-52.107481644896,-38.1097274249748));
#25927=CARTESIAN_POINT('Ctrl Pts',(-19.8486424720205,-53.6233173671768,
-37.9517789017825));
#25928=CARTESIAN_POINT('Ctrl Pts',(-16.8832684886027,-51.8540024255665,
-37.7938303785899));
#25929=CARTESIAN_POINT('Ctrl Pts',(-16.7437401425967,-48.4037193720523,
-37.6358818553975));
#25930=CARTESIAN_POINT('Ctrl Pts',(-19.5565635911389,-46.4007356661223,
-37.477933332205));
#25931=CARTESIAN_POINT('Ctrl Pts',(-22.7714373367961,-47.6610953390299,
-37.3199848090126));
#25932=CARTESIAN_POINT('Ctrl Pts',(-23.4735331428005,-51.0420687967573,
-37.1620362858201));
#25933=CARTESIAN_POINT('Ctrl Pts',(-21.0262820888715,-53.4782301377694,
-37.0040877626276));
#25934=CARTESIAN_POINT('Ctrl Pts',(-17.6485322789718,-52.7607860144173,
-36.8461392394351));
#25935=CARTESIAN_POINT('Ctrl Pts',(-16.402786734543,-49.5402211692867,-36.6881907162427));
#25936=CARTESIAN_POINT('Ctrl Pts',(-18.4185250538729,-46.7365238104494,
-36.5302421930502));
#25937=CARTESIAN_POINT('Ctrl Pts',(-21.868138608337,-46.8917210565137,-36.3722936698577));
#25938=CARTESIAN_POINT('Ctrl Pts',(-23.6239677035562,-49.865100287622,-36.2143451466653));
#25939=CARTESIAN_POINT('Ctrl Pts',(-22.0940554999228,-52.9607889846439,
-36.0563966234728));
#25940=CARTESIAN_POINT('Ctrl Pts',(-18.6655268623454,-53.3720203578719,
-35.8984481002803));
#25941=CARTESIAN_POINT('Ctrl Pts',(-16.4469244325051,-50.725943427852,-35.7404995770878));
#25942=CARTESIAN_POINT('Ctrl Pts',(-17.4497875578081,-47.4216756704347,
-35.5825510538954));
#25943=CARTESIAN_POINT('Ctrl Pts',(-20.764850743239,-46.4550961664119,-35.4246025307029));
#25944=CARTESIAN_POINT('Ctrl Pts',(-23.38644702166,-48.7025731549433,-35.2666540075105));
#25945=CARTESIAN_POINT('Ctrl Pts',(-22.9376547796718,-52.1263876044256,
-35.108705484318));
#25946=CARTESIAN_POINT('Ctrl Pts',(-19.8253802936868,-53.6222710841349,
-34.9507569611255));
#25947=CARTESIAN_POINT('Ctrl Pts',(-16.8714281845976,-51.8339515382522,
-34.792808437933));
#25948=CARTESIAN_POINT('Ctrl Pts',(-16.7540569893232,-48.3828439097519,
-34.6348599147406));
#25949=CARTESIAN_POINT('Ctrl Pts',(-19.5796836009353,-46.3979625246999,
-34.4769113915481));
#25950=CARTESIAN_POINT('Ctrl Pts',(-22.7863983082339,-47.678938967485,-34.3189628683557));
#25951=CARTESIAN_POINT('Ctrl Pts',(-23.4667704139307,-51.0643508565711,
-34.1610143451631));
#25952=CARTESIAN_POINT('Ctrl Pts',(-21.0039272223724,-53.4847481947722,
-34.0030658219707));
#25953=CARTESIAN_POINT('Ctrl Pts',(-17.6308537513554,-52.7456303285988,
-33.8451172987782));
#25954=CARTESIAN_POINT('Ctrl Pts',(-16.4058131296584,-49.5171329480567,
-33.6871687755858));
#25955=CARTESIAN_POINT('Ctrl Pts',(-18.4395124310478,-46.7264364377739,
-33.5292202523933));
#25956=CARTESIAN_POINT('Ctrl Pts',(-21.8880583511222,-46.9037804484265,
-33.3712717292008));
#25957=CARTESIAN_POINT('Ctrl Pts',(-23.6247591869331,-49.8883725592297,
-33.2133232060084));
#25958=CARTESIAN_POINT('Ctrl Pts',(-22.0750011100191,-52.9741738755843,
-33.0553746828159));
#25959=CARTESIAN_POINT('Ctrl Pts',(-18.6439026349568,-53.3633821943561,
-32.8974261596234));
#25960=CARTESIAN_POINT('Ctrl Pts',(-16.4423363969422,-50.7031141701506,
-32.739477636431));
#25961=CARTESIAN_POINT('Ctrl Pts',(-17.4663955463727,-47.4053539121205,
-32.5815291132385));
#25962=CARTESIAN_POINT('Ctrl Pts',(-20.7875967978108,-46.460080349377,-32.423580590046));
#25963=CARTESIAN_POINT('Ctrl Pts',(-23.3947079863477,-48.724344272064,-32.2656320668535));
#25964=CARTESIAN_POINT('Ctrl Pts',(-22.9239406890394,-52.1452064459554,
-32.1076835436611));
#25965=CARTESIAN_POINT('Ctrl Pts',(-19.8021252966153,-53.6210751788038,
-31.9497350204686));
#25966=CARTESIAN_POINT('Ctrl Pts',(-16.859716879663,-51.8138251770541,-31.7917864972762));
#25967=CARTESIAN_POINT('Ctrl Pts',(-16.7645076605265,-48.3620350522686,
-31.6338379740837));
#25968=CARTESIAN_POINT('Ctrl Pts',(-19.6028209425392,-46.3953379291391,
-31.4758894508912));
#25969=CARTESIAN_POINT('Ctrl Pts',(-22.8012443962967,-47.696878274818,-31.3179409276987));
#25970=CARTESIAN_POINT('Ctrl Pts',(-23.459864751929,-51.0865890424386,-31.1599924045063));
#25971=CARTESIAN_POINT('Ctrl Pts',(-20.9815309640172,-53.4911225723918,
-31.0020438813138));
#25972=CARTESIAN_POINT('Ctrl Pts',(-17.6132729029457,-52.730361443651,-30.8440953581213));
#25973=CARTESIAN_POINT('Ctrl Pts',(-16.4089877117502,-49.4940646341411,
-30.6861468349289));
#25974=CARTESIAN_POINT('Ctrl Pts',(-18.4605641466087,-46.7164840335274,
-30.5281983117364));
#25975=CARTESIAN_POINT('Ctrl Pts',(-21.9079002499127,-46.9159674960896,
-30.370249788544));
#25976=CARTESIAN_POINT('Ctrl Pts',(-23.6254012227827,-49.9116494333404,
-30.2123012653514));
#25977=CARTESIAN_POINT('Ctrl Pts',(-22.0558611685522,-52.9874361423172,
-30.054352742159));
#25978=CARTESIAN_POINT('Ctrl Pts',(-18.6223343189813,-53.3546053598246,
-29.8964042189665));
#25979=CARTESIAN_POINT('Ctrl Pts',(-16.4378950425926,-50.6802559232762,
-29.7384556957741));
#25980=CARTESIAN_POINT('Ctrl Pts',(-17.48310799454,-47.3891391301676,-29.5805071725815));
#25981=CARTESIAN_POINT('Ctrl Pts',(-20.810310380068,-46.4652104819412,-29.4225586493892));
#25982=CARTESIAN_POINT('Ctrl Pts',(-23.4028289883847,-48.7461679840765,
-29.2646101261966));
#25983=CARTESIAN_POINT('Ctrl Pts',(-22.9101060454574,-52.163936841271,-29.1066616030042));
#25984=CARTESIAN_POINT('Ctrl Pts',(-19.7788784576719,-53.6197299780505,
-28.9487130798117));
#25985=CARTESIAN_POINT('Ctrl Pts',(-16.8481350478379,-51.7936240320434,
-28.7907645566193));
#25986=CARTESIAN_POINT('Ctrl Pts',(-16.7750917292348,-48.3412937283827,
-28.6328160334268));
#25987=CARTESIAN_POINT('Ctrl Pts',(-19.6259746610823,-46.3928619507583,
-28.4748675102343));
#25988=CARTESIAN_POINT('Ctrl Pts',(-22.8159749872838,-47.7149125425452,
-28.3169189870419));
#25989=CARTESIAN_POINT('Ctrl Pts',(-23.4528164464309,-51.1087824216521,
-28.1589704638493));
#25990=CARTESIAN_POINT('Ctrl Pts',(-20.9590942265365,-53.4973530261498,
-28.0010219406569));
#25991=CARTESIAN_POINT('Ctrl Pts',(-17.595790480254,-52.7149799592246,-27.8430734174644));
#25992=CARTESIAN_POINT('Ctrl Pts',(-16.4123103065868,-49.4710172348044,
-27.685124894272));
#25993=CARTESIAN_POINT('Ctrl Pts',(-18.4816794190144,-46.7066668978831,
-27.5271763710795));
#25994=CARTESIAN_POINT('Ctrl Pts',(-21.9276633145204,-46.9282819155376,
-27.369227847887));
#25995=CARTESIAN_POINT('Ctrl Pts',(-23.6258941273587,-49.9349295156179,
-27.2112793246946));
#25996=CARTESIAN_POINT('Ctrl Pts',(-22.0366357822403,-53.0005761032442,
-27.0533308015021));
#25997=CARTESIAN_POINT('Ctrl Pts',(-18.6008241624394,-53.3456884935447,
-26.8953822783096));
#25998=CARTESIAN_POINT('Ctrl Pts',(-16.4335978471204,-50.657373059488,-26.7374337551171));
#25999=CARTESIAN_POINT('Ctrl Pts',(-17.4999296001022,-47.3730251639953,
-26.5794852319247));
#26000=CARTESIAN_POINT('Ctrl Pts',(-20.8329798277681,-46.4704999500574,
-26.4215367087322));
#26001=CARTESIAN_POINT('Ctrl Pts',(-23.4108310490853,-48.7680163172086,
-26.2635881855398));
#26002=CARTESIAN_POINT('Ctrl Pts',(-22.8961088969807,-52.1826319253429,
-26.1056396623473));
#26003=CARTESIAN_POINT('Ctrl Pts',(-19.7557254019559,-53.6181282017024,
-25.9476911391548));
#26004=CARTESIAN_POINT('Ctrl Pts',(-16.8365145842861,-51.7735626612651,
-25.7897426159623));
#26005=CARTESIAN_POINT('Ctrl Pts',(-16.7861444514027,-48.3201951348933,
-25.6317940927699));
#26006=CARTESIAN_POINT('Ctrl Pts',(-19.6484750587118,-46.3913836024568,
-25.4738455695774));
#26007=CARTESIAN_POINT('Ctrl Pts',(-22.8319253439964,-47.7313330083366,
-25.3158970463849));
#26008=CARTESIAN_POINT('Ctrl Pts',(-23.4429084618352,-51.1345418770559,
-25.1579485231925));
#26009=CARTESIAN_POINT('Ctrl Pts',(-21.7760378723045,-52.706628901368,-25.0526495077308));
#26010=CARTESIAN_POINT('Ctrl Pts',(-20.7937992825329,-52.9692229537457,
-25.));
#26011=CARTESIAN_POINT('Ctrl Pts',(-17.4818816223345,-50.0021988885187,
-38.387416697508));
#26012=CARTESIAN_POINT('Ctrl Pts',(-17.4802992936945,-50.1765619490587,
-38.3984493876971));
#26013=CARTESIAN_POINT('Ctrl Pts',(-17.4968845768144,-50.3506259225462,
-38.4094820778862));
#26014=CARTESIAN_POINT('Ctrl Pts',(-17.5327554656256,-50.5206201636086,
-38.4205147680753));
#26015=CARTESIAN_POINT('Ctrl Pts',(-17.7039362570194,-51.3318559506749,
-38.4731642758061));
#26016=CARTESIAN_POINT('Ctrl Pts',(-18.3143137472823,-52.0504105393911,
-38.525813783537));
#26017=CARTESIAN_POINT('Ctrl Pts',(-19.0871834193891,-52.350550845055,-38.5784632912678));
#26018=CARTESIAN_POINT('Ctrl Pts',(-19.8600530914959,-52.650691150719,-38.6311127989986));
#26019=CARTESIAN_POINT('Ctrl Pts',(-20.7954149454465,-52.5324171733308,
-38.6837623067294));
#26020=CARTESIAN_POINT('Ctrl Pts',(-21.4692352434878,-52.049321312685,-38.7364118144602));
#26021=CARTESIAN_POINT('Ctrl Pts',(-22.1430555415291,-51.5662254520392,
-38.7890613221911));
#26022=CARTESIAN_POINT('Ctrl Pts',(-22.555334283661,-50.7183077081358,-38.8417108299219));
#26023=CARTESIAN_POINT('Ctrl Pts',(-22.519174487008,-49.890009089608,-38.8943603376527));
#26024=CARTESIAN_POINT('Ctrl Pts',(-22.483014690355,-49.0617104710802,-38.9470098453835));
#26025=CARTESIAN_POINT('Ctrl Pts',(-21.9984163549171,-48.2530309779281,
-38.9996593531144));
#26026=CARTESIAN_POINT('Ctrl Pts',(-21.2850581660083,-47.8304728207041,
-39.0523088608452));
#26027=CARTESIAN_POINT('Ctrl Pts',(-20.5716999770995,-47.4079146634801,
-39.104958368576));
#26028=CARTESIAN_POINT('Ctrl Pts',(-19.6295819347198,-47.3714778421842,
-39.1576078763068));
#26029=CARTESIAN_POINT('Ctrl Pts',(-18.8858120634375,-47.7378802405701,
-39.2102573840377));
#26030=CARTESIAN_POINT('Ctrl Pts',(-18.1420421921552,-48.1042826389561,
-39.2629068917685));
#26031=CARTESIAN_POINT('Ctrl Pts',(-17.5966204919703,-48.8735242570238,
-39.3155563994993));
#26032=CARTESIAN_POINT('Ctrl Pts',(-17.4967795202106,-49.6964830578704,
-39.3682059072301));
#26033=CARTESIAN_POINT('Ctrl Pts',(-17.4846361716636,-49.7965769910764,
-39.3746095039894));
#26034=CARTESIAN_POINT('Ctrl Pts',(-17.4790843453548,-49.8974655681758,
-39.3810131007487));
#26035=CARTESIAN_POINT('Ctrl Pts',(-17.4798421274757,-49.9984351524252,
-39.387416697508));
#26036=CARTESIAN_POINT('Ctrl Pts',(-19.2062007174672,-52.9692229537457,
-40.));
#26037=CARTESIAN_POINT('Ctrl Pts',(-18.2239621276955,-52.7066289013681,
-39.9473504922692));
#26038=CARTESIAN_POINT('Ctrl Pts',(-16.5570904206518,-51.1345489516877,
-39.8420514768075));
#26039=CARTESIAN_POINT('Ctrl Pts',(-17.1680756287354,-47.7313299839058,
-39.6841029536151));
#26040=CARTESIAN_POINT('Ctrl Pts',(-20.3515248249563,-46.3913860864081,
-39.5261544304226));
#26041=CARTESIAN_POINT('Ctrl Pts',(-23.2138549612499,-48.3201943023511,
-39.3682059072301));
#26042=CARTESIAN_POINT('Ctrl Pts',(-23.1634850140729,-51.7735630043146,
-39.2102573840376));
#26043=CARTESIAN_POINT('Ctrl Pts',(-20.2442744821096,-53.6181272821323,
-39.0523088608452));
#26044=CARTESIAN_POINT('Ctrl Pts',(-17.1038916129568,-52.1826317747292,
-38.8943603376527));
#26045=CARTESIAN_POINT('Ctrl Pts',(-16.5891694547899,-48.7680164050864,
-38.7364118144603));
#26046=CARTESIAN_POINT('Ctrl Pts',(-19.1670203242729,-46.4705005646606,
-38.5784632912678));
#26047=CARTESIAN_POINT('Ctrl Pts',(-22.5000699934528,-47.373025546768,-38.4205147680754));
#26048=CARTESIAN_POINT('Ctrl Pts',(-23.5664015975527,-50.657372972797,-38.2625662448828));
#26049=CARTESIAN_POINT('Ctrl Pts',(-21.3991756129266,-53.3456879568638,
-38.1046177216904));
#26050=CARTESIAN_POINT('Ctrl Pts',(-17.9633645411529,-53.0005756349581,
-37.9466691984979));
#26051=CARTESIAN_POINT('Ctrl Pts',(-16.3741064431585,-49.9349295232864,
-37.7887206753054));
#26052=CARTESIAN_POINT('Ctrl Pts',(-18.0723369901302,-46.9282824012858,
-37.630772152113));
#26053=CARTESIAN_POINT('Ctrl Pts',(-21.5183203411933,-46.7066674164727,
-37.4728236289205));
#26054=CARTESIAN_POINT('Ctrl Pts',(-23.5876891278802,-49.4710173186029,
-37.3148751057281));
#26055=CARTESIAN_POINT('Ctrl Pts',(-22.4042091405233,-52.7149795309031,
-37.1569265825355));
#26056=CARTESIAN_POINT('Ctrl Pts',(-19.0409059247592,-53.4973524747668,
-36.9989780593431));
#26057=CARTESIAN_POINT('Ctrl Pts',(-16.5471840980045,-51.1087822467551,
-36.8410295361506));
#26058=CARTESIAN_POINT('Ctrl Pts',(-17.1840254567772,-47.7149129029046,
-36.6830810129582));
#26059=CARTESIAN_POINT('Ctrl Pts',(-20.3740252799296,-46.3928625195443,
-36.5251324897657));
#26060=CARTESIAN_POINT('Ctrl Pts',(-23.2249077622416,-48.3412939899481,
-36.3671839665732));
#26061=CARTESIAN_POINT('Ctrl Pts',(-23.1518644551494,-51.7936237492067,
-36.2092354433807));
#26062=CARTESIAN_POINT('Ctrl Pts',(-20.2211215074614,-53.6197294072659,
-36.0512869201883));
#26063=CARTESIAN_POINT('Ctrl Pts',(-17.0898944134298,-52.1639365000438,
-35.8933383969958));
#26064=CARTESIAN_POINT('Ctrl Pts',(-16.5971715481998,-48.746168181791,-35.7353898738033));
#26065=CARTESIAN_POINT('Ctrl Pts',(-19.1896897477077,-46.4652110393336,
-35.5774413506109));
#26066=CARTESIAN_POINT('Ctrl Pts',(-22.5168916085772,-47.3891395418682,
-35.4194928274184));
#26067=CARTESIAN_POINT('Ctrl Pts',(-23.5621043957074,-50.6802558160081,
-35.261544304226));
#26068=CARTESIAN_POINT('Ctrl Pts',(-21.3776654637779,-53.3546048308447,
-35.1035957810335));
#26069=CARTESIAN_POINT('Ctrl Pts',(-17.9441391556319,-52.9874356712354,
-34.945647257841));
#26070=CARTESIAN_POINT('Ctrl Pts',(-16.3745993488984,-49.9116494472723,
-34.7876987346485));
#26071=CARTESIAN_POINT('Ctrl Pts',(-18.0921000509396,-46.9159679824036,
-34.6297502114561));
#26072=CARTESIAN_POINT('Ctrl Pts',(-21.5394356106412,-46.7164845512972,
-34.4718016882636));
#26073=CARTESIAN_POINT('Ctrl Pts',(-23.5910117219915,-49.4940647139208,
-34.3138531650712));
#26074=CARTESIAN_POINT('Ctrl Pts',(-22.386726720697,-52.7303610131065,-34.1559046418786));
#26075=CARTESIAN_POINT('Ctrl Pts',(-19.0184691907583,-53.491122021885,-33.9979561186862));
#26076=CARTESIAN_POINT('Ctrl Pts',(-16.540135793649,-51.086588871097,-33.8400075954937));
#26077=CARTESIAN_POINT('Ctrl Pts',(-17.1987560454249,-47.696878637992,-33.6820590723013));
#26078=CARTESIAN_POINT('Ctrl Pts',(-20.3971789948304,-46.3953384975499,
-33.5241105491088));
#26079=CARTESIAN_POINT('Ctrl Pts',(-23.2354918292762,-48.3620353105553,
-33.3661620259163));
#26080=CARTESIAN_POINT('Ctrl Pts',(-23.1402826251531,-51.8138248910362,
-33.2082135027239));
#26081=CARTESIAN_POINT('Ctrl Pts',(-20.1978746721824,-53.6210746078049,
-33.0502649795314));
#26082=CARTESIAN_POINT('Ctrl Pts',(-17.0760597720301,-52.1452061076829,
-32.8923164563389));
#26083=CARTESIAN_POINT('Ctrl Pts',(-16.6052925489559,-48.7243444732193,
-32.7343679331465));
#26084=CARTESIAN_POINT('Ctrl Pts',(-19.2124033263834,-46.4600809075787,
-32.576419409954));
#26085=CARTESIAN_POINT('Ctrl Pts',(-22.533604054109,-47.405354321264,-32.4184708867615));
#26086=CARTESIAN_POINT('Ctrl Pts',(-23.5576630420582,-50.7031140592781,
-32.2605223635691));
#26087=CARTESIAN_POINT('Ctrl Pts',(-21.3560971512034,-53.3633816639922,
-32.1025738403766));
#26088=CARTESIAN_POINT('Ctrl Pts',(-17.9249992171831,-52.9741734065938,
-31.9446253171841));
#26089=CARTESIAN_POINT('Ctrl Pts',(-16.3752413846467,-49.8883725768321,
-31.7866767939917));
#26090=CARTESIAN_POINT('Ctrl Pts',(-18.1119419466013,-46.9037809366621,
-31.6287282707992));
#26091=CARTESIAN_POINT('Ctrl Pts',(-21.5604873228824,-46.7264369539744,
-31.4707797476067));
#26092=CARTESIAN_POINT('Ctrl Pts',(-23.5941863035827,-49.5171330241987,
-31.3128312244142));
#26093=CARTESIAN_POINT('Ctrl Pts',(-22.3691458750596,-52.7456298956467,
-31.1548827012218));
#26094=CARTESIAN_POINT('Ctrl Pts',(-18.9960729359346,-53.4847476452704,
-30.9969341780293));
#26095=CARTESIAN_POINT('Ctrl Pts',(-16.5332301327363,-51.0643506887362,
-30.8389856548368));
#26096=CARTESIAN_POINT('Ctrl Pts',(-17.2136021311466,-47.6789393334878,
-30.6810371316444));
#26097=CARTESIAN_POINT('Ctrl Pts',(-20.4203163327858,-46.3979630926968,
-30.5230886084519));
#26098=CARTESIAN_POINT('Ctrl Pts',(-23.2459424988316,-48.3828441647573,
-30.3651400852595));
#26099=CARTESIAN_POINT('Ctrl Pts',(-23.1285713220653,-51.8339512490605,
-30.207191562067));
#26100=CARTESIAN_POINT('Ctrl Pts',(-20.1746196787779,-53.6222705129474,
-30.0492430388745));
#26101=CARTESIAN_POINT('Ctrl Pts',(-17.0623456835602,-52.1263872691206,
-29.891294515682));
#26102=CARTESIAN_POINT('Ctrl Pts',(-16.6135535123409,-48.7025733595317,
-29.7333459924896));
#26103=CARTESIAN_POINT('Ctrl Pts',(-19.2351493773684,-46.4550967253995,
-29.5753974692971));
#26104=CARTESIAN_POINT('Ctrl Pts',(-22.5502120400548,-47.4216760770047,
-29.4174489461046));
#26105=CARTESIAN_POINT('Ctrl Pts',(-23.5530750072187,-50.7259433133794,
-29.2595004229121));
#26106=CARTESIAN_POINT('Ctrl Pts',(-21.3344729272248,-53.3720198261462,
-29.1015518997197));
#26107=CARTESIAN_POINT('Ctrl Pts',(-17.905944830284,-52.9607885177635,-28.9436033765272));
#26108=CARTESIAN_POINT('Ctrl Pts',(-16.3760328678989,-49.8651003088954,
-28.7856548533348));
#26109=CARTESIAN_POINT('Ctrl Pts',(-18.1318616862451,-46.8917215466485,
-28.6277063301423));
#26110=CARTESIAN_POINT('Ctrl Pts',(-21.5814746967481,-46.7365243250642,
-28.4697578069498));
#26111=CARTESIAN_POINT('Ctrl Pts',(-23.5972126982202,-49.5402212417787,
-28.3118092837573));
#26112=CARTESIAN_POINT('Ctrl Pts',(-22.3514673502323,-52.7607855790929,
-28.1538607605649));
#26113=CARTESIAN_POINT('Ctrl Pts',(-18.9737180729577,-53.4782295892619,
-27.9959122373724));
#26114=CARTESIAN_POINT('Ctrl Pts',(-16.5264674049389,-51.0420686324998,
-27.83796371418));
#26115=CARTESIAN_POINT('Ctrl Pts',(-17.2285631002129,-47.6610957077258,
-27.6800151909875));
#26116=CARTESIAN_POINT('Ctrl Pts',(-20.4434363389617,-46.4007362339102,
-27.522066667795));
#26117=CARTESIAN_POINT('Ctrl Pts',(-23.2562593438794,-48.403719623335,-27.3641181446025));
#26118=CARTESIAN_POINT('Ctrl Pts',(-23.1167310200335,-51.8540021340239,
-27.2061696214101));
#26119=CARTESIAN_POINT('Ctrl Pts',(-20.1513575038949,-53.623316794304,-27.0482210982176));
#26120=CARTESIAN_POINT('Ctrl Pts',(-17.0487526776507,-52.1074813154118,
-26.8902725750251));
#26121=CARTESIAN_POINT('Ctrl Pts',(-16.6219541691413,-48.6808546335012,
-26.7323240518326));
#26122=CARTESIAN_POINT('Ctrl Pts',(-19.2579268207016,-46.4502608973225,
-26.5743755286402));
#26123=CARTESIAN_POINT('Ctrl Pts',(-22.5667151646459,-47.4380997591695,
-26.4164270054477));
#26124=CARTESIAN_POINT('Ctrl Pts',(-23.5483399170972,-50.748751349135,-26.2584784822553));
#26125=CARTESIAN_POINT('Ctrl Pts',(-21.312794804531,-53.3805016203859,-26.1005299590628));
#26126=CARTESIAN_POINT('Ctrl Pts',(-17.8869745490034,-52.9473160722452,
-25.9425814358703));
#26127=CARTESIAN_POINT('Ctrl Pts',(-16.3769782077294,-49.8417649018331,
-25.7846329126779));
#26128=CARTESIAN_POINT('Ctrl Pts',(-18.1518496079148,-46.8799270552508,
-25.6266843894854));
#26129=CARTESIAN_POINT('Ctrl Pts',(-21.6024144605454,-46.7464740570925,
-25.468735866293));
#26130=CARTESIAN_POINT('Ctrl Pts',(-23.6000558022285,-49.5638703006617,
-25.3107873431004));
#26131=CARTESIAN_POINT('Ctrl Pts',(-22.3337609944815,-52.7747475021281,
-25.152838819908));
#26132=CARTESIAN_POINT('Ctrl Pts',(-18.9512744725129,-53.4737348854633,
-24.9948902967155));
#26133=CARTESIAN_POINT('Ctrl Pts',(-16.5200358935638,-51.0152228884625,
-24.836941773523));
#26134=CARTESIAN_POINT('Ctrl Pts',(-17.003216778308,-48.7754834195627,-24.7316427580614));
#26135=CARTESIAN_POINT('Ctrl Pts',(-17.6639373423038,-48.0026984430694,
-24.6789932503306));
#26136=CARTESIAN_POINT('Ctrl Pts',(-19.2540671456531,-52.7901775698422,
-40.1070022498898));
#26137=CARTESIAN_POINT('Ctrl Pts',(-18.3310579529763,-52.5434180484685,
-40.054352742159));
#26138=CARTESIAN_POINT('Ctrl Pts',(-16.764699305866,-51.0661351761724,-39.9490537266973));
#26139=CARTESIAN_POINT('Ctrl Pts',(-17.3388418507866,-47.8681317331546,
-39.7911052035049));
#26140=CARTESIAN_POINT('Ctrl Pts',(-20.330327731233,-46.6089870121667,-39.6331566803124));
#26141=CARTESIAN_POINT('Ctrl Pts',(-23.0200581651483,-48.4214872873186,
-39.4752081571199));
#26142=CARTESIAN_POINT('Ctrl Pts',(-22.9727255468179,-51.666616414607,-39.3172596339275));
#26143=CARTESIAN_POINT('Ctrl Pts',(-20.2295446288421,-53.3999526962785,
-39.159311110735));
#26144=CARTESIAN_POINT('Ctrl Pts',(-17.2785281579593,-52.0510181673598,
-39.0013625875425));
#26145=CARTESIAN_POINT('Ctrl Pts',(-16.7948439608511,-48.8423055302719,
-38.8434140643501));
#26146=CARTESIAN_POINT('Ctrl Pts',(-19.2172493465281,-46.6833308543465,
-38.6854655411576));
#26147=CARTESIAN_POINT('Ctrl Pts',(-22.3493147289487,-47.5314332031855,
-38.5275170179651));
#26148=CARTESIAN_POINT('Ctrl Pts',(-23.3513460920769,-50.6177331080526,
-38.3695684947727));
#26149=CARTESIAN_POINT('Ctrl Pts',(-21.3148047392443,-53.14394157608,-38.2116199715802));
#26150=CARTESIAN_POINT('Ctrl Pts',(-18.0861745097142,-52.8196396712863,
-38.0536714483877));
#26151=CARTESIAN_POINT('Ctrl Pts',(-16.5927493386201,-49.9388533002023,
-37.8957229251952));
#26152=CARTESIAN_POINT('Ctrl Pts',(-18.1885758745169,-47.1135082550774,
-37.7377744020028));
#26153=CARTESIAN_POINT('Ctrl Pts',(-21.426764990648,-46.9052567463833,-37.5798258788103));
#26154=CARTESIAN_POINT('Ctrl Pts',(-23.3713499754371,-49.5029151951668,
-37.4218773556179));
#26155=CARTESIAN_POINT('Ctrl Pts',(-22.2592343254774,-52.5512651315557,
-37.2639288324253));
#26156=CARTESIAN_POINT('Ctrl Pts',(-19.0987396979639,-53.2864606602264,
-37.1059803092329));
#26157=CARTESIAN_POINT('Ctrl Pts',(-16.7553903386107,-51.0419222143061,
-36.9480317860404));
#26158=CARTESIAN_POINT('Ctrl Pts',(-17.3538298975377,-47.8527046089926,
-36.790083262848));
#26159=CARTESIAN_POINT('Ctrl Pts',(-20.3514713993765,-46.6103744157683,
-36.6321347396555));
#26160=CARTESIAN_POINT('Ctrl Pts',(-23.0304444776251,-48.4413146549433,
-36.474186216463));
#26161=CARTESIAN_POINT('Ctrl Pts',(-22.9618057124497,-51.6854674882058,
-36.3162376932706));
#26162=CARTESIAN_POINT('Ctrl Pts',(-20.2077877882326,-53.4014582125975,
-36.1582891700781));
#26163=CARTESIAN_POINT('Ctrl Pts',(-17.2653749954083,-52.0334502255441,
-36.0003406468856));
#26164=CARTESIAN_POINT('Ctrl Pts',(-16.8023635246871,-48.8217747639638,
-35.8423921236932));
#26165=CARTESIAN_POINT('Ctrl Pts',(-19.2385517942642,-46.6783602896053,
-35.6844436005007));
#26166=CARTESIAN_POINT('Ctrl Pts',(-22.3651219936574,-47.5465755176528,
-35.5264950773082));
#26167=CARTESIAN_POINT('Ctrl Pts',(-23.3473080132972,-50.6392361062634,
-35.3685465541158));
#26168=CARTESIAN_POINT('Ctrl Pts',(-21.2945916610709,-53.1523207588367,
-35.2105980309233));
#26169=CARTESIAN_POINT('Ctrl Pts',(-18.0681084229676,-52.8072920528626,
-35.0526495077308));
#26170=CARTESIAN_POINT('Ctrl Pts',(-16.5932125219381,-49.9169770224924,
-34.8947009845383));
#26171=CARTESIAN_POINT('Ctrl Pts',(-18.2071472145074,-47.1019364007955,
-34.7367524613459));
#26172=CARTESIAN_POINT('Ctrl Pts',(-21.4466070005315,-46.9144819038789,
-34.5788039381534));
#26173=CARTESIAN_POINT('Ctrl Pts',(-23.3744722157361,-49.5245728229235,
-34.420855414961));
#26174=CARTESIAN_POINT('Ctrl Pts',(-22.2428061028663,-52.5657191039599,
-34.2629068917685));
#26175=CARTESIAN_POINT('Ctrl Pts',(-19.0776559083916,-53.2806059062547,
-34.104958368576));
#26176=CARTESIAN_POINT('Ctrl Pts',(-16.7487670499508,-51.021067108467,-33.9470098453835));
#26177=CARTESIAN_POINT('Ctrl Pts',(-17.3676722255392,-47.8357578177845,
-33.7890613221911));
#26178=CARTESIAN_POINT('Ctrl Pts',(-20.3732289356009,-46.6127010912662,
-33.6311127989986));
#26179=CARTESIAN_POINT('Ctrl Pts',(-23.0403903209982,-48.4608052652575,
-33.4731642758061));
#26180=CARTESIAN_POINT('Ctrl Pts',(-22.9509222716381,-51.704450492748,-33.3152157526137));
#26181=CARTESIAN_POINT('Ctrl Pts',(-20.1859427468276,-53.4027222969824,
-33.1572672294212));
#26182=CARTESIAN_POINT('Ctrl Pts',(-17.2523745886616,-52.0158492836633,
-32.9993187062287));
#26183=CARTESIAN_POINT('Ctrl Pts',(-16.8099948257066,-48.8012670341315,
-32.8413701830363));
#26184=CARTESIAN_POINT('Ctrl Pts',(-19.2598957346618,-46.6735395069373,
-32.6834216598438));
#26185=CARTESIAN_POINT('Ctrl Pts',(-22.3808266717453,-47.5618125390806,
-32.5254731366513));
#26186=CARTESIAN_POINT('Ctrl Pts',(-23.3431344751275,-50.6607159879198,
-32.3675246134589));
#26187=CARTESIAN_POINT('Ctrl Pts',(-21.2743239267504,-53.1605683452807,
-32.2095760902664));
#26188=CARTESIAN_POINT('Ctrl Pts',(-18.0501226307991,-52.7948295083164,
-32.0516275670739));
#26189=CARTESIAN_POINT('Ctrl Pts',(-16.5938158426627,-49.895103757059,-31.8936790438815));
#26190=CARTESIAN_POINT('Ctrl Pts',(-18.2257926355758,-47.0904842390009,
-31.7357305206889));
#26191=CARTESIAN_POINT('Ctrl Pts',(-21.4663892857345,-46.9238341725191,
-31.5777819974966));
#26192=CARTESIAN_POINT('Ctrl Pts',(-23.3774553687318,-49.5462501044595,
-31.419833474304));
#26193=CARTESIAN_POINT('Ctrl Pts',(-22.2262853895617,-52.5800672665074,
-31.2618849511117));
#26194=CARTESIAN_POINT('Ctrl Pts',(-19.0566101570854,-53.2746159072117,
-31.1039364279191));
#26195=CARTESIAN_POINT('Ctrl Pts',(-16.7422778032747,-51.000169897788,-30.9459879047267));
#26196=CARTESIAN_POINT('Ctrl Pts',(-17.3816230860929,-47.8189002608325,
-30.7880393815342));
#26197=CARTESIAN_POINT('Ctrl Pts',(-20.3949710824167,-46.6151674222299,
-30.6300908583417));
#26198=CARTESIAN_POINT('Ctrl Pts',(-23.0502108108157,-48.4803593368625,
-30.4721423351493));
#26199=CARTESIAN_POINT('Ctrl Pts',(-22.9399171650165,-51.7233632229797,
-30.3141938119568));
#26200=CARTESIAN_POINT('Ctrl Pts',(-20.1640900392355,-53.4038460885454,
-30.1562452887643));
#26201=CARTESIAN_POINT('Ctrl Pts',(-17.2394874654528,-51.9981652289242,
-29.9982967655718));
#26202=CARTESIAN_POINT('Ctrl Pts',(-16.8177576495502,-48.7808087276896,
-29.8403482423794));
#26203=CARTESIAN_POINT('Ctrl Pts',(-19.2812701892749,-46.6688558730247,
-29.6823997191869));
#26204=CARTESIAN_POINT('Ctrl Pts',(-22.3964331892039,-47.5771500861349,
-29.5244511959945));
#26205=CARTESIAN_POINT('Ctrl Pts',(-23.3388231007046,-50.6821686284665,
-29.3665026728019));
#26206=CARTESIAN_POINT('Ctrl Pts',(-21.2540036525068,-53.1686856226499,
-29.2085541496095));
#26207=CARTESIAN_POINT('Ctrl Pts',(-18.0322172313861,-52.7822517338714,
-29.050605626417));
#26208=CARTESIAN_POINT('Ctrl Pts',(-16.5945595991443,-49.8732348165961,
-28.8926571032245));
#26209=CARTESIAN_POINT('Ctrl Pts',(-18.2445112066017,-47.0791520352407,
-28.7347085800321));
#26210=CARTESIAN_POINT('Ctrl Pts',(-21.4861111121929,-46.93331327092,-28.5767600568396));
#26211=CARTESIAN_POINT('Ctrl Pts',(-23.3802992705091,-49.5679460928791,
-28.4188115336471));
#26212=CARTESIAN_POINT('Ctrl Pts',(-22.2096728871631,-52.5943090559135,
-28.2608630104547));
#26213=CARTESIAN_POINT('Ctrl Pts',(-19.0356033016802,-53.2684908927021,
-28.1029144872622));
#26214=CARTESIAN_POINT('Ctrl Pts',(-16.7359228707871,-50.9792314588465,
-27.9449659640698));
#26215=CARTESIAN_POINT('Ctrl Pts',(-17.3956819024776,-47.8021326131544,
-27.7870174408773));
#26216=CARTESIAN_POINT('Ctrl Pts',(-20.4166969425664,-46.6177733418703,
-27.6290689176848));
#26217=CARTESIAN_POINT('Ctrl Pts',(-23.0599055457993,-48.4999759965714,
-27.4711203944923));
#26218=CARTESIAN_POINT('Ctrl Pts',(-22.9287908381411,-51.7422050312076,
-27.3131718712999));
#26219=CARTESIAN_POINT('Ctrl Pts',(-20.1422305832111,-53.4048292786993,
-27.1552233481074));
#26220=CARTESIAN_POINT('Ctrl Pts',(-17.2267141234753,-51.9803993121182,
-26.9972748249149));
#26221=CARTESIAN_POINT('Ctrl Pts',(-16.8256517432378,-48.7603996499074,
-26.8393263017224));
#26222=CARTESIAN_POINT('Ctrl Pts',(-19.3026741432644,-46.6643116473999,
-26.68137777853));
#26223=CARTESIAN_POINT('Ctrl Pts',(-22.4119411684913,-47.5925834134076,
-26.5234292553375));
#26224=CARTESIAN_POINT('Ctrl Pts',(-23.3343735384945,-50.7036013301426,
-26.3654807321451));
#26225=CARTESIAN_POINT('Ctrl Pts',(-21.2336327296632,-53.1766559611554,
-26.2075322089526));
#26226=CARTESIAN_POINT('Ctrl Pts',(-18.0143908659877,-52.7695916824433,
-26.0495836857601));
#26227=CARTESIAN_POINT('Ctrl Pts',(-16.5954479345883,-49.8513065443232,
-25.8916351625677));
#26228=CARTESIAN_POINT('Ctrl Pts',(-18.2632938482488,-47.068068756599,-25.7336866393752));
#26229=CARTESIAN_POINT('Ctrl Pts',(-21.5057881994898,-46.9426630299526,
-25.5757381161827));
#26230=CARTESIAN_POINT('Ctrl Pts',(-23.3829709341586,-49.5901691036368,
-25.4177895929902));
#26231=CARTESIAN_POINT('Ctrl Pts',(-22.1930342320574,-52.60742906916,-25.2598410697978));
#26232=CARTESIAN_POINT('Ctrl Pts',(-19.0145130597135,-53.2642672214192,
-25.1018925466053));
#26233=CARTESIAN_POINT('Ctrl Pts',(-16.7298791822334,-50.9540045243841,
-24.9439440234128));
#26234=CARTESIAN_POINT('Ctrl Pts',(-17.1839240578764,-48.8493222806574,
-24.8386450079512));
#26235=CARTESIAN_POINT('Ctrl Pts',(-17.8048028959808,-48.1231365609213,
-24.7859955002204));
#26236=CARTESIAN_POINT('Ctrl Pts',(-19.301933573839,-52.6111321859386,-40.2140044997796));
#26237=CARTESIAN_POINT('Ctrl Pts',(-18.4381537782571,-52.3802071955689,
-40.1613549920488));
#26238=CARTESIAN_POINT('Ctrl Pts',(-16.9723081910803,-50.9977214006572,
-40.0560559765871));
#26239=CARTESIAN_POINT('Ctrl Pts',(-17.5096080728378,-48.0049334824034,
-39.8981074533947));
#26240=CARTESIAN_POINT('Ctrl Pts',(-20.3091306375097,-46.8265879379253,
-39.7401589302022));
#26241=CARTESIAN_POINT('Ctrl Pts',(-22.8262613690466,-48.522780272286,-39.5822104070098));
#26242=CARTESIAN_POINT('Ctrl Pts',(-22.781966079563,-51.5596698248994,-39.4242618838172));
#26243=CARTESIAN_POINT('Ctrl Pts',(-20.2148147755746,-53.1817781104246,
-39.2663133606248));
#26244=CARTESIAN_POINT('Ctrl Pts',(-17.4531647029619,-51.9194045599905,
-39.1083648374323));
#26245=CARTESIAN_POINT('Ctrl Pts',(-17.0005184669122,-48.9165946554572,
-38.9504163142399));
#26246=CARTESIAN_POINT('Ctrl Pts',(-19.2674783687833,-46.8961611440324,
-38.7924677910474));
#26247=CARTESIAN_POINT('Ctrl Pts',(-22.1985594644447,-47.6898408596029,
-38.634519267855));
#26248=CARTESIAN_POINT('Ctrl Pts',(-23.1362905866011,-50.5780932433083,
-38.4765707446625));
#26249=CARTESIAN_POINT('Ctrl Pts',(-21.2304338655621,-52.9421951952963,
-38.31862222147));
#26250=CARTESIAN_POINT('Ctrl Pts',(-18.2089844782754,-52.6387037076143,
-38.1606736982775));
#26251=CARTESIAN_POINT('Ctrl Pts',(-16.8113922340818,-49.9427770771181,
-38.002725175085));
#26252=CARTESIAN_POINT('Ctrl Pts',(-18.3048147589036,-47.298734108869,-37.8447766518926));
#26253=CARTESIAN_POINT('Ctrl Pts',(-21.3352096401026,-47.103846076294,-37.6868281287001));
#26254=CARTESIAN_POINT('Ctrl Pts',(-23.1550108229941,-49.5348130717306,
-37.5288796055077));
#26255=CARTESIAN_POINT('Ctrl Pts',(-22.1142595104314,-52.3875507322084,
-37.3709310823152));
#26256=CARTESIAN_POINT('Ctrl Pts',(-19.1565734711686,-53.0755688456859,
-37.2129825591228));
#26257=CARTESIAN_POINT('Ctrl Pts',(-16.9635965792169,-50.9750621818571,
-37.0550340359302));
#26258=CARTESIAN_POINT('Ctrl Pts',(-17.5236343382981,-47.9904963150807,
-36.8970855127378));
#26259=CARTESIAN_POINT('Ctrl Pts',(-20.3289175188232,-46.8278863119923,
-36.7391369895453));
#26260=CARTESIAN_POINT('Ctrl Pts',(-22.8359811930086,-48.5413353199386,
-36.5811884663528));
#26261=CARTESIAN_POINT('Ctrl Pts',(-22.77174696975,-51.5773112272049,-36.4232399431604));
#26262=CARTESIAN_POINT('Ctrl Pts',(-20.1944540690039,-53.1831870179292,
-36.2652914199679));
#26263=CARTESIAN_POINT('Ctrl Pts',(-17.4408555773868,-51.9029639510444,
-36.1073428967755));
#26264=CARTESIAN_POINT('Ctrl Pts',(-17.0075555011744,-48.8973813461366,
-35.949394373583));
#26265=CARTESIAN_POINT('Ctrl Pts',(-19.2874138408208,-46.8915095398771,
-35.7914458503905));
#26266=CARTESIAN_POINT('Ctrl Pts',(-22.2133523787375,-47.7040114934373,
-35.633497327198));
#26267=CARTESIAN_POINT('Ctrl Pts',(-23.1325116308869,-50.5982163965188,
-35.4755488040056));
#26268=CARTESIAN_POINT('Ctrl Pts',(-21.2115178583638,-52.9500366868287,
-35.3176002808131));
#26269=CARTESIAN_POINT('Ctrl Pts',(-18.1920776903032,-52.6271484344897,
-35.1596517576206));
#26270=CARTESIAN_POINT('Ctrl Pts',(-16.8118256949778,-49.9223045977125,
-35.0017032344282));
#26271=CARTESIAN_POINT('Ctrl Pts',(-18.3221943780753,-47.2879048191876,
-34.8437547112357));
#26272=CARTESIAN_POINT('Ctrl Pts',(-21.3537783904218,-47.1124792564605,
-34.6858061880432));
#26273=CARTESIAN_POINT('Ctrl Pts',(-23.1579327094808,-49.5550809319264,
-34.5278576648508));
#26274=CARTESIAN_POINT('Ctrl Pts',(-22.0988854850357,-52.4010771948131,
-34.3699091416583));
#26275=CARTESIAN_POINT('Ctrl Pts',(-19.136842626025,-53.0700897906246,-34.2119606184658));
#26276=CARTESIAN_POINT('Ctrl Pts',(-16.9573983062527,-50.955545345837,-34.0540120952733));
#26277=CARTESIAN_POINT('Ctrl Pts',(-17.5365884056535,-47.9746369975769,
-33.8960635720809));
#26278=CARTESIAN_POINT('Ctrl Pts',(-20.3492788763714,-46.8300636849827,
-33.7381150488884));
#26279=CARTESIAN_POINT('Ctrl Pts',(-22.8452888127201,-48.5595752199596,
-33.5801665256959));
#26280=CARTESIAN_POINT('Ctrl Pts',(-22.7615619181231,-51.5950760944598,
-33.4222180025035));
#26281=CARTESIAN_POINT('Ctrl Pts',(-20.1740108214729,-53.1843699861598,
-33.264269479311));
#26282=CARTESIAN_POINT('Ctrl Pts',(-17.4286894052932,-51.8864924596438,
-33.1063209561186));
#26283=CARTESIAN_POINT('Ctrl Pts',(-17.0146971024574,-48.8781895950435,
-32.9483724329261));
#26284=CARTESIAN_POINT('Ctrl Pts',(-19.3073881429401,-46.886998106296,-32.7904239097336));
#26285=CARTESIAN_POINT('Ctrl Pts',(-22.2280492893816,-47.7182707568971,
-32.6324753865411));
#26286=CARTESIAN_POINT('Ctrl Pts',(-23.1286059081968,-50.6183179165617,
-32.4745268633487));
#26287=CARTESIAN_POINT('Ctrl Pts',(-21.1925507022974,-52.9577550265691,
-32.3165783401562));
#26288=CARTESIAN_POINT('Ctrl Pts',(-18.1752460444151,-52.6154856100391,
-32.1586298169637));
#26289=CARTESIAN_POINT('Ctrl Pts',(-16.8123903006787,-49.9018349372858,
-32.0006812937713));
#26290=CARTESIAN_POINT('Ctrl Pts',(-18.3396433245503,-47.2771875413399,
-31.8427327705788));
#26291=CARTESIAN_POINT('Ctrl Pts',(-21.3722912485865,-47.1212313910636,
-31.6847842473863));
#26292=CARTESIAN_POINT('Ctrl Pts',(-23.160724433881,-49.5753671847204,-31.5268357241938));
#26293=CARTESIAN_POINT('Ctrl Pts',(-22.0834249040639,-52.414504637368,-31.3688872010014));
#26294=CARTESIAN_POINT('Ctrl Pts',(-19.1171473782361,-53.0644841691531,
-31.2109386778089));
#26295=CARTESIAN_POINT('Ctrl Pts',(-16.951325473813,-50.9359891068399,-31.0529901546164));
#26296=CARTESIAN_POINT('Ctrl Pts',(-17.5496440410392,-47.9588611881771,
-30.895041631424));
#26297=CARTESIAN_POINT('Ctrl Pts',(-20.3696258320475,-46.8323717517629,
-30.7370931082315));
#26298=CARTESIAN_POINT('Ctrl Pts',(-22.8544791227998,-48.5778745089676,
-30.5791445850391));
#26299=CARTESIAN_POINT('Ctrl Pts',(-22.7512630079677,-51.6127751968989,
-30.4211960618466));
#26300=CARTESIAN_POINT('Ctrl Pts',(-20.1535603996932,-53.1854216641434,
-30.2632475386541));
#26301=CARTESIAN_POINT('Ctrl Pts',(-17.4166292473454,-51.8699431887277,
-30.1052990154616));
#26302=CARTESIAN_POINT('Ctrl Pts',(-17.0219617867595,-48.8590440958476,
-29.9473504922692));
#26303=CARTESIAN_POINT('Ctrl Pts',(-19.3273910011813,-46.8826150206499,
-29.7894019690767));
#26304=CARTESIAN_POINT('Ctrl Pts',(-22.242654338353,-47.7326240952651,-29.6314534458843));
#26305=CARTESIAN_POINT('Ctrl Pts',(-23.1245711941905,-50.6383939435537,
-29.4735049226917));
#26306=CARTESIAN_POINT('Ctrl Pts',(-21.1735343777889,-52.9653514191537,
-29.3155563994993));
#26307=CARTESIAN_POINT('Ctrl Pts',(-18.1584896324882,-52.6037149499794,
-29.1576078763068));
#26308=CARTESIAN_POINT('Ctrl Pts',(-16.8130863303897,-49.8813693242968,
-28.9996593531144));
#26309=CARTESIAN_POINT('Ctrl Pts',(-18.3571607269583,-47.2665825238328,
-28.8417108299219));
#26310=CARTESIAN_POINT('Ctrl Pts',(-21.3907475276376,-47.1301022167759,
-28.6837623067294));
#26311=CARTESIAN_POINT('Ctrl Pts',(-23.163385842798,-49.5956709439795,-28.525813783537));
#26312=CARTESIAN_POINT('Ctrl Pts',(-22.067878424094,-52.4278325327341,-28.3678652603445));
#26313=CARTESIAN_POINT('Ctrl Pts',(-19.0974885304027,-53.0587521961423,
-28.209916737152));
#26314=CARTESIAN_POINT('Ctrl Pts',(-16.9453783366354,-50.9163942851932,
-28.0519682139596));
#26315=CARTESIAN_POINT('Ctrl Pts',(-17.5628007047423,-47.943169518583,-27.8940196907671));
#26316=CARTESIAN_POINT('Ctrl Pts',(-20.3899575461711,-46.8348104498304,
-27.7360711675746));
#26317=CARTESIAN_POINT('Ctrl Pts',(-22.8635517477194,-48.5962323698076,
-27.5781226443821));
#26318=CARTESIAN_POINT('Ctrl Pts',(-22.7408506562487,-51.6304079283914,
-27.4201741211897));
#26319=CARTESIAN_POINT('Ctrl Pts',(-20.1331036625272,-53.1863417630947,
-27.2622255979972));
#26320=CARTESIAN_POINT('Ctrl Pts',(-17.4046755693,-51.8533173088245,-27.1042770748047));
#26321=CARTESIAN_POINT('Ctrl Pts',(-17.0293493173344,-48.8399446663136,
-26.9463285516123));
#26322=CARTESIAN_POINT('Ctrl Pts',(-19.3474214658271,-46.8783623974773,
-26.7883800284198));
#26323=CARTESIAN_POINT('Ctrl Pts',(-22.2571671723368,-47.7470670676456,
-26.6304315052273));
#26324=CARTESIAN_POINT('Ctrl Pts',(-23.1204071598918,-50.6584513111502,
-26.4724829820349));
#26325=CARTESIAN_POINT('Ctrl Pts',(-21.1544706547953,-52.972810301925,-26.3145344588424));
#26326=CARTESIAN_POINT('Ctrl Pts',(-18.141807182972,-52.5918672926414,-26.1565859356499));
#26327=CARTESIAN_POINT('Ctrl Pts',(-16.8139176614472,-49.8608481868135,
-25.9986374124575));
#26328=CARTESIAN_POINT('Ctrl Pts',(-18.3747380885828,-47.2562104579471,
-25.840688889265));
#26329=CARTESIAN_POINT('Ctrl Pts',(-21.4091619384342,-47.1388520028128,
-25.6827403660725));
#26330=CARTESIAN_POINT('Ctrl Pts',(-23.1658860660886,-49.6164679066119,
-25.5247918428801));
#26331=CARTESIAN_POINT('Ctrl Pts',(-22.0523074696332,-52.4401106361917,
-25.3668433196876));
#26332=CARTESIAN_POINT('Ctrl Pts',(-19.077751646914,-53.0547995573753,-25.2088947964951));
#26333=CARTESIAN_POINT('Ctrl Pts',(-16.9397224709031,-50.8927861603057,
-25.0509462733027));
#26334=CARTESIAN_POINT('Ctrl Pts',(-17.3646313374448,-48.923161141752,-24.945647257841));
#26335=CARTESIAN_POINT('Ctrl Pts',(-17.9456684496579,-48.2435746787732,
-24.8929977501102));
#26336=CARTESIAN_POINT('Ctrl Pts',(-19.3498000020249,-52.4320868020351,
-40.3210067496694));
#26337=CARTESIAN_POINT('Ctrl Pts',(-18.5452496035378,-52.2169963426693,
-40.2683572419386));
#26338=CARTESIAN_POINT('Ctrl Pts',(-17.1799170762945,-50.9293076251419,
-40.163058226477));
#26339=CARTESIAN_POINT('Ctrl Pts',(-17.680374294889,-48.1417352316521,-40.0051097032845));
#26340=CARTESIAN_POINT('Ctrl Pts',(-20.2879335437864,-47.0441888636839,
-39.847161180092));
#26341=CARTESIAN_POINT('Ctrl Pts',(-22.632464572945,-48.6240732572535,-39.6892126568995));
#26342=CARTESIAN_POINT('Ctrl Pts',(-22.591206612308,-51.4527232351918,-39.5312641337071));
#26343=CARTESIAN_POINT('Ctrl Pts',(-20.2000849223071,-52.9636035245707,
-39.3733156105146));
#26344=CARTESIAN_POINT('Ctrl Pts',(-17.6278012479644,-51.7877909526211,
-39.2153670873221));
#26345=CARTESIAN_POINT('Ctrl Pts',(-17.2061929729734,-48.9908837806426,
-39.0574185641297));
#26346=CARTESIAN_POINT('Ctrl Pts',(-19.3177073910386,-47.1089914337183,
-38.8994700409372));
#26347=CARTESIAN_POINT('Ctrl Pts',(-22.0478041999406,-47.8482485160203,
-38.7415215177447));
#26348=CARTESIAN_POINT('Ctrl Pts',(-22.9212350811254,-50.538453378564,-38.5835729945523));
#26349=CARTESIAN_POINT('Ctrl Pts',(-21.1460629918798,-52.7404488145126,
-38.4256244713598));
#26350=CARTESIAN_POINT('Ctrl Pts',(-18.3317944468367,-52.4577677439425,
-38.2676759481673));
#26351=CARTESIAN_POINT('Ctrl Pts',(-17.0300351295434,-49.946700854034,-38.1097274249748));
#26352=CARTESIAN_POINT('Ctrl Pts',(-18.4210536432903,-47.4839599626605,
-37.9517789017824));
#26353=CARTESIAN_POINT('Ctrl Pts',(-21.2436542895572,-47.3024354062046,
-37.7938303785899));
#26354=CARTESIAN_POINT('Ctrl Pts',(-22.938671670551,-49.5667109482944,-37.6358818553975));
#26355=CARTESIAN_POINT('Ctrl Pts',(-21.9692846953855,-52.2238363328611,
-37.477933332205));
#26356=CARTESIAN_POINT('Ctrl Pts',(-19.2144072443732,-52.8646770311455,
-37.3199848090126));
#26357=CARTESIAN_POINT('Ctrl Pts',(-17.1718028198231,-50.9082021494081,
-37.1620362858201));
#26358=CARTESIAN_POINT('Ctrl Pts',(-17.6934387790586,-48.1282880211688,
-37.0040877626276));
#26359=CARTESIAN_POINT('Ctrl Pts',(-20.30636363827,-47.0453982082162,-36.8461392394351));
#26360=CARTESIAN_POINT('Ctrl Pts',(-22.6415179083921,-48.6413559849339,
-36.6881907162427));
#26361=CARTESIAN_POINT('Ctrl Pts',(-22.5816882270502,-51.4691549662039,
-36.5302421930502));
#26362=CARTESIAN_POINT('Ctrl Pts',(-20.1811203497752,-52.9649158232608,
-36.3722936698577));
#26363=CARTESIAN_POINT('Ctrl Pts',(-17.6163361593653,-51.7724776765447,
-36.2143451466653));
#26364=CARTESIAN_POINT('Ctrl Pts',(-17.2127474776616,-48.9729879283094,
-36.0563966234728));
#26365=CARTESIAN_POINT('Ctrl Pts',(-19.3362758873773,-47.1046587901488,
-35.8984481002803));
#26366=CARTESIAN_POINT('Ctrl Pts',(-22.0615827638175,-47.8614474692219,
-35.7404995770878));
#26367=CARTESIAN_POINT('Ctrl Pts',(-22.9177152484768,-50.5571966867741,
-35.5825510538954));
#26368=CARTESIAN_POINT('Ctrl Pts',(-21.1284440556567,-52.7477526148208,
-35.4246025307029));
#26369=CARTESIAN_POINT('Ctrl Pts',(-18.316046957639,-52.4470048161168,-35.2666540075105));
#26370=CARTESIAN_POINT('Ctrl Pts',(-17.0304388680174,-49.9276321729325,
-35.1087054843179));
#26371=CARTESIAN_POINT('Ctrl Pts',(-18.4372415416432,-47.4738732375796,
-34.9507569611255));
#26372=CARTESIAN_POINT('Ctrl Pts',(-21.2609497803121,-47.3104766090421,
-34.792808437933));
#26373=CARTESIAN_POINT('Ctrl Pts',(-22.9413932032255,-49.5855890409291,
-34.6348599147406));
#26374=CARTESIAN_POINT('Ctrl Pts',(-21.954964867205,-52.2364352856664,-34.4769113915481));
#26375=CARTESIAN_POINT('Ctrl Pts',(-19.1960293436584,-52.8595736749944,
-34.3189628683556));
#26376=CARTESIAN_POINT('Ctrl Pts',(-17.1660295625545,-50.890023583207,-34.1610143451632));
#26377=CARTESIAN_POINT('Ctrl Pts',(-17.7055045857678,-48.1135161773694,
-34.0030658219706));
#26378=CARTESIAN_POINT('Ctrl Pts',(-20.3253288171419,-47.0474262786991,
-33.8451172987783));
#26379=CARTESIAN_POINT('Ctrl Pts',(-22.6501873044421,-48.6583451746618,
-33.6871687755857));
#26380=CARTESIAN_POINT('Ctrl Pts',(-22.5722015646081,-51.4857016961716,
-33.5292202523933));
#26381=CARTESIAN_POINT('Ctrl Pts',(-20.1620788961182,-52.9660176753372,
-33.3712717292008));
#26382=CARTESIAN_POINT('Ctrl Pts',(-17.6050042219247,-51.7571356356244,
-33.2133232060083));
#26383=CARTESIAN_POINT('Ctrl Pts',(-17.2193993792082,-48.9551121559556,
-33.0553746828159));
#26384=CARTESIAN_POINT('Ctrl Pts',(-19.3548805512185,-47.1004567056546,
-32.8974261596234));
#26385=CARTESIAN_POINT('Ctrl Pts',(-22.0752719070179,-47.8747289747136,
-32.7394776364309));
#26386=CARTESIAN_POINT('Ctrl Pts',(-22.9140773412661,-50.5759198452034,
-32.5815291132385));
#26387=CARTESIAN_POINT('Ctrl Pts',(-21.1107774778443,-52.7549417078576,
-32.423580590046));
#26388=CARTESIAN_POINT('Ctrl Pts',(-18.3003694580311,-52.4361417117618,
-32.2656320668536));
#26389=CARTESIAN_POINT('Ctrl Pts',(-17.0309647586947,-49.9085661175126,
-32.107683543661));
#26390=CARTESIAN_POINT('Ctrl Pts',(-18.4534940135249,-47.4638908436788,
-31.9497350204686));
#26391=CARTESIAN_POINT('Ctrl Pts',(-21.2781932114386,-47.3186286096082,
-31.7917864972761));
#26392=CARTESIAN_POINT('Ctrl Pts',(-22.9439934990302,-49.6044842649813,
-31.6338379740836));
#26393=CARTESIAN_POINT('Ctrl Pts',(-21.940564418566,-52.2489420082286,-31.4758894508913));
#26394=CARTESIAN_POINT('Ctrl Pts',(-19.1776845993869,-52.8543524310943,
-31.3179409276987));
#26395=CARTESIAN_POINT('Ctrl Pts',(-17.1603731443513,-50.8718083158917,
-31.1599924045063));
#26396=CARTESIAN_POINT('Ctrl Pts',(-17.7176649959856,-48.0988221155217,
-31.0020438813138));
#26397=CARTESIAN_POINT('Ctrl Pts',(-20.3442805816783,-47.0495760812962,
-30.8440953581213));
#26398=CARTESIAN_POINT('Ctrl Pts',(-22.658747434784,-48.6753896810726,-30.6861468349289));
#26399=CARTESIAN_POINT('Ctrl Pts',(-22.5626088509189,-51.5021871708183,
-30.5281983117364));
#26400=CARTESIAN_POINT('Ctrl Pts',(-20.1430307601508,-52.9669972397414,
-30.3702497885439));
#26401=CARTESIAN_POINT('Ctrl Pts',(-17.5937710292379,-51.7417211485313,
-30.2123012653515));
#26402=CARTESIAN_POINT('Ctrl Pts',(-17.2261659239688,-48.9372794640055,
-30.054352742159));
#26403=CARTESIAN_POINT('Ctrl Pts',(-19.3735118130877,-47.0963741682751,
-29.8964042189665));
#26404=CARTESIAN_POINT('Ctrl Pts',(-22.0888754875022,-47.8880981043954,
-29.7384556957741));
#26405=CARTESIAN_POINT('Ctrl Pts',(-22.9103192876763,-50.5946192586408,
-29.5805071725816));
#26406=CARTESIAN_POINT('Ctrl Pts',(-21.0930651030709,-52.7620172156573,
-29.4225586493891));
#26407=CARTESIAN_POINT('Ctrl Pts',(-18.2847620335903,-52.4251781660874,
-29.2646101261966));
#26408=CARTESIAN_POINT('Ctrl Pts',(-17.0316130616351,-49.8895038319974,
-29.1066616030042));
#26409=CARTESIAN_POINT('Ctrl Pts',(-18.4698102473148,-47.454013012425,-28.9487130798117));
#26410=CARTESIAN_POINT('Ctrl Pts',(-21.2953839430823,-47.3268911626317,
-28.7907645566192));
#26411=CARTESIAN_POINT('Ctrl Pts',(-22.9464724150868,-49.6233957950799,
-28.6328160334268));
#26412=CARTESIAN_POINT('Ctrl Pts',(-21.9260839610248,-52.2613560095547,
-28.4748675102343));
#26413=CARTESIAN_POINT('Ctrl Pts',(-19.1593737591251,-52.8490134995825,
-28.3169189870418));
#26414=CARTESIAN_POINT('Ctrl Pts',(-17.1548338024837,-50.85355711154,-28.1589704638494));
#26415=CARTESIAN_POINT('Ctrl Pts',(-17.729919507007,-48.0842064240116,-28.0010219406569));
#26416=CARTESIAN_POINT('Ctrl Pts',(-20.3632181497758,-47.0518475577905,
-27.8430734174644));
#26417=CARTESIAN_POINT('Ctrl Pts',(-22.6671979496393,-48.692488743044,-27.685124894272));
#26418=CARTESIAN_POINT('Ctrl Pts',(-22.5529104743563,-51.5186108255752,
-27.5271763710795));
#26419=CARTESIAN_POINT('Ctrl Pts',(-20.1239767418433,-52.9678542474899,
-27.369227847887));
#26420=CARTESIAN_POINT('Ctrl Pts',(-17.5826370151246,-51.7262353055309,
-27.2112793246945));
#26421=CARTESIAN_POINT('Ctrl Pts',(-17.233046891431,-48.9194896827197,-27.0533308015021));
#26422=CARTESIAN_POINT('Ctrl Pts',(-19.3921687883899,-47.0924131475548,
-26.8953822783096));
#26423=CARTESIAN_POINT('Ctrl Pts',(-22.1023931761822,-47.9015507218836,
-26.7374337551172));
#26424=CARTESIAN_POINT('Ctrl Pts',(-22.9064407812892,-50.6133012921579,
-26.5794852319247));
#26425=CARTESIAN_POINT('Ctrl Pts',(-21.0753085799274,-52.7689646426944,
-26.4215367087322));
#26426=CARTESIAN_POINT('Ctrl Pts',(-18.2692234999564,-52.4141429028396,
-26.2635881855398));
#26427=CARTESIAN_POINT('Ctrl Pts',(-17.0323873883061,-49.8703898293036,
-26.1056396623473));
#26428=CARTESIAN_POINT('Ctrl Pts',(-18.4861823289167,-47.4443521592953,
-25.9476911391548));
#26429=CARTESIAN_POINT('Ctrl Pts',(-21.3125356773786,-47.3350409756728,
-25.7897426159623));
#26430=CARTESIAN_POINT('Ctrl Pts',(-22.9488011980187,-49.6427667095871,
-25.6317940927699));
#26431=CARTESIAN_POINT('Ctrl Pts',(-21.9115807072091,-52.2727922032235,
-25.4738455695774));
#26432=CARTESIAN_POINT('Ctrl Pts',(-19.1409902341146,-52.8453318933313,
-25.3158970463849));
#26433=CARTESIAN_POINT('Ctrl Pts',(-17.1495657595727,-50.8315677962272,
-25.1579485231925));
#26434=CARTESIAN_POINT('Ctrl Pts',(-17.5453386170133,-48.9970000028466,
-25.0526495077308));
#26435=CARTESIAN_POINT('Ctrl Pts',(-18.0865340033349,-48.3640127966251,
-25.));
#26436=CARTESIAN_POINT('Ctrl Pts',(-17.4850545138796,-49.9982392692185,
-39.112583302492));
#26437=CARTESIAN_POINT('Ctrl Pts',(-17.4831412917956,-49.7066909038706,
-39.0941950563712));
#26438=CARTESIAN_POINT('Ctrl Pts',(-17.5300112989184,-49.4157373800817,
-39.0758068102505));
#26439=CARTESIAN_POINT('Ctrl Pts',(-17.6283800884828,-49.143386251485,-39.0574185641297));
#26440=CARTESIAN_POINT('Ctrl Pts',(-17.9100311123284,-48.3635863316678,
-39.0047690563989));
#26441=CARTESIAN_POINT('Ctrl Pts',(-18.6138692516835,-47.736288882693,-38.9521195486681));
#26442=CARTESIAN_POINT('Ctrl Pts',(-19.420804456178,-47.5458496719227,-38.8994700409372));
#26443=CARTESIAN_POINT('Ctrl Pts',(-20.2277396606726,-47.3554104611523,
-38.8468205332064));
#26444=CARTESIAN_POINT('Ctrl Pts',(-21.1377719303066,-47.6018294885863,
-38.7941710254756));
#26445=CARTESIAN_POINT('Ctrl Pts',(-21.7383598786544,-48.1734064793939,
-38.7415215177447));
#26446=CARTESIAN_POINT('Ctrl Pts',(-22.3389478270022,-48.7449834702016,
-38.6888720100139));
#26447=CARTESIAN_POINT('Ctrl Pts',(-22.6300914540638,-49.6417184243828,
-38.6362225022831));
#26448=CARTESIAN_POINT('Ctrl Pts',(-22.4798012527203,-50.4570851407982,
-38.5835729945523));
#26449=CARTESIAN_POINT('Ctrl Pts',(-22.3295110513769,-51.2724518572135,
-38.5309234868215));
#26450=CARTESIAN_POINT('Ctrl Pts',(-21.7377870216284,-52.0064503358631,
-38.4782739790906));
#26451=CARTESIAN_POINT('Ctrl Pts',(-20.9728802492469,-52.3263360634262,
-38.4256244713598));
#26452=CARTESIAN_POINT('Ctrl Pts',(-20.2079734768655,-52.6462217909892,
-38.372974963629));
#26453=CARTESIAN_POINT('Ctrl Pts',(-19.2698839618511,-52.5519947674658,
-38.3203254558982));
#26454=CARTESIAN_POINT('Ctrl Pts',(-18.5838793181283,-52.0863701073861,
-38.2676759481673));
#26455=CARTESIAN_POINT('Ctrl Pts',(-17.9102783689704,-51.6291644370585,
-38.2159783996089));
#26456=CARTESIAN_POINT('Ctrl Pts',(-17.4797287780335,-50.813870240662,-38.1642808510504));
#26457=CARTESIAN_POINT('Ctrl Pts',(-17.4784634893366,-49.9997267145485,
-38.112583302492));
#26458=CARTESIAN_POINT('Origin',(-20.,-50.,-32.));
#26459=CARTESIAN_POINT('Origin',(-20.,50.,-25.));
#26460=CARTESIAN_POINT('Ctrl Pts',(-18.0865340033349,51.6359872033749,-25.));
#26461=CARTESIAN_POINT('Ctrl Pts',(-18.0243833228338,51.5775808249506,-25.));
#26462=CARTESIAN_POINT('Ctrl Pts',(-17.9656072042478,51.5159215542002,-25.));
#26463=CARTESIAN_POINT('Ctrl Pts',(-17.9102180900498,51.4513856299869,-25.));
#26464=CARTESIAN_POINT('Ctrl Pts',(-17.8534757442914,51.3852730051767,-25.));
#26465=CARTESIAN_POINT('Ctrl Pts',(-17.8002874537736,51.3161409574413,-25.));
#26466=CARTESIAN_POINT('Ctrl Pts',(-17.7506954746655,51.2443477068885,-25.));
#26467=CARTESIAN_POINT('Ctrl Pts',(-17.7377283789557,51.2255755189666,-25.));
#26468=CARTESIAN_POINT('Ctrl Pts',(-17.7250073328008,51.2066211684088,-25.));
#26469=CARTESIAN_POINT('Ctrl Pts',(-17.712533469509,51.1874906231763,-25.));
#26470=CARTESIAN_POINT('Ctrl Pts',(-17.7024059324163,51.1719585220211,-25.));
#26471=CARTESIAN_POINT('Ctrl Pts',(-17.6924409292295,51.156309427101,-25.));
#26472=CARTESIAN_POINT('Ctrl Pts',(-17.682647813279,51.1405609613993,-25.));
#26473=CARTESIAN_POINT('Ctrl Pts',(-17.6351885166707,51.0642409108008,-25.));
#26474=CARTESIAN_POINT('Ctrl Pts',(-17.5917126522887,50.9855142151719,-25.));
#26475=CARTESIAN_POINT('Ctrl Pts',(-17.5522554123681,50.9047730795493,-25.));
#26476=CARTESIAN_POINT('Ctrl Pts',(-17.5204203008065,50.8396290637662,-25.));
#26477=CARTESIAN_POINT('Ctrl Pts',(-17.4912016837347,50.7731726244963,-25.));
#26478=CARTESIAN_POINT('Ctrl Pts',(-17.4646351938,50.7055919593486,-25.));
#26479=CARTESIAN_POINT('Ctrl Pts',(-17.4539844043915,50.6784981492764,-25.));
#26480=CARTESIAN_POINT('Ctrl Pts',(-17.4437600743761,50.6512234901344,-25.));
#26481=CARTESIAN_POINT('Ctrl Pts',(-17.4339652711491,50.6237795558022,-25.));
#26482=CARTESIAN_POINT('Ctrl Pts',(-17.4287336556888,50.6091211591182,-25.));
#26483=CARTESIAN_POINT('Ctrl Pts',(-17.4236250235962,50.5944154772993,-25.));
#26484=CARTESIAN_POINT('Ctrl Pts',(-17.41864375021,50.5796764952228,-25.));
#26485=CARTESIAN_POINT('Ctrl Pts',(-17.3890989440111,50.4922570072194,-25.));
#26486=CARTESIAN_POINT('Ctrl Pts',(-17.3639908537199,50.4035567266403,-25.));
#26487=CARTESIAN_POINT('Ctrl Pts',(-17.3433526020187,50.3139730842995,-25.));
#26488=CARTESIAN_POINT('Ctrl Pts',(-17.322396152995,50.223008255434,-25.));
#26489=CARTESIAN_POINT('Ctrl Pts',(-17.3060479349661,50.131131810167,-25.));
#26490=CARTESIAN_POINT('Ctrl Pts',(-17.2943844478798,50.0387266921583,-25.));
#26491=CARTESIAN_POINT('Ctrl Pts',(-17.2828125669698,49.9470473330473,-25.));
#26492=CARTESIAN_POINT('Ctrl Pts',(-17.2758517728664,49.8548466441588,-25.));
#26493=CARTESIAN_POINT('Ctrl Pts',(-17.2736237166568,49.7624794304333,-25.));
#26494=CARTESIAN_POINT('Ctrl Pts',(-17.2725154991996,49.7165367121665,-25.));
#26495=CARTESIAN_POINT('Ctrl Pts',(-17.2725789187574,49.6705525832056,-25.));
#26496=CARTESIAN_POINT('Ctrl Pts',(-17.2738337345407,49.6245700069453,-25.));
#26497=CARTESIAN_POINT('Ctrl Pts',(-17.2742445582872,49.6095154192502,-25.));
#26498=CARTESIAN_POINT('Ctrl Pts',(-17.2747831814028,49.5944594880405,-25.));
#26499=CARTESIAN_POINT('Ctrl Pts',(-17.2754501651331,49.5794084218269,-25.));
#26500=CARTESIAN_POINT('Ctrl Pts',(-17.2796911524576,49.483706865494,-25.));
#26501=CARTESIAN_POINT('Ctrl Pts',(-17.2891006969591,49.3885698423273,-25.));
#26502=CARTESIAN_POINT('Ctrl Pts',(-17.3037432826356,49.294395309891,-25.));
#26503=CARTESIAN_POINT('Ctrl Pts',(-17.3078992671603,49.2676658846328,-25.));
#26504=CARTESIAN_POINT('Ctrl Pts',(-17.3124771127594,49.2410138657042,-25.));
#26505=CARTESIAN_POINT('Ctrl Pts',(-17.3174790132619,49.2144480906985,-25.));
#26506=CARTESIAN_POINT('Ctrl Pts',(-17.3344212204447,49.1244657202194,-25.));
#26507=CARTESIAN_POINT('Ctrl Pts',(-17.3562243822145,49.0354729310092,-25.));
#26508=CARTESIAN_POINT('Ctrl Pts',(-17.3825856673629,48.9477022722757,-25.));
#26509=CARTESIAN_POINT('Ctrl Pts',(-17.4095441942202,48.8579430800576,-25.));
#26510=CARTESIAN_POINT('Ctrl Pts',(-17.441269931108,48.7694613223897,-25.));
#26511=CARTESIAN_POINT('Ctrl Pts',(-17.4774932435503,48.6825093747115,-25.));
#26512=CARTESIAN_POINT('Ctrl Pts',(-17.4899698857142,48.6525599232811,-25.));
#26513=CARTESIAN_POINT('Ctrl Pts',(-17.5029805545828,48.6227920442769,-25.));
#26514=CARTESIAN_POINT('Ctrl Pts',(-17.516515599114,48.59321638808,-25.));
#26515=CARTESIAN_POINT('Ctrl Pts',(-17.5231913782271,48.5786290295058,-25.));
#26516=CARTESIAN_POINT('Ctrl Pts',(-17.529994731303,48.5640884359945,-25.));
#26517=CARTESIAN_POINT('Ctrl Pts',(-17.5369245591161,48.5495959077351,-25.));
#26518=CARTESIAN_POINT('Ctrl Pts',(-17.5430261062936,48.5368355842061,-25.));
#26519=CARTESIAN_POINT('Ctrl Pts',(-17.5492249412562,48.5241142478127,-25.));
#26520=CARTESIAN_POINT('Ctrl Pts',(-17.5555148617866,48.5114432513385,-25.));
#26521=CARTESIAN_POINT('Ctrl Pts',(-17.5983742533158,48.425103337132,-25.));
#26522=CARTESIAN_POINT('Ctrl Pts',(-17.6455227691097,48.3409647245588,-25.));
#26523=CARTESIAN_POINT('Ctrl Pts',(-17.6966178449534,48.2592776638004,-25.));
#26524=CARTESIAN_POINT('Ctrl Pts',(-17.7487226127291,48.175976381616,-25.));
#26525=CARTESIAN_POINT('Ctrl Pts',(-17.8049317736166,48.0952237256181,-25.));
#26526=CARTESIAN_POINT('Ctrl Pts',(-17.8649370191223,48.0172922419165,-25.));
#26527=CARTESIAN_POINT('Ctrl Pts',(-17.9254206661132,47.9387394369082,-25.));
#26528=CARTESIAN_POINT('Ctrl Pts',(-17.989761629997,47.8630521302711,-25.));
#26529=CARTESIAN_POINT('Ctrl Pts',(-18.0576934095421,47.7905288730113,-25.));
#26530=CARTESIAN_POINT('Ctrl Pts',(-18.0946392725352,47.7510858561423,-25.));
#26531=CARTESIAN_POINT('Ctrl Pts',(-18.1326480797102,47.7125791482251,-25.));
#26532=CARTESIAN_POINT('Ctrl Pts',(-18.1716822386029,47.6750605369461,-25.));
#26533=CARTESIAN_POINT('Ctrl Pts',(-18.1843390275069,47.6628951629147,-25.));
#26534=CARTESIAN_POINT('Ctrl Pts',(-18.1971036460433,47.6508336993754,-25.));
#26535=CARTESIAN_POINT('Ctrl Pts',(-18.2099748874407,47.638877986089,-25.));
#26536=CARTESIAN_POINT('Ctrl Pts',(-18.2214598785455,47.6282099194662,-25.));
#26537=CARTESIAN_POINT('Ctrl Pts',(-18.2330243829329,47.6176310982102,-25.));
#26538=CARTESIAN_POINT('Ctrl Pts',(-18.2446619767169,47.6071472907025,-25.));
#26539=CARTESIAN_POINT('Ctrl Pts',(-18.3204767947681,47.5388489832147,-25.));
#26540=CARTESIAN_POINT('Ctrl Pts',(-18.3994577938915,47.4745180356072,-25.));
#26541=CARTESIAN_POINT('Ctrl Pts',(-18.4812785962965,47.4144375027462,-25.));
#26542=CARTESIAN_POINT('Ctrl Pts',(-18.5631717960198,47.3543038089612,-25.));
#26543=CARTESIAN_POINT('Ctrl Pts',(-18.6479104038285,47.2984272169749,-25.));
#26544=CARTESIAN_POINT('Ctrl Pts',(-18.7352121444042,47.2471177279551,-25.));
#26545=CARTESIAN_POINT('Ctrl Pts',(-18.820751629926,47.1968439617712,-25.));
#26546=CARTESIAN_POINT('Ctrl Pts',(-18.9087524795439,47.1509541033334,-25.));
#26547=CARTESIAN_POINT('Ctrl Pts',(-18.998982921958,47.1097758970613,-25.));
#26548=CARTESIAN_POINT('Ctrl Pts',(-19.0364028378792,47.092698678162,-25.));
#26549=CARTESIAN_POINT('Ctrl Pts',(-19.0742065683153,47.0764323013347,-25.));
#26550=CARTESIAN_POINT('Ctrl Pts',(-19.1123789307588,47.0610024423687,-25.));
#26551=CARTESIAN_POINT('Ctrl Pts',(-19.142800661846,47.0487055084058,-25.));
#26552=CARTESIAN_POINT('Ctrl Pts',(-19.1734565434277,47.0369399116326,-25.));
#26553=CARTESIAN_POINT('Ctrl Pts',(-19.2043343151472,47.0257029622097,-25.));
#26554=CARTESIAN_POINT('Ctrl Pts',(-20.7937992825329,47.0307770462543,-25.));
#26555=CARTESIAN_POINT('Ctrl Pts',(-20.8886442187745,47.065471747601,-25.));
#26556=CARTESIAN_POINT('Ctrl Pts',(-20.9814460889928,47.1051547823912,-25.));
#26557=CARTESIAN_POINT('Ctrl Pts',(-21.0719637631512,47.1495064254641,-25.));
#26558=CARTESIAN_POINT('Ctrl Pts',(-21.163746553324,47.1944779471897,-25.));
#26559=CARTESIAN_POINT('Ctrl Pts',(-21.253181519704,47.2442501915546,-25.));
#26560=CARTESIAN_POINT('Ctrl Pts',(-21.3399832517889,47.2985305082219,-25.));
#26561=CARTESIAN_POINT('Ctrl Pts',(-21.3644994122972,47.3138613653821,-25.));
#26562=CARTESIAN_POINT('Ctrl Pts',(-21.3888052755545,47.3295520482463,-25.));
#26563=CARTESIAN_POINT('Ctrl Pts',(-21.4128938145509,47.3455964190897,-25.));
#26564=CARTESIAN_POINT('Ctrl Pts',(-21.4322113128632,47.3584629987829,-25.));
#26565=CARTESIAN_POINT('Ctrl Pts',(-21.4513911411419,47.3715586534343,-25.));
#26566=CARTESIAN_POINT('Ctrl Pts',(-21.470410419303,47.3848664771592,-25.));
#26567=CARTESIAN_POINT('Ctrl Pts',(-21.5531190276758,47.4427378417522,-25.));
#26568=CARTESIAN_POINT('Ctrl Pts',(-21.6328730469962,47.5046694738537,-25.));
#26569=CARTESIAN_POINT('Ctrl Pts',(-21.7094059959913,47.5703647549773,-25.));
#26570=CARTESIAN_POINT('Ctrl Pts',(-21.7684006486615,47.6210053005573,-25.));
#26571=CARTESIAN_POINT('Ctrl Pts',(-21.8254807251055,47.6738830950808,-25.));
#26572=CARTESIAN_POINT('Ctrl Pts',(-21.880506602648,47.7288740485728,-25.));
#26573=CARTESIAN_POINT('Ctrl Pts',(-21.9097988741256,47.758147728711,-25.));
#26574=CARTESIAN_POINT('Ctrl Pts',(-21.9385087463308,47.7880203887706,-25.));
#26575=CARTESIAN_POINT('Ctrl Pts',(-21.9666131342303,47.8184741413986,-25.));
#26576=CARTESIAN_POINT('Ctrl Pts',(-21.9762497481644,47.8289163206757,-25.));
#26577=CARTESIAN_POINT('Ctrl Pts',(-21.9858144352345,47.8394261052524,-25.));
#26578=CARTESIAN_POINT('Ctrl Pts',(-21.9952996346009,47.8499951701003,-25.));
#26579=CARTESIAN_POINT('Ctrl Pts',(-22.0610978805005,47.9233121243291,-25.));
#26580=CARTESIAN_POINT('Ctrl Pts',(-22.1231640295475,47.999575563378,-25.));
#26581=CARTESIAN_POINT('Ctrl Pts',(-22.1812542057559,48.0785076415563,-25.));
#26582=CARTESIAN_POINT('Ctrl Pts',(-22.2388179901799,48.1567244663097,-25.));
#26583=CARTESIAN_POINT('Ctrl Pts',(-22.2924779669419,48.2375625681601,-25.));
#26584=CARTESIAN_POINT('Ctrl Pts',(-22.3419510864935,48.3207739812286,-25.));
#26585=CARTESIAN_POINT('Ctrl Pts',(-22.3900084462906,48.4016041543266,-25.));
#26586=CARTESIAN_POINT('Ctrl Pts',(-22.4341153568532,48.48467444732,-25.));
#26587=CARTESIAN_POINT('Ctrl Pts',(-22.4739645960461,48.5697679270184,-25.));
#26588=CARTESIAN_POINT('Ctrl Pts',(-22.4947696783231,48.6141947939351,-25.));
#26589=CARTESIAN_POINT('Ctrl Pts',(-22.514413373569,48.6591732571786,-25.));
#26590=CARTESIAN_POINT('Ctrl Pts',(-22.5328462651431,48.7046726841286,-25.));
#26591=CARTESIAN_POINT('Ctrl Pts',(-22.5399053146425,48.7220971183659,-25.));
#26592=CARTESIAN_POINT('Ctrl Pts',(-22.5467867474585,48.7395979548892,-25.));
#26593=CARTESIAN_POINT('Ctrl Pts',(-22.5534876260568,48.7571734646438,-25.));
#26594=CARTESIAN_POINT('Ctrl Pts',(-22.5587290601633,48.770921046385,-25.));
#26595=CARTESIAN_POINT('Ctrl Pts',(-22.5638601218329,48.7847148146814,-25.));
#26596=CARTESIAN_POINT('Ctrl Pts',(-22.5688742772034,48.7985392343856,-25.));
#26597=CARTESIAN_POINT('Ctrl Pts',(-22.6005567102338,48.8858901876576,-25.));
#26598=CARTESIAN_POINT('Ctrl Pts',(-22.6276303371176,48.9746044552164,-25.));
#26599=CARTESIAN_POINT('Ctrl Pts',(-22.6498438368096,49.064459151712,-25.));
#26600=CARTESIAN_POINT('Ctrl Pts',(-22.6548287054449,49.0846231900001,-25.));
#26601=CARTESIAN_POINT('Ctrl Pts',(-22.6595686217097,49.1048446984201,-25.));
#26602=CARTESIAN_POINT('Ctrl Pts',(-22.664060384471,49.1251212139915,-25.));
#26603=CARTESIAN_POINT('Ctrl Pts',(-22.6844252492069,49.2170513801367,-25.));
#26604=CARTESIAN_POINT('Ctrl Pts',(-22.699693338023,49.3101125654953,-25.));
#26605=CARTESIAN_POINT('Ctrl Pts',(-22.7099745886613,49.4039125916329,-25.));
#26606=CARTESIAN_POINT('Ctrl Pts',(-22.7207065136441,49.5018243028922,-25.));
#26607=CARTESIAN_POINT('Ctrl Pts',(-22.726004813639,49.6005422870379,-25.));
#26608=CARTESIAN_POINT('Ctrl Pts',(-22.7259370635773,49.6996058630434,-25.));
#26609=CARTESIAN_POINT('Ctrl Pts',(-22.7259105623628,49.7383557181929,-25.));
#26610=CARTESIAN_POINT('Ctrl Pts',(-22.7250624171289,49.777158194654,-25.));
#26611=CARTESIAN_POINT('Ctrl Pts',(-22.7233944482762,49.8159844929349,-25.));
#26612=CARTESIAN_POINT('Ctrl Pts',(-22.7228610319112,49.8284011414003,-25.));
#26613=CARTESIAN_POINT('Ctrl Pts',(-22.7222437741598,49.8408189143377,-25.));
#26614=CARTESIAN_POINT('Ctrl Pts',(-22.7215434366001,49.8532272016926,-25.));
#26615=CARTESIAN_POINT('Ctrl Pts',(-22.7163011026353,49.9461086776959,-25.));
#26616=CARTESIAN_POINT('Ctrl Pts',(-22.7064019888496,50.0386086524861,-25.));
#26617=CARTESIAN_POINT('Ctrl Pts',(-22.6919696691014,50.130354953021,-25.));
#26618=CARTESIAN_POINT('Ctrl Pts',(-22.6775715542487,50.221883812931,-25.));
#26619=CARTESIAN_POINT('Ctrl Pts',(-22.6586612853047,50.3126635132626,-25.));
#26620=CARTESIAN_POINT('Ctrl Pts',(-22.6353128834832,50.4023075767819,-25.));
#26621=CARTESIAN_POINT('Ctrl Pts',(-22.6123616726036,50.4904266618342,-25.));
#26622=CARTESIAN_POINT('Ctrl Pts',(-22.5851215750556,50.5774492051802,-25.));
#26623=CARTESIAN_POINT('Ctrl Pts',(-22.5536224664953,50.6629790188289,-25.));
#26624=CARTESIAN_POINT('Ctrl Pts',(-22.5377791649532,50.7059984784396,-25.));
#26625=CARTESIAN_POINT('Ctrl Pts',(-22.5208577985189,50.748639764913,-25.));
#26626=CARTESIAN_POINT('Ctrl Pts',(-22.5028587517058,50.7908486725183,-25.));
#26627=CARTESIAN_POINT('Ctrl Pts',(-22.4972963290681,50.8038929067832,-25.));
#26628=CARTESIAN_POINT('Ctrl Pts',(-22.4916309664074,50.8168958257194,-25.));
#26629=CARTESIAN_POINT('Ctrl Pts',(-22.4858626342927,50.8298557719296,-25.));
#26630=CARTESIAN_POINT('Ctrl Pts',(-22.4801786518254,50.8426262063587,-25.));
#26631=CARTESIAN_POINT('Ctrl Pts',(-22.4743981603631,50.8553470721618,-25.));
#26632=CARTESIAN_POINT('Ctrl Pts',(-22.4685229752345,50.8680138234556,-25.));
#26633=CARTESIAN_POINT('Ctrl Pts',(-22.4310412018688,50.9488235836377,-25.));
#26634=CARTESIAN_POINT('Ctrl Pts',(-22.3896896687866,51.0274761880601,-25.));
#26635=CARTESIAN_POINT('Ctrl Pts',(-22.3445381491691,51.1036235513123,-25.));
#26636=CARTESIAN_POINT('Ctrl Pts',(-22.3001458590794,51.1784904853093,-25.));
#26637=CARTESIAN_POINT('Ctrl Pts',(-22.2520798483092,51.2509363917474,-25.));
#26638=CARTESIAN_POINT('Ctrl Pts',(-22.2003702290622,51.320596267752,-25.));
#26639=CARTESIAN_POINT('Ctrl Pts',(-22.1502407921192,51.3881274237048,-25.));
#26640=CARTESIAN_POINT('Ctrl Pts',(-22.0966865895448,51.4530406640365,-25.));
#26641=CARTESIAN_POINT('Ctrl Pts',(-22.0397073639147,51.5149631456524,-25.));
#26642=CARTESIAN_POINT('Ctrl Pts',(-22.0187240959256,51.5377668256239,-25.));
#26643=CARTESIAN_POINT('Ctrl Pts',(-21.9972760930074,51.5601644736352,-25.));
#26644=CARTESIAN_POINT('Ctrl Pts',(-21.975362529417,51.5821358538774,-25.));
#26645=CARTESIAN_POINT('Ctrl Pts',(-21.9562846701964,51.6012640480396,-25.));
#26646=CARTESIAN_POINT('Ctrl Pts',(-21.9368539244304,51.6200691348985,-25.));
#26647=CARTESIAN_POINT('Ctrl Pts',(-21.9170804273993,51.6385459961512,-25.));
#26648=CARTESIAN_POINT('Origin',(-20.,50.,-42.2084234471774));
#26649=CARTESIAN_POINT('Ctrl Pts',(-16.9232550353076,50.0019104925463,-39.7084234471775));
#26650=CARTESIAN_POINT('Ctrl Pts',(-16.9223298998565,50.1251796275816,-39.7020198504182));
#26651=CARTESIAN_POINT('Ctrl Pts',(-16.9848354680816,51.261038906527,-39.642966745928));
#26652=CARTESIAN_POINT('Ctrl Pts',(-18.3975849010801,53.2535258762515,-39.5312641337071));
#26653=CARTESIAN_POINT('Ctrl Pts',(-21.848150909044,53.1200739456119,-39.3733156105146));
#26654=CARTESIAN_POINT('Ctrl Pts',(-23.6230224069675,50.158234898072,-39.2153670873222));
#26655=CARTESIAN_POINT('Ctrl Pts',(-22.1130258952668,47.0526834926192,-39.0574185641297));
#26656=CARTESIAN_POINT('Ctrl Pts',(-18.6872049245772,46.6194976592071,-38.8994700409372));
#26657=CARTESIAN_POINT('Ctrl Pts',(-17.0406885958919,48.5578258148839,-38.7831383352865));
#26658=CARTESIAN_POINT('Ctrl Pts',(-16.9238131547401,49.7844436293797,-38.7194561373665));
#26659=CARTESIAN_POINT('Ctrl Pts',(-16.9257449470869,49.9973154802779,-38.7084234471774));
#26660=CARTESIAN_POINT('Ctrl Pts',(-16.9296933173407,49.9966552073599,-39.7915765528225));
#26661=CARTESIAN_POINT('Ctrl Pts',(-16.9347030447108,50.6897748401454,-39.7557520197534));
#26662=CARTESIAN_POINT('Ctrl Pts',(-17.5071823782537,52.4114026146138,-39.6672779789534));
#26663=CARTESIAN_POINT('Ctrl Pts',(-20.3515248609294,53.6086146806686,-39.5261544304226));
#26664=CARTESIAN_POINT('Ctrl Pts',(-23.2138551423641,51.6798054402274,-39.3682059072301));
#26665=CARTESIAN_POINT('Ctrl Pts',(-23.1634851378897,48.2264371018949,-39.2102573840377));
#26666=CARTESIAN_POINT('Ctrl Pts',(-20.2442745178934,46.3818724340551,-39.0523088608451));
#26667=CARTESIAN_POINT('Ctrl Pts',(-17.4694924470354,47.6502488635873,-38.9127485837735));
#26668=CARTESIAN_POINT('Ctrl Pts',(-16.9339705689346,49.3389604585216,-38.8258378144326));
#26669=CARTESIAN_POINT('Ctrl Pts',(-16.9296185387977,50.0021495995983,-38.7915765528225));
#26670=CARTESIAN_POINT('Ctrl Pts',(-21.913465996665,51.635987203375,-40.));
#26671=CARTESIAN_POINT('Ctrl Pts',(-22.4546613829867,51.0029999971535,-39.9473504922692));
#26672=CARTESIAN_POINT('Ctrl Pts',(-22.8504293341544,49.1684270296901,-39.8420514768075));
#26673=CARTESIAN_POINT('Ctrl Pts',(-20.8590122687702,47.1546700385836,-39.6841029536151));
#26674=CARTESIAN_POINT('Ctrl Pts',(-18.0884177969373,47.7272058248279,-39.5261544304226));
#26675=CARTESIAN_POINT('Ctrl Pts',(-17.051198789188,50.3572343043579,-39.3682059072301));
#26676=CARTESIAN_POINT('Ctrl Pts',(-18.6874637997297,52.6649589697292,-39.2102573840377));
#26677=CARTESIAN_POINT('Ctrl Pts',(-21.5138180945235,52.5556486605102,-39.0523088608452));
#26678=CARTESIAN_POINT('Ctrl Pts',(-22.9676131151914,50.1296100067989,-38.8943603376527));
#26679=CARTESIAN_POINT('Ctrl Pts',(-21.7307768639447,47.5858567407415,-38.7364118144603));
#26680=CARTESIAN_POINT('Ctrl Pts',(-18.9246911981855,47.231034767221,-38.5784632912678));
#26681=CARTESIAN_POINT('Ctrl Pts',(-17.0935586692445,49.3866986229546,-38.4205147680753));
#26682=CARTESIAN_POINT('Ctrl Pts',(-17.897606416995,52.0984496625164,-38.2625662448829));
#26683=CARTESIAN_POINT('Ctrl Pts',(-20.6078313299859,52.90758741957,-38.1046177216903));
#26684=CARTESIAN_POINT('Ctrl Pts',(-22.7669536381063,51.0805105191678,-37.9466691984979));
#26685=CARTESIAN_POINT('Ctrl Pts',(-22.4173634487422,48.2737643663635,-37.7887206753054));
#26686=CARTESIAN_POINT('Ctrl Pts',(-19.8760232341734,47.032145182041,-37.630772152113));
#26687=CARTESIAN_POINT('Ctrl Pts',(-17.4470890363398,48.4813888841037,-37.4728236289205));
#26688=CARTESIAN_POINT('Ctrl Pts',(-17.3328015389901,51.3075115071856,-37.3148751057281));
#26689=CARTESIAN_POINT('Ctrl Pts',(-19.6367817806179,52.9481530076165,-37.1569265825355));
#26690=CARTESIAN_POINT('Ctrl Pts',(-22.2700809281698,51.9157939431384,-36.9989780593431));
#26691=CARTESIAN_POINT('Ctrl Pts',(-22.845166742959,49.146442724891,-36.8410295361506));
#26692=CARTESIAN_POINT('Ctrl Pts',(-20.8406264020256,47.1509859542099,-36.6830810129582));
#26693=CARTESIAN_POINT('Ctrl Pts',(-18.0739156697339,47.7386435569461,-36.5251324897657));
#26694=CARTESIAN_POINT('Ctrl Pts',(-17.0535270200547,50.3766042771083,-36.3671839665732));
#26695=CARTESIAN_POINT('Ctrl Pts',(-18.7046158085844,52.6731093498251,-36.2092354433807));
#26696=CARTESIAN_POINT('Ctrl Pts',(-21.5301900460322,52.5459874756549,-36.0512869201883));
#26697=CARTESIAN_POINT('Ctrl Pts',(-22.9683875074239,50.1104961891868,-35.8933383969958));
#26698=CARTESIAN_POINT('Ctrl Pts',(-21.7152382952319,47.5748213689897,-35.7353898738034));
#26699=CARTESIAN_POINT('Ctrl Pts',(-18.9069346873816,47.2379822548464,-35.5774413506109));
#26700=CARTESIAN_POINT('Ctrl Pts',(-17.0896801543967,49.4053806273666,-35.4194928274185));
#26701=CARTESIAN_POINT('Ctrl Pts',(-17.9111241120468,52.1119023004698,-35.2615443042259));
#26702=CARTESIAN_POINT('Ctrl Pts',(-20.626488307014,52.9036263883688,-35.1035957810335));
#26703=CARTESIAN_POINT('Ctrl Pts',(-22.7738346077931,51.062720739725,-34.945647257841));
#26704=CARTESIAN_POINT('Ctrl Pts',(-22.4062294320517,48.2582785175696,-34.7876987346486));
#26705=CARTESIAN_POINT('Ctrl Pts',(-19.8569692124294,47.033002191466,-34.6297502114561));
#26706=CARTESIAN_POINT('Ctrl Pts',(-17.4373906578124,48.4978125412028,-34.4718016882636));
#26707=CARTESIAN_POINT('Ctrl Pts',(-17.341252055517,51.3246105728636,-34.3138531650711));
#26708=CARTESIAN_POINT('Ctrl Pts',(-19.6557193523207,52.9504244843191,-34.1559046418787));
#26709=CARTESIAN_POINT('Ctrl Pts',(-22.2823354415527,51.9011782489466,-33.9979561186862));
#26710=CARTESIAN_POINT('Ctrl Pts',(-22.8396274000236,49.128191516977,-33.8400075954937));
#26711=CARTESIAN_POINT('Ctrl Pts',(-20.8223155582564,47.1456470217079,-33.6820590723012));
#26712=CARTESIAN_POINT('Ctrl Pts',(-18.0594352094154,47.7510575606347,-33.5241105491088));
#26713=CARTESIAN_POINT('Ctrl Pts',(-17.0560059365872,50.3955158108414,-33.3661620259163));
#26714=CARTESIAN_POINT('Ctrl Pts',(-18.7218065435234,52.681371904428,-33.2082135027239));
#26715=CARTESIAN_POINT('Ctrl Pts',(-21.5465062829502,52.5361096425097,-33.0502649795314));
#26716=CARTESIAN_POINT('Ctrl Pts',(-22.9690358104885,50.091433900016,-32.8923164563389));
#26717=CARTESIAN_POINT('Ctrl Pts',(-21.6996308677992,47.5638578212141,-32.7343679331465));
#26718=CARTESIAN_POINT('Ctrl Pts',(-18.8892223092125,47.2450577640023,-32.576419409954));
#26719=CARTESIAN_POINT('Ctrl Pts',(-17.0859221000865,49.424080044389,-32.4184708867615));
#26720=CARTESIAN_POINT('Ctrl Pts',(-17.924727695139,52.1252714327145,-32.2605223635691));
#26721=CARTESIAN_POINT('Ctrl Pts',(-20.645119572455,52.8995438502066,-32.1025738403766));
#26722=CARTESIAN_POINT('Ctrl Pts',(-22.7806011538509,51.0448880443562,-31.9446253171841));
#26723=CARTESIAN_POINT('Ctrl Pts',(-22.3949962372115,48.2428640275214,-31.7866767939916));
#26724=CARTESIAN_POINT('Ctrl Pts',(-19.8379210728103,47.033981756058,-31.6287282707992));
#26725=CARTESIAN_POINT('Ctrl Pts',(-17.4277979422843,48.5142980190097,-31.4707797476067));
#26726=CARTESIAN_POINT('Ctrl Pts',(-17.3498121874998,51.341655082542,-31.3128312244142));
#26727=CARTESIAN_POINT('Ctrl Pts',(-19.6746711204904,52.9525742873284,-31.1548827012218));
#26728=CARTESIAN_POINT('Ctrl Pts',(-22.2944958541018,51.8864841842817,-30.9969341780293));
#26729=CARTESIAN_POINT('Ctrl Pts',(-22.8339709807359,49.1099762461699,-30.8389856548368));
#26730=CARTESIAN_POINT('Ctrl Pts',(-20.8039708104681,47.1404257768069,-30.6810371316443));
#26731=CARTESIAN_POINT('Ctrl Pts',(-18.0450347580157,47.7635642855944,-30.5230886084519));
#26732=CARTESIAN_POINT('Ctrl Pts',(-17.0586062328904,50.4144110385161,-30.3651400852594));
#26733=CARTESIAN_POINT('Ctrl Pts',(-18.7390499779557,52.6895239065569,-30.207191562067));
#26734=CARTESIAN_POINT('Ctrl Pts',(-21.5627587579476,52.5261272466952,-30.0492430388745));
#26735=CARTESIAN_POINT('Ctrl Pts',(-22.9695617012666,50.072367840941,-29.891294515682));
#26736=CARTESIAN_POINT('Ctrl Pts',(-21.6839533651858,47.5529947147765,-29.7333459924895));
#26737=CARTESIAN_POINT('Ctrl Pts',(-18.8715557280134,47.2522468584174,-29.5753974692971));
#26738=CARTESIAN_POINT('Ctrl Pts',(-17.0822841921784,49.4428032064075,-29.4174489461046));
#26739=CARTESIAN_POINT('Ctrl Pts',(-17.9384168409638,52.1385529407526,-29.2595004229121));
#26740=CARTESIAN_POINT('Ctrl Pts',(-20.6637242398626,52.8953417649065,-29.1015518997197));
#26741=CARTESIAN_POINT('Ctrl Pts',(-22.787253056673,51.0270122685761,-28.9436033765272));
#26742=CARTESIAN_POINT('Ctrl Pts',(-22.3836642975977,48.2275219836588,-28.7856548533347));
#26743=CARTESIAN_POINT('Ctrl Pts',(-19.8188796155043,47.0350836083479,-28.6277063301423));
#26744=CARTESIAN_POINT('Ctrl Pts',(-17.4183112780211,48.5308447521454,-28.4697578069498));
#26745=CARTESIAN_POINT('Ctrl Pts',(-17.3584815852165,51.3586442755348,-28.3118092837573));
#26746=CARTESIAN_POINT('Ctrl Pts',(-19.6936363029893,52.9546023581848,-28.1538607605649));
#26747=CARTESIAN_POINT('Ctrl Pts',(-22.3065616631405,51.8717123376796,-27.9959122373724));
#26748=CARTESIAN_POINT('Ctrl Pts',(-22.8281977223296,49.0917976764282,-27.8379637141799));
#26749=CARTESIAN_POINT('Ctrl Pts',(-20.785592906288,47.1353224197833,-27.6800151909875));
#26750=CARTESIAN_POINT('Ctrl Pts',(-18.0307149269819,47.7761632406137,-27.522066667795));
#26751=CARTESIAN_POINT('Ctrl Pts',(-17.0613277662871,50.4332891351524,-27.3641181446025));
#26752=CARTESIAN_POINT('Ctrl Pts',(-18.7563454716562,52.6975651102113,-27.2061696214101));
#26753=CARTESIAN_POINT('Ctrl Pts',(-21.5789466600823,52.5160405210495,-27.0482210982176));
#26754=CARTESIAN_POINT('Ctrl Pts',(-22.9699654385827,50.0532991536051,-26.8902725750251));
#26755=CARTESIAN_POINT('Ctrl Pts',(-21.6682058751988,47.5422317897299,-26.7323240518326));
#26756=CARTESIAN_POINT('Ctrl Pts',(-18.853936784431,47.2595506510657,-26.5743755286402));
#26757=CARTESIAN_POINT('Ctrl Pts',(-17.0787643658711,49.4615465350924,-26.4164270054477));
#26758=CARTESIAN_POINT('Ctrl Pts',(-17.9521953953268,52.151751865176,-26.2584784822553));
#26759=CARTESIAN_POINT('Ctrl Pts',(-20.682292760352,52.8910091782576,-26.1005299590628));
#26760=CARTESIAN_POINT('Ctrl Pts',(-22.7938075288087,51.0091163069545,-25.9425814358703));
#26761=CARTESIAN_POINT('Ctrl Pts',(-22.3721992598072,48.2122088972454,-25.7846329126778));
#26762=CARTESIAN_POINT('Ctrl Pts',(-19.7999149622792,47.0363955599718,-25.6266843894854));
#26763=CARTESIAN_POINT('Ctrl Pts',(-17.4087929877025,48.5472771059899,-25.4687358662929));
#26764=CARTESIAN_POINT('Ctrl Pts',(-17.3675348421714,51.3759259143989,-25.3107873431005));
#26765=CARTESIAN_POINT('Ctrl Pts',(-19.7120663404711,52.9558136087163,-25.1528388199079));
#26766=CARTESIAN_POINT('Ctrl Pts',(-22.3196266734264,51.8582617585154,-24.9948902967155));
#26767=CARTESIAN_POINT('Ctrl Pts',(-22.8200818112517,49.0706994179464,-24.836941773523));
#26768=CARTESIAN_POINT('Ctrl Pts',(-21.4547503964622,47.7830036573307,-24.7316427580614));
#26769=CARTESIAN_POINT('Ctrl Pts',(-20.6501999979751,47.5679131979649,-24.6789932503306));
#26770=CARTESIAN_POINT('Ctrl Pts',(-22.0543315503421,51.7564253212269,-40.1070022498898));
#26771=CARTESIAN_POINT('Ctrl Pts',(-22.6353686625551,51.0768388582481,-40.054352742159));
#26772=CARTESIAN_POINT('Ctrl Pts',(-23.060272261634,49.107208284706,-39.9490537266973));
#26773=CARTESIAN_POINT('Ctrl Pts',(-20.9222510402281,46.9452025167633,-39.7911052035049));
#26774=CARTESIAN_POINT('Ctrl Pts',(-17.9476909243915,47.5598872466888,-39.6331566803124));
#26775=CARTESIAN_POINT('Ctrl Pts',(-16.8341139201763,50.3835331819777,-39.47520815712));
#26776=CARTESIAN_POINT('Ctrl Pts',(-18.5908375001798,52.86114793857,-39.3172596339274));
#26777=CARTESIAN_POINT('Ctrl Pts',(-21.6252623660303,52.7437904222108,-39.159311110735));
#26778=CARTESIAN_POINT('Ctrl Pts',(-23.1860828791167,50.1391516372232,-39.0013625875425));
#26779=CARTESIAN_POINT('Ctrl Pts',(-21.8581932077187,47.4081323247007,-38.84341406435));
#26780=CARTESIAN_POINT('Ctrl Pts',(-18.8455291069827,47.0271890645498,-38.6854655411576));
#26781=CARTESIAN_POINT('Ctrl Pts',(-16.8795922501912,49.341548597713,-38.5275170179651));
#26782=CARTESIAN_POINT('Ctrl Pts',(-17.742832390891,52.2529333450532,-38.3695684947727));
#26783=CARTESIAN_POINT('Ctrl Pts',(-20.6525786612632,53.121638211398,-38.2116199715802));
#26784=CARTESIAN_POINT('Ctrl Pts',(-22.9706512511864,51.1600555504364,-38.0536714483877));
#26785=CARTESIAN_POINT('Ctrl Pts',(-22.5953249287157,48.1466823389155,-37.8957229251952));
#26786=CARTESIAN_POINT('Ctrl Pts',(-19.866896311724,46.8136576244393,-37.7377744020028));
#26787=CARTESIAN_POINT('Ctrl Pts',(-17.2591488184259,48.3695917599147,-37.5798258788103));
#26788=CARTESIAN_POINT('Ctrl Pts',(-17.136447703264,51.4037678988433,-37.4218773556179));
#26789=CARTESIAN_POINT('Ctrl Pts',(-19.6100423790983,53.1651901572008,-37.2639288324253));
#26790=CARTESIAN_POINT('Ctrl Pts',(-22.4371997624713,52.0568308755958,-37.1059803092329));
#26791=CARTESIAN_POINT('Ctrl Pts',(-23.0546222489617,49.0836055391962,-36.9480317860404));
#26792=CARTESIAN_POINT('Ctrl Pts',(-20.9025116426116,46.9412472174394,-36.790083262848));
#26793=CARTESIAN_POINT('Ctrl Pts',(-17.932121179482,47.5721670018534,-36.6321347396555));
#26794=CARTESIAN_POINT('Ctrl Pts',(-16.8366135507598,50.4043291335231,-36.4741862164631));
#26795=CARTESIAN_POINT('Ctrl Pts',(-18.6092522057474,52.8698983334071,-36.3162376932705));
#26796=CARTESIAN_POINT('Ctrl Pts',(-21.6428395879844,52.7334180001784,-36.1582891700781));
#26797=CARTESIAN_POINT('Ctrl Pts',(-23.1869142805623,50.118630698447,-36.0003406468856));
#26798=CARTESIAN_POINT('Ctrl Pts',(-21.8415107205413,47.396284550871,-35.8423921236932));
#26799=CARTESIAN_POINT('Ctrl Pts',(-18.8264653972371,47.0346480123697,-35.6844436005007));
#26800=CARTESIAN_POINT('Ctrl Pts',(-16.8754282068091,49.3616059340618,-35.5264950773083));
#26801=CARTESIAN_POINT('Ctrl Pts',(-17.7573452317156,52.2673763394054,-35.3685465541157));
#26802=CARTESIAN_POINT('Ctrl Pts',(-20.6726091277621,53.117385576973,-35.2105980309233));
#26803=CARTESIAN_POINT('Ctrl Pts',(-22.9780387841496,51.1409561228812,-35.0526495077308));
#26804=CARTESIAN_POINT('Ctrl Pts',(-22.5833712479035,48.1300564527922,-34.8947009845384));
#26805=CARTESIAN_POINT('Ctrl Pts',(-19.8464395708685,46.8145777251907,-34.7367524613459));
#26806=CARTESIAN_POINT('Ctrl Pts',(-17.2487364645975,48.3872244939215,-34.5788039381534));
#26807=CARTESIAN_POINT('Ctrl Pts',(-17.145520329978,51.422125763663,-34.4208554149609));
#26808=CARTESIAN_POINT('Ctrl Pts',(-19.6303740970927,53.1676288554917,-34.2629068917685));
#26809=CARTESIAN_POINT('Ctrl Pts',(-22.4503564287097,52.0411392031225,-34.104958368576));
#26810=CARTESIAN_POINT('Ctrl Pts',(-23.0486751106377,49.0640107137251,-33.9470098453835));
#26811=CARTESIAN_POINT('Ctrl Pts',(-20.8828527910125,46.9355152433656,-33.7890613221911));
#26812=CARTESIAN_POINT('Ctrl Pts',(-17.9165746965303,47.5854948997559,-33.6311127989986));
#26813=CARTESIAN_POINT('Ctrl Pts',(-16.8392749601877,50.4246328966843,-33.4731642758061));
#26814=CARTESIAN_POINT('Ctrl Pts',(-18.6277084883363,52.8787691608149,-33.3152157526137));
#26815=CARTESIAN_POINT('Ctrl Pts',(-21.6603569937506,52.7228129806409,-33.1572672294212));
#26816=CARTESIAN_POINT('Ctrl Pts',(-23.1876103104067,50.0981650815332,-32.9993187062287));
#26817=CARTESIAN_POINT('Ctrl Pts',(-21.8247543054021,47.3845138885554,-32.8413701830363));
#26818=CARTESIAN_POINT('Ctrl Pts',(-18.807449069083,47.0422444064101,-32.6834216598438));
#26819=CARTESIAN_POINT('Ctrl Pts',(-16.8713934920293,49.3816819649028,-32.5254731366513));
#26820=CARTESIAN_POINT('Ctrl Pts',(-17.7719502834869,52.2817296805251,-32.3675246134588));
#26821=CARTESIAN_POINT('Ctrl Pts',(-20.692611989838,53.1130024904866,-32.2095760902664));
#26822=CARTESIAN_POINT('Ctrl Pts',(-22.9853034698444,51.1218106200149,-32.0516275670739));
#26823=CARTESIAN_POINT('Ctrl Pts',(-22.5713110876437,48.1135071787034,-31.8936790438815));
#26824=CARTESIAN_POINT('Ctrl Pts',(-19.8259891451682,46.815629403376,-31.7357305206889));
#26825=CARTESIAN_POINT('Ctrl Pts',(-17.2384375524677,48.4049235997537,-31.5777819974966));
#26826=CARTESIAN_POINT('Ctrl Pts',(-17.1547106418195,51.440425056179,-31.419833474304));
#26827=CARTESIAN_POINT('Ctrl Pts',(-19.6507210566695,53.1699369227146,-31.2618849511116));
#26828=CARTESIAN_POINT('Ctrl Pts',(-22.4634120665983,52.0253633906983,-31.1039364279191));
#26829=CARTESIAN_POINT('Ctrl Pts',(-23.0426022770338,49.0444544709788,-30.9459879047267));
#26830=CARTESIAN_POINT('Ctrl Pts',(-20.8631575394479,46.9299096208195,-30.7880393815342));
#26831=CARTESIAN_POINT('Ctrl Pts',(-17.9011141125945,47.5989223448847,-30.6300908583417));
#26832=CARTESIAN_POINT('Ctrl Pts',(-16.8420666851231,50.4449191533675,-30.4721423351493));
#26833=CARTESIAN_POINT('Ctrl Pts',(-18.6462213500501,52.8875212970958,-30.3141938119568));
#26834=CARTESIAN_POINT('Ctrl Pts',(-21.6778059435708,52.7120957007386,-30.1562452887643));
#26835=CARTESIAN_POINT('Ctrl Pts',(-23.1881749162158,50.0776954171824,-29.9982967655718));
#26836=CARTESIAN_POINT('Ctrl Pts',(-21.8079226562872,47.372851061869,-29.8403482423794));
#26837=CARTESIAN_POINT('Ctrl Pts',(-18.7884819093805,47.0499627476302,-29.6823997191869));
#26838=CARTESIAN_POINT('Ctrl Pts',(-16.8674877685903,49.4017834887991,-29.5244511959944));
#26839=CARTESIAN_POINT('Ctrl Pts',(-17.7866471969486,52.2959889467186,-29.366502672802));
#26840=CARTESIAN_POINT('Ctrl Pts',(-20.7125862957864,53.1084910560403,-29.2085541496095));
#26841=CARTESIAN_POINT('Ctrl Pts',(-22.9924450724969,51.1026188652432,-29.050605626417));
#26842=CARTESIAN_POINT('Ctrl Pts',(-22.559144913217,48.0970356841439,-28.8926571032246));
#26843=CARTESIAN_POINT('Ctrl Pts',(-19.8055458937194,46.8168123718357,-28.7347085800321));
#26844=CARTESIAN_POINT('Ctrl Pts',(-17.2282524988857,48.4226884704099,-28.5767600568396));
#26845=CARTESIAN_POINT('Ctrl Pts',(-17.1640182633205,51.4586649597053,-28.4188115336471));
#26846=CARTESIAN_POINT('Ctrl Pts',(-19.6710824181117,53.1721142961061,-28.2608630104547));
#26847=CARTESIAN_POINT('Ctrl Pts',(-22.4763661364548,52.0095040701854,-28.1029144872622));
#26848=CARTESIAN_POINT('Ctrl Pts',(-23.036404002848,49.0249376311576,-27.9449659640697));
#26849=CARTESIAN_POINT('Ctrl Pts',(-20.843426690584,46.9244305648213,-27.7870174408773));
#26850=CARTESIAN_POINT('Ctrl Pts',(-17.8857400841354,47.6124488098665,-27.6290689176848));
#26851=CARTESIAN_POINT('Ctrl Pts',(-16.8449885723852,50.4651870178593,-27.4711203944923));
#26852=CARTESIAN_POINT('Ctrl Pts',(-18.6647901035319,52.8961544781396,-27.3131718712999));
#26853=CARTESIAN_POINT('Ctrl Pts',(-21.6951855668027,52.7012664104508,-27.1552233481074));
#26854=CARTESIAN_POINT('Ctrl Pts',(-23.1886083758687,50.0572229310833,-26.9972748249149));
#26855=CARTESIAN_POINT('Ctrl Pts',(-21.7910158674676,47.3612957917279,-26.8393263017225));
#26856=CARTESIAN_POINT('Ctrl Pts',(-18.7695658942812,47.057804230939,-26.68137777853));
#26857=CARTESIAN_POINT('Ctrl Pts',(-16.8637088196843,49.4219066639916,-26.5234292553375));
#26858=CARTESIAN_POINT('Ctrl Pts',(-17.8014401010271,52.3101595496564,-26.3654807321451));
#26859=CARTESIAN_POINT('Ctrl Pts',(-20.7325217937523,53.1038395129959,-26.2075322089526));
#26860=CARTESIAN_POINT('Ctrl Pts',(-22.9994820718101,51.0834054385887,-26.0495836857601));
#26861=CARTESIAN_POINT('Ctrl Pts',(-22.5468358421909,48.0805952788235,-25.8916351625677));
#26862=CARTESIAN_POINT('Ctrl Pts',(-19.7851851005152,46.8182209067238,-25.7336866393752));
#26863=CARTESIAN_POINT('Ctrl Pts',(-17.2180334910011,48.4403305413994,-25.5757381161827));
#26864=CARTESIAN_POINT('Ctrl Pts',(-17.1737380030118,51.4772188383851,-25.4177895929903));
#26865=CARTESIAN_POINT('Ctrl Pts',(-19.6908692382271,53.173414716488,-25.2598410697978));
#26866=CARTESIAN_POINT('Ctrl Pts',(-22.4903929667631,51.9950632861863,-25.1018925466053));
#26867=CARTESIAN_POINT('Ctrl Pts',(-23.0276906145693,49.0022861609293,-24.9439440234128));
#26868=CARTESIAN_POINT('Ctrl Pts',(-21.561846221743,47.6197928044311,-24.8386450079512));
#26869=CARTESIAN_POINT('Ctrl Pts',(-20.698066426161,47.3888678140614,-24.7859955002204));
#26870=CARTESIAN_POINT('Ctrl Pts',(-22.1951971040191,51.8768634390788,-40.2140044997796));
#26871=CARTESIAN_POINT('Ctrl Pts',(-22.8160759421236,51.1506777193428,-40.1613549920488));
#26872=CARTESIAN_POINT('Ctrl Pts',(-23.2701151891136,49.0459895397219,-40.0560559765872));
#26873=CARTESIAN_POINT('Ctrl Pts',(-20.9854898116861,46.735734994943,-39.8981074533947));
#26874=CARTESIAN_POINT('Ctrl Pts',(-17.8069640518455,47.3925686685497,-39.7401589302022));
#26875=CARTESIAN_POINT('Ctrl Pts',(-16.6170290511645,50.4098320595973,-39.5822104070097));
#26876=CARTESIAN_POINT('Ctrl Pts',(-18.49421120063,53.0573369074108,-39.4242618838173));
#26877=CARTESIAN_POINT('Ctrl Pts',(-21.7367066375372,52.9319321839113,-39.2663133606248));
#26878=CARTESIAN_POINT('Ctrl Pts',(-23.4045526430421,50.1486932676477,-39.1083648374323));
#26879=CARTESIAN_POINT('Ctrl Pts',(-21.9856095514927,47.2304079086599,-38.9504163142399));
#26880=CARTESIAN_POINT('Ctrl Pts',(-18.76636701578,46.8233433618784,-38.7924677910474));
#26881=CARTESIAN_POINT('Ctrl Pts',(-16.6656258311379,49.2963985724715,-38.6345192678549));
#26882=CARTESIAN_POINT('Ctrl Pts',(-17.5880583647869,52.4074170275899,-38.4765707446625));
#26883=CARTESIAN_POINT('Ctrl Pts',(-20.6973259925406,53.3356890032261,-38.31862222147));
#26884=CARTESIAN_POINT('Ctrl Pts',(-23.1743488642664,51.2396005817052,-38.1606736982775));
#26885=CARTESIAN_POINT('Ctrl Pts',(-22.7732864086894,48.0196003114673,-38.002725175085));
#26886=CARTESIAN_POINT('Ctrl Pts',(-19.8577693892745,46.5951700668379,-37.8447766518926));
#26887=CARTESIAN_POINT('Ctrl Pts',(-17.0712086005119,48.2577946357256,-37.6868281287001));
#26888=CARTESIAN_POINT('Ctrl Pts',(-16.9400938675379,51.500024290501,-37.5288796055076));
#26889=CARTESIAN_POINT('Ctrl Pts',(-19.5833029775787,53.382227306785,-37.3709310823152));
#26890=CARTESIAN_POINT('Ctrl Pts',(-22.6043185967729,52.1978678080534,-37.2129825591227));
#26891=CARTESIAN_POINT('Ctrl Pts',(-23.2640777549644,49.0207683535012,-37.0550340359303));
#26892=CARTESIAN_POINT('Ctrl Pts',(-20.9643968831977,46.731508480669,-36.8970855127378));
#26893=CARTESIAN_POINT('Ctrl Pts',(-17.79032668923,47.4056904467606,-36.7391369895453));
#26894=CARTESIAN_POINT('Ctrl Pts',(-16.619700081465,50.4320539899379,-36.5811884663528));
#26895=CARTESIAN_POINT('Ctrl Pts',(-18.5138886029103,53.066687316989,-36.4232399431604));
#26896=CARTESIAN_POINT('Ctrl Pts',(-21.7554891299366,52.920848524702,-36.2652914199679));
#26897=CARTESIAN_POINT('Ctrl Pts',(-23.4054410537007,50.1267652077072,-36.1073428967755));
#26898=CARTESIAN_POINT('Ctrl Pts',(-21.9677831458506,47.2177477327522,-35.949394373583));
#26899=CARTESIAN_POINT('Ctrl Pts',(-18.7459961070927,46.831313769893,-35.7914458503905));
#26900=CARTESIAN_POINT('Ctrl Pts',(-16.6611762592215,49.317831240757,-35.6334973271981));
#26901=CARTESIAN_POINT('Ctrl Pts',(-17.6035663513843,52.4228503783411,-35.4755488040055));
#26902=CARTESIAN_POINT('Ctrl Pts',(-20.7187299485102,53.3311447655771,-35.3176002808131));
#26903=CARTESIAN_POINT('Ctrl Pts',(-23.1822429605062,51.2191915060373,-35.1596517576206));
#26904=CARTESIAN_POINT('Ctrl Pts',(-22.7605130637554,48.0018343880148,-35.0017032344282));
#26905=CARTESIAN_POINT('Ctrl Pts',(-19.8359099293075,46.5961532589153,-34.8437547112357));
#26906=CARTESIAN_POINT('Ctrl Pts',(-17.0600822713825,48.2766364466403,-34.6858061880432));
#26907=CARTESIAN_POINT('Ctrl Pts',(-16.9497886044391,51.5196409544624,-34.5278576648508));
#26908=CARTESIAN_POINT('Ctrl Pts',(-19.6050288418647,53.3848332266643,-34.3699091416583));
#26909=CARTESIAN_POINT('Ctrl Pts',(-22.6183774158668,52.1811001572986,-34.2119606184659));
#26910=CARTESIAN_POINT('Ctrl Pts',(-23.2577228212518,48.9998299104731,-34.0540120952733));
#26911=CARTESIAN_POINT('Ctrl Pts',(-20.9433900237686,46.7253834650232,-33.8960635720809));
#26912=CARTESIAN_POINT('Ctrl Pts',(-17.7737141836451,47.419932238877,-33.7381150488884));
#26913=CARTESIAN_POINT('Ctrl Pts',(-16.6225439837881,50.4537499825271,-33.580166525696));
#26914=CARTESIAN_POINT('Ctrl Pts',(-18.5336104331491,53.0761664172017,-33.4222180025035));
#26915=CARTESIAN_POINT('Ctrl Pts',(-21.7742077045511,52.909516318772,-33.264269479311));
#26916=CARTESIAN_POINT('Ctrl Pts',(-23.4061848103248,50.1048962630504,-33.1063209561185));
#26917=CARTESIAN_POINT('Ctrl Pts',(-21.9498777430051,47.2051699558967,-32.9483724329261));
#26918=CARTESIAN_POINT('Ctrl Pts',(-18.7256758289536,46.8394310488179,-32.7904239097336));
#26919=CARTESIAN_POINT('Ctrl Pts',(-16.6568648839721,49.3392838854165,-32.6324753865411));
#26920=CARTESIAN_POINT('Ctrl Pts',(-17.6191728718348,52.4381879283357,-32.4745268633487));
#26921=CARTESIAN_POINT('Ctrl Pts',(-20.7401044072209,53.3264611307666,-32.3165783401562));
#26922=CARTESIAN_POINT('Ctrl Pts',(-23.1900057858379,51.1987331956736,-32.1586298169638));
#26923=CARTESIAN_POINT('Ctrl Pts',(-22.747625938076,47.9841503298854,-32.0006812937712));
#26924=CARTESIAN_POINT('Ctrl Pts',(-19.814057217526,46.5972770506939,-31.8427327705788));
#26925=CARTESIAN_POINT('Ctrl Pts',(-17.0490771626511,48.2955491804977,-31.6847842473863));
#26926=CARTESIAN_POINT('Ctrl Pts',(-16.9596090961393,51.539195029816,-31.5268357241939));
#26927=CARTESIAN_POINT('Ctrl Pts',(-19.6267709928486,53.3872995581008,-31.3688872010014));
#26928=CARTESIAN_POINT('Ctrl Pts',(-22.6323282790949,52.1642425971148,-31.2109386778089));
#26929=CARTESIAN_POINT('Ctrl Pts',(-23.2512335733316,48.9789326957879,-31.0529901546164));
#26930=CARTESIAN_POINT('Ctrl Pts',(-20.9223442684278,46.719393464832,-30.895041631424));
#26931=CARTESIAN_POINT('Ctrl Pts',(-17.7571934671733,47.4342804041751,-30.7370931082315));
#26932=CARTESIAN_POINT('Ctrl Pts',(-16.6255271373557,50.4754272682189,-30.5791445850391));
#26933=CARTESIAN_POINT('Ctrl Pts',(-18.5533927221445,53.0855186876348,-30.4211960618465));
#26934=CARTESIAN_POINT('Ctrl Pts',(-21.7928531291939,52.898064154782,-30.2632475386541));
#26935=CARTESIAN_POINT('Ctrl Pts',(-23.4067881311651,50.0830229934237,-30.1052990154616));
#26936=CARTESIAN_POINT('Ctrl Pts',(-21.9318919473886,47.1927074089615,-29.9473504922692));
#26937=CARTESIAN_POINT('Ctrl Pts',(-18.7054080907476,46.8476786368431,-29.7894019690767));
#26938=CARTESIAN_POINT('Ctrl Pts',(-16.6526913450023,49.3607637711907,-29.6314534458842));
#26939=CARTESIAN_POINT('Ctrl Pts',(-17.6348775529335,52.4534249526847,-29.4735049226918));
#26940=CARTESIAN_POINT('Ctrl Pts',(-20.76144835171,53.3216403471741,-29.3155563994993));
#26941=CARTESIAN_POINT('Ctrl Pts',(-23.1976370883209,51.1782254619103,-29.1576078763068));
#26942=CARTESIAN_POINT('Ctrl Pts',(-22.7346255288362,47.9665493846291,-28.9996593531144));
#26943=CARTESIAN_POINT('Ctrl Pts',(-19.7922121719347,46.5985411353234,-28.8417108299219));
#26944=CARTESIAN_POINT('Ctrl Pts',(-17.0381937197502,48.3145321886744,-28.6837623067294));
#26945=CARTESIAN_POINT('Ctrl Pts',(-16.9695549414245,51.5586856438757,-28.525813783537));
#26946=CARTESIAN_POINT('Ctrl Pts',(-19.6485285332341,53.3896262340275,-28.3678652603445));
#26947=CARTESIAN_POINT('Ctrl Pts',(-22.6461706097691,52.1472958026912,-28.209916737152));
#26948=CARTESIAN_POINT('Ctrl Pts',(-23.2446102833664,48.9580775858871,-28.0519682139595));
#26949=CARTESIAN_POINT('Ctrl Pts',(-20.9012604748801,46.7135387098593,-27.8940196907671));
#26950=CARTESIAN_POINT('Ctrl Pts',(-17.7407652412889,47.4487343791192,-27.7360711675746));
#26951=CARTESIAN_POINT('Ctrl Pts',(-16.6286493784833,50.4970849005663,-27.5781226443822));
#26952=CARTESIAN_POINT('Ctrl Pts',(-18.5732347354075,53.0947438460678,-27.4201741211897));
#26953=CARTESIAN_POINT('Ctrl Pts',(-21.8114244735231,52.8864922998521,-27.2622255979972));
#26954=CARTESIAN_POINT('Ctrl Pts',(-23.4072513131546,50.0611467085616,-27.1042770748048));
#26955=CARTESIAN_POINT('Ctrl Pts',(-21.9138258597365,47.1803597937259,-26.9463285516123));
#26956=CARTESIAN_POINT('Ctrl Pts',(-18.6851950041314,46.8560578108122,-26.7883800284198));
#26957=CARTESIAN_POINT('Ctrl Pts',(-16.6486532734975,49.3822667928909,-26.6304315052273));
#26958=CARTESIAN_POINT('Ctrl Pts',(-17.6506848067274,52.4685672341367,-26.4724829820349));
#26959=CARTESIAN_POINT('Ctrl Pts',(-20.7827508271526,53.3166698477343,-26.3145344588424));
#26960=CARTESIAN_POINT('Ctrl Pts',(-23.2051566148114,51.1576945702228,-26.1565859356499));
#26961=CARTESIAN_POINT('Ctrl Pts',(-22.7214724245746,47.9489816604016,-25.9986374124575));
#26962=CARTESIAN_POINT('Ctrl Pts',(-19.7704552387511,46.6000462534758,-25.840688889265));
#26963=CARTESIAN_POINT('Ctrl Pts',(-17.0272739942997,48.3333839768089,-25.6827403660725));
#26964=CARTESIAN_POINT('Ctrl Pts',(-16.9799411638522,51.5785117623713,-25.5247918428801));
#26965=CARTESIAN_POINT('Ctrl Pts',(-19.6696721359831,53.3910158242598,-25.3668433196876));
#26966=CARTESIAN_POINT('Ctrl Pts',(-22.6611592600998,52.1318648138572,-25.2088947964951));
#26967=CARTESIAN_POINT('Ctrl Pts',(-23.2352994178868,48.9338729039122,-25.0509462733027));
#26968=CARTESIAN_POINT('Ctrl Pts',(-21.6689420470237,47.4565819515315,-24.945647257841));
#26969=CARTESIAN_POINT('Ctrl Pts',(-20.7459328543469,47.2098224301578,-24.8929977501102));
#26970=CARTESIAN_POINT('Ctrl Pts',(-22.3360626576961,51.9973015569307,-40.3210067496694));
#26971=CARTESIAN_POINT('Ctrl Pts',(-22.996783221692,51.2245165804374,-40.2683572419386));
#26972=CARTESIAN_POINT('Ctrl Pts',(-23.4799581165932,48.9847707947378,-40.163058226477));
#26973=CARTESIAN_POINT('Ctrl Pts',(-21.0487285831441,46.5262674731227,-40.0051097032845));
#26974=CARTESIAN_POINT('Ctrl Pts',(-17.6662371792997,47.2252500904106,-39.8471611800921));
#26975=CARTESIAN_POINT('Ctrl Pts',(-16.3999441821527,50.4361309372171,-39.6892126568996));
#26976=CARTESIAN_POINT('Ctrl Pts',(-18.3975849010801,53.2535258762515,-39.5312641337071));
#26977=CARTESIAN_POINT('Ctrl Pts',(-21.848150909044,53.1200739456119,-39.3733156105146));
#26978=CARTESIAN_POINT('Ctrl Pts',(-23.6230224069675,50.158234898072,-39.2153670873222));
#26979=CARTESIAN_POINT('Ctrl Pts',(-22.1130258952668,47.0526834926192,-39.0574185641297));
#26980=CARTESIAN_POINT('Ctrl Pts',(-18.6872049245772,46.6194976592071,-38.8994700409372));
#26981=CARTESIAN_POINT('Ctrl Pts',(-16.4516594120846,49.2512485472298,-38.7415215177447));
#26982=CARTESIAN_POINT('Ctrl Pts',(-17.4332843386828,52.5619007101268,-38.5835729945523));
#26983=CARTESIAN_POINT('Ctrl Pts',(-20.7420733238179,53.5497397950539,-38.4256244713598));
#26984=CARTESIAN_POINT('Ctrl Pts',(-23.3780464773465,51.3191456129741,-38.2676759481674));
#26985=CARTESIAN_POINT('Ctrl Pts',(-22.951247888663,47.8925182840191,-38.1097274249748));
#26986=CARTESIAN_POINT('Ctrl Pts',(-19.8486424668251,46.3766825092365,-37.9517789017824));
#26987=CARTESIAN_POINT('Ctrl Pts',(-16.883268382598,48.1459975115365,-37.7938303785899));
#26988=CARTESIAN_POINT('Ctrl Pts',(-16.7437400318118,51.5962806821587,-37.6358818553975));
#26989=CARTESIAN_POINT('Ctrl Pts',(-19.5565635760592,53.5992644563693,-37.477933332205));
#26990=CARTESIAN_POINT('Ctrl Pts',(-22.7714374310744,52.3389047405107,-37.3199848090126));
#26991=CARTESIAN_POINT('Ctrl Pts',(-23.4735332609671,48.9579311678064,-37.16203628582));
#26992=CARTESIAN_POINT('Ctrl Pts',(-21.0262821237837,46.5217697438983,-37.0040877626276));
#26993=CARTESIAN_POINT('Ctrl Pts',(-17.648532198978,47.239213891668,-36.8461392394351));
#26994=CARTESIAN_POINT('Ctrl Pts',(-16.4027866121701,50.4597788463525,-36.6881907162427));
#26995=CARTESIAN_POINT('Ctrl Pts',(-18.4185250000732,53.263476300571,-36.5302421930502));
#26996=CARTESIAN_POINT('Ctrl Pts',(-21.8681386718888,53.1082790492255,-36.3722936698577));
#26997=CARTESIAN_POINT('Ctrl Pts',(-23.6239678268391,50.1348997169674,-36.2143451466652));
#26998=CARTESIAN_POINT('Ctrl Pts',(-22.09405557116,47.0392109146336,-36.0563966234728));
#26999=CARTESIAN_POINT('Ctrl Pts',(-18.6655268169483,46.6279795274162,-35.8984481002803));
#27000=CARTESIAN_POINT('Ctrl Pts',(-16.4469243116338,49.2740565474523,-35.7404995770879));
#27001=CARTESIAN_POINT('Ctrl Pts',(-17.449787471053,52.5783244172767,-35.5825510538954));
#27002=CARTESIAN_POINT('Ctrl Pts',(-20.7648507692583,53.5449039541813,-35.4246025307029));
#27003=CARTESIAN_POINT('Ctrl Pts',(-23.3864471368627,51.2974268891935,-35.2666540075105));
#27004=CARTESIAN_POINT('Ctrl Pts',(-22.9376548796072,47.8736123232374,-35.108705484318));
#27005=CARTESIAN_POINT('Ctrl Pts',(-19.8253802877465,46.3777287926399,-34.9507569611255));
#27006=CARTESIAN_POINT('Ctrl Pts',(-16.8714280781675,48.1660483993591,-34.7928084379331));
#27007=CARTESIAN_POINT('Ctrl Pts',(-16.7540568789002,51.6171561452617,-34.6348599147406));
#27008=CARTESIAN_POINT('Ctrl Pts',(-19.5796835866367,53.602037597837,-34.4769113915481));
#27009=CARTESIAN_POINT('Ctrl Pts',(-22.7863984030238,52.3210611114746,-34.3189628683556));
#27010=CARTESIAN_POINT('Ctrl Pts',(-23.4667705318659,48.935649107221,-34.1610143451632));
#27011=CARTESIAN_POINT('Ctrl Pts',(-21.0039272565248,46.515251686681,-34.0030658219707));
#27012=CARTESIAN_POINT('Ctrl Pts',(-17.6308536707599,47.2543695779982,-33.8451172987782));
#27013=CARTESIAN_POINT('Ctrl Pts',(-16.4058130073886,50.4828670683699,-33.6871687755858));
#27014=CARTESIAN_POINT('Ctrl Pts',(-18.4395123779619,53.2735636735887,-33.5292202523933));
#27015=CARTESIAN_POINT('Ctrl Pts',(-21.8880584153516,53.0962196569031,-33.3712717292008));
#27016=CARTESIAN_POINT('Ctrl Pts',(-23.6247593102429,50.1116274445677,-33.2133232060084));
#27017=CARTESIAN_POINT('Ctrl Pts',(-22.0750011806081,47.025826023238,-33.0553746828159));
#27018=CARTESIAN_POINT('Ctrl Pts',(-18.6439025888241,46.6366176912258,-32.8974261596234));
#27019=CARTESIAN_POINT('Ctrl Pts',(-16.4423362759149,49.2968858059303,-32.7394776364309));
#27020=CARTESIAN_POINT('Ctrl Pts',(-17.4663954601827,52.5946461761462,-32.5815291132385));
#27021=CARTESIAN_POINT('Ctrl Pts',(-20.7875968246039,53.5399197710466,-32.423580590046));
#27022=CARTESIAN_POINT('Ctrl Pts',(-23.3947081018314,51.2756557713323,-32.2656320668536));
#27023=CARTESIAN_POINT('Ctrl Pts',(-22.9239407885082,47.8547934810673,-32.107683543661));
#27024=CARTESIAN_POINT('Ctrl Pts',(-19.8021252898838,46.3789246980118,-31.9497350204686));
#27025=CARTESIAN_POINT('Ctrl Pts',(-16.8597167728345,48.1861747612417,-31.7917864972761));
#27026=CARTESIAN_POINT('Ctrl Pts',(-16.7645075504591,51.637965003453,-31.6338379740837));
#27027=CARTESIAN_POINT('Ctrl Pts',(-19.6028209290277,53.604662193487,-31.4758894508912));
#27028=CARTESIAN_POINT('Ctrl Pts',(-22.8012444915916,52.3031218035313,-31.3179409276987));
#27029=CARTESIAN_POINT('Ctrl Pts',(-23.4598648696293,48.913410920597,-31.1599924045063));
#27030=CARTESIAN_POINT('Ctrl Pts',(-20.9815309974076,46.5088773088445,-31.0020438813138));
#27031=CARTESIAN_POINT('Ctrl Pts',(-17.6132728217522,47.2696384634655,-30.8440953581213));
#27032=CARTESIAN_POINT('Ctrl Pts',(-16.4089875895884,50.5059353830703,-30.6861468349289));
#27033=CARTESIAN_POINT('Ctrl Pts',(-18.460564094239,53.2835160781738,-30.5281983117364));
#27034=CARTESIAN_POINT('Ctrl Pts',(-21.9079003148171,53.0840326088254,-30.3702497885439));
#27035=CARTESIAN_POINT('Ctrl Pts',(-23.6254013461144,50.0883505696652,-30.2123012653514));
#27036=CARTESIAN_POINT('Ctrl Pts',(-22.05586123849,47.0125637560539,-30.054352742159));
#27037=CARTESIAN_POINT('Ctrl Pts',(-18.6223342721148,46.6453945260559,-29.8964042189665));
#27038=CARTESIAN_POINT('Ctrl Pts',(-16.4378949214142,49.3197440535823,-29.738455695774));
#27039=CARTESIAN_POINT('Ctrl Pts',(-17.4831079089184,52.6108609586507,-29.5805071725816));
#27040=CARTESIAN_POINT('Ctrl Pts',(-20.8103104076337,53.5347896383079,-29.4225586493891));
#27041=CARTESIAN_POINT('Ctrl Pts',(-23.4028291041448,51.2538320585774,-29.2646101261967));
#27042=CARTESIAN_POINT('Ctrl Pts',(-22.9101061444555,47.8360630851142,-29.1066616030042));
#27043=CARTESIAN_POINT('Ctrl Pts',(-19.7788784501499,46.3802698988112,-28.9487130798117));
#27044=CARTESIAN_POINT('Ctrl Pts',(-16.8481349406148,48.2063759069389,-28.7907645566192));
#27045=CARTESIAN_POINT('Ctrl Pts',(-16.7750916195284,51.6587063280462,-28.6328160334268));
#27046=CARTESIAN_POINT('Ctrl Pts',(-19.6259746483565,53.6071381719488,-28.4748675102343));
#27047=CARTESIAN_POINT('Ctrl Pts',(-22.8159750830834,52.2850875351969,-28.3169189870418));
#27048=CARTESIAN_POINT('Ctrl Pts',(-23.4528165638848,48.8912175406165,-28.1589704638494));
#27049=CARTESIAN_POINT('Ctrl Pts',(-20.9590942591762,46.5026468548974,-28.0010219406569));
#27050=CARTESIAN_POINT('Ctrl Pts',(-17.5957903984424,47.2850199483718,-27.8430734174645));
#27051=CARTESIAN_POINT('Ctrl Pts',(-16.4123101845813,50.5289827832734,-27.685124894272));
#27052=CARTESIAN_POINT('Ctrl Pts',(-18.4816793672832,53.2933332139959,-27.5271763710795));
#27053=CARTESIAN_POINT('Ctrl Pts',(-21.9276633802435,53.0717181892534,-27.369227847887));
#27054=CARTESIAN_POINT('Ctrl Pts',(-23.6258942504405,50.0650704860399,-27.2112793246945));
#27055=CARTESIAN_POINT('Ctrl Pts',(-22.0366358520053,46.9994237957239,-27.0533308015021));
#27056=CARTESIAN_POINT('Ctrl Pts',(-18.6008241139817,46.6543113906855,-26.8953822783096));
#27057=CARTESIAN_POINT('Ctrl Pts',(-16.4335977273107,49.34262692179,-26.7374337551171));
#27058=CARTESIAN_POINT('Ctrl Pts',(-17.4999295124278,52.6269749186172,-26.5794852319247));
#27059=CARTESIAN_POINT('Ctrl Pts',(-20.8329798605529,53.5295001824726,-26.4215367087322));
#27060=CARTESIAN_POINT('Ctrl Pts',(-23.4108311578128,51.2319837018569,-26.2635881855397));
#27061=CARTESIAN_POINT('Ctrl Pts',(-22.8961090069582,47.8173680419797,-26.1056396623473));
#27062=CARTESIAN_POINT('Ctrl Pts',(-19.7557253769871,46.3818716002278,-25.9476911391548));
#27063=CARTESIAN_POINT('Ctrl Pts',(-16.8365144975983,48.2264374122185,-25.7897426159623));
#27064=CARTESIAN_POINT('Ctrl Pts',(-16.7861443246926,51.6798046863575,-25.6317940927699));
#27065=CARTESIAN_POINT('Ctrl Pts',(-19.6484750337391,53.6086169320315,-25.4738455695774));
#27066=CARTESIAN_POINT('Ctrl Pts',(-22.8319255534364,52.2686663415281,-25.315897046385));
#27067=CARTESIAN_POINT('Ctrl Pts',(-23.4429082212044,48.865459646895,-25.1579485231924));
#27068=CARTESIAN_POINT('Ctrl Pts',(-21.7760378723045,47.2933710986319,-25.0526495077308));
#27069=CARTESIAN_POINT('Ctrl Pts',(-20.7937992825328,47.0307770462543,-25.));
#27070=CARTESIAN_POINT('Ctrl Pts',(-17.4818815371047,49.9978011132584,-38.387416697508));
#27071=CARTESIAN_POINT('Ctrl Pts',(-17.4802992084132,49.8234380468402,-38.3984493876971));
#27072=CARTESIAN_POINT('Ctrl Pts',(-17.4968844920688,49.6493740673602,-38.4094820778862));
#27073=CARTESIAN_POINT('Ctrl Pts',(-17.5327553820264,49.4793798202593,-38.4205147680753));
#27074=CARTESIAN_POINT('Ctrl Pts',(-17.7039361788915,48.6681440043768,-38.4731642758061));
#27075=CARTESIAN_POINT('Ctrl Pts',(-18.3143136885385,47.9495893857989,-38.5258137835369));
#27076=CARTESIAN_POINT('Ctrl Pts',(-19.0871833876552,47.6494490720967,-38.5784632912678));
#27077=CARTESIAN_POINT('Ctrl Pts',(-19.8600530867719,47.3493087583945,-38.6311127989986));
#27078=CARTESIAN_POINT('Ctrl Pts',(-20.7954149753583,47.467582749568,-38.6837623067294));
#27079=CARTESIAN_POINT('Ctrl Pts',(-21.4692352948593,47.950678622831,-38.7364118144603));
#27080=CARTESIAN_POINT('Ctrl Pts',(-22.1430556143602,48.4337744960939,-38.7890613221911));
#27081=CARTESIAN_POINT('Ctrl Pts',(-22.5553343647758,49.2816922514464,-38.8417108299219));
#27082=CARTESIAN_POINT('Ctrl Pts',(-22.5191745698723,50.1099909047412,-38.8943603376527));
#27083=CARTESIAN_POINT('Ctrl Pts',(-22.4830147749687,50.938289558036,-38.9470098453835));
#27084=CARTESIAN_POINT('Ctrl Pts',(-21.9984164347461,51.7469691092731,-38.9996593531144));
#27085=CARTESIAN_POINT('Ctrl Pts',(-21.2850582155025,52.1695272697615,-39.0523088608452));
#27086=CARTESIAN_POINT('Ctrl Pts',(-20.5716999962589,52.5920854302499,-39.104958368576));
#27087=CARTESIAN_POINT('Ctrl Pts',(-19.6295818979943,52.6285221999896,-39.1576078763068));
#27088=CARTESIAN_POINT('Ctrl Pts',(-18.8858120137717,52.2621198072975,-39.2102573840377));
#27089=CARTESIAN_POINT('Ctrl Pts',(-18.1420421295491,51.8957174146055,-39.2629068917685));
#27090=CARTESIAN_POINT('Ctrl Pts',(-17.5966204593686,51.1264758594817,-39.3155563994993));
#27091=CARTESIAN_POINT('Ctrl Pts',(-17.4967794589032,50.3035170019982,-39.3682059072301));
#27092=CARTESIAN_POINT('Ctrl Pts',(-17.4846361068648,50.2034230619036,-39.3746095039894));
#27093=CARTESIAN_POINT('Ctrl Pts',(-17.4790842761961,50.1025344761466,-39.3810131007487));
#27094=CARTESIAN_POINT('Ctrl Pts',(-17.4798420534852,50.0015648820515,-39.387416697508));
#27095=CARTESIAN_POINT('Ctrl Pts',(-19.2062007174672,47.0307770462543,-40.));
#27096=CARTESIAN_POINT('Ctrl Pts',(-18.2239621276955,47.2933710986319,-39.9473504922692));
#27097=CARTESIAN_POINT('Ctrl Pts',(-16.5570907656171,48.8654532317005,-39.8420514768075));
#27098=CARTESIAN_POINT('Ctrl Pts',(-17.16807532845,52.2686690815805,-39.6841029536151));
#27099=CARTESIAN_POINT('Ctrl Pts',(-20.3515248609294,53.6086146806686,-39.5261544304226));
#27100=CARTESIAN_POINT('Ctrl Pts',(-23.2138551423641,51.6798054402274,-39.3682059072301));
#27101=CARTESIAN_POINT('Ctrl Pts',(-23.1634851378897,48.2264371018949,-39.2102573840377));
#27102=CARTESIAN_POINT('Ctrl Pts',(-20.2442745178934,46.3818724340551,-39.0523088608451));
#27103=CARTESIAN_POINT('Ctrl Pts',(-17.103891455686,47.8173681789784,-38.8943603376527));
#27104=CARTESIAN_POINT('Ctrl Pts',(-16.5891692994355,51.231983621924,-38.7364118144602));
#27105=CARTESIAN_POINT('Ctrl Pts',(-19.167020277377,53.5294996249073,-38.5784632912678));
#27106=CARTESIAN_POINT('Ctrl Pts',(-22.5000701187915,52.6269745712345,-38.4205147680753));
#27107=CARTESIAN_POINT('Ctrl Pts',(-23.5664017687871,49.3426270004872,-38.2625662448828));
#27108=CARTESIAN_POINT('Ctrl Pts',(-21.3991756821973,46.6543118776375,-38.1046177216904));
#27109=CARTESIAN_POINT('Ctrl Pts',(-17.9633644414303,46.9994242206471,-37.9466691984979));
#27110=CARTESIAN_POINT('Ctrl Pts',(-16.3741062672361,50.0650704790755,-37.7887206753054));
#27111=CARTESIAN_POINT('Ctrl Pts',(-18.0723368961882,53.0717177485,-37.630772152113));
#27112=CARTESIAN_POINT('Ctrl Pts',(-21.5183204151355,53.2933327434377,-37.4728236289205));
#27113=CARTESIAN_POINT('Ctrl Pts',(-23.5876893022666,50.5289827072374,-37.314875105728));
#27114=CARTESIAN_POINT('Ctrl Pts',(-22.4042092574597,47.2850203370204,-37.1569265825356));
#27115=CARTESIAN_POINT('Ctrl Pts',(-19.0409058781059,46.5026473552099,-36.9989780593431));
#27116=CARTESIAN_POINT('Ctrl Pts',(-16.5471839301236,48.891217699314,-36.8410295361507));
#27117=CARTESIAN_POINT('Ctrl Pts',(-17.1840253198474,52.2850872082152,-36.6830810129582));
#27118=CARTESIAN_POINT('Ctrl Pts',(-20.3740252981191,53.6071376558454,-36.5251324897657));
#27119=CARTESIAN_POINT('Ctrl Pts',(-23.2249079190488,51.6587060907077,-36.3671839665732));
#27120=CARTESIAN_POINT('Ctrl Pts',(-23.1518646084073,48.2063761635784,-36.2092354433808));
#27121=CARTESIAN_POINT('Ctrl Pts',(-20.2211215182128,46.3802704167281,-36.0512869201883));
#27122=CARTESIAN_POINT('Ctrl Pts',(-17.0898942719283,47.8360633947361,-35.8933383969959));
#27123=CARTESIAN_POINT('Ctrl Pts',(-16.5971713827397,51.2538318791758,-35.7353898738033));
#27124=CARTESIAN_POINT('Ctrl Pts',(-19.1896897083071,53.5347891325428,-35.5774413506109));
#27125=CARTESIAN_POINT('Ctrl Pts',(-22.5168917309592,52.6108605850829,-35.4194928274184));
#27126=CARTESIAN_POINT('Ctrl Pts',(-23.562104568912,49.319744150915,-35.261544304226));
#27127=CARTESIAN_POINT('Ctrl Pts',(-21.3776655307659,46.6453950060402,-35.1035957810335));
#27128=CARTESIAN_POINT('Ctrl Pts',(-17.9441390556672,47.0125641835028,-34.945647257841));
#27129=CARTESIAN_POINT('Ctrl Pts',(-16.374599172616,50.0883505570237,-34.7876987346486));
#27130=CARTESIAN_POINT('Ctrl Pts',(-18.0920999581694,53.0840321675552,-34.6297502114561));
#27131=CARTESIAN_POINT('Ctrl Pts',(-21.5394356854951,53.2835156083612,-34.4718016882636));
#27132=CARTESIAN_POINT('Ctrl Pts',(-23.5910118966017,50.50593531068,-34.3138531650712));
#27133=CARTESIAN_POINT('Ctrl Pts',(-22.3867268367498,47.2696388541317,-34.1559046418787));
#27134=CARTESIAN_POINT('Ctrl Pts',(-19.0184691430321,46.5088778083619,-33.9979561186862));
#27135=CARTESIAN_POINT('Ctrl Pts',(-16.5401356254157,48.9134110760685,-33.8400075954937));
#27136=CARTESIAN_POINT('Ctrl Pts',(-17.1987559092166,52.3031214739955,-33.6820590723013));
#27137=CARTESIAN_POINT('Ctrl Pts',(-20.3971790141429,53.6046616777241,-33.5241105491088));
#27138=CARTESIAN_POINT('Ctrl Pts',(-23.2354919865996,51.6379647690895,-33.3661620259163));
#27139=CARTESIAN_POINT('Ctrl Pts',(-23.140282777847,48.1861750207679,-33.2082135027238));
#27140=CARTESIAN_POINT('Ctrl Pts',(-20.1978746818039,46.3789252161231,-33.0502649795314));
#27141=CARTESIAN_POINT('Ctrl Pts',(-17.0760596298556,47.8547937880081,-32.8923164563389));
#27142=CARTESIAN_POINT('Ctrl Pts',(-16.6052923838908,51.2756555888085,-32.7343679331464));
#27143=CARTESIAN_POINT('Ctrl Pts',(-19.2124032880871,53.5399192645472,-32.576419409954));
#27144=CARTESIAN_POINT('Ctrl Pts',(-22.5336041773036,52.5946458048986,-32.4184708867615));
#27145=CARTESIAN_POINT('Ctrl Pts',(-23.5576632150468,49.2968859065335,-32.260522363569));
#27146=CARTESIAN_POINT('Ctrl Pts',(-21.3560972171426,46.6366181724659,-32.1025738403766));
#27147=CARTESIAN_POINT('Ctrl Pts',(-17.9249991162877,47.0258264487893,-31.9446253171841));
#27148=CARTESIAN_POINT('Ctrl Pts',(-16.3752412083956,50.1116274285957,-31.7866767939916));
#27149=CARTESIAN_POINT('Ctrl Pts',(-18.1119418547959,53.0962192138892,-31.6287282707992));
#27150=CARTESIAN_POINT('Ctrl Pts',(-21.56048739876,53.2735632052001,-31.4707797476067));
#27151=CARTESIAN_POINT('Ctrl Pts',(-23.5941864783473,50.4828669992804,-31.3128312244143));
#27152=CARTESIAN_POINT('Ctrl Pts',(-22.3691459902575,47.2543699708491,-31.1548827012218));
#27153=CARTESIAN_POINT('Ctrl Pts',(-18.9960728871194,46.5152521852863,-30.9969341780293));
#27154=CARTESIAN_POINT('Ctrl Pts',(-16.5332299641673,48.9356492595106,-30.8389856548368));
#27155=CARTESIAN_POINT('Ctrl Pts',(-17.2136019956601,52.321060779372,-30.6810371316444));
#27156=CARTESIAN_POINT('Ctrl Pts',(-20.4203163532235,53.6020370824496,-30.5230886084519));
#27157=CARTESIAN_POINT('Ctrl Pts',(-23.2459426566631,51.6171559138756,-30.3651400852594));
#27158=CARTESIAN_POINT('Ctrl Pts',(-23.1285714741897,48.166048661765,-30.207191562067));
#27159=CARTESIAN_POINT('Ctrl Pts',(-20.1746196872686,46.3777293109224,-30.0492430388745));
#27160=CARTESIAN_POINT('Ctrl Pts',(-17.0623455407189,47.8736126274854,-29.891294515682));
#27161=CARTESIAN_POINT('Ctrl Pts',(-16.6135533476775,51.2974267035548,-29.7333459924896));
#27162=CARTESIAN_POINT('Ctrl Pts',(-19.2351493401782,53.5449034469686,-29.5753974692971));
#27163=CARTESIAN_POINT('Ctrl Pts',(-22.5502121640569,52.5783240483645,-29.4174489461047));
#27164=CARTESIAN_POINT('Ctrl Pts',(-23.5530751799844,49.274056651322,-29.2595004229121));
#27165=CARTESIAN_POINT('Ctrl Pts',(-21.3344729921125,46.627980009892,-29.1015518997197));
#27166=CARTESIAN_POINT('Ctrl Pts',(-17.9059447284621,47.0392113382703,-28.9436033765272));
#27167=CARTESIAN_POINT('Ctrl Pts',(-16.3760326916862,50.1348996976644,-28.7856548533347));
#27168=CARTESIAN_POINT('Ctrl Pts',(-18.1318615954084,53.1082786044884,-28.6277063301423));
#27169=CARTESIAN_POINT('Ctrl Pts',(-21.5814747736461,53.2634758336214,-28.4697578069498));
#27170=CARTESIAN_POINT('Ctrl Pts',(-23.5972128731322,50.4597787805748,-28.3118092837574));
#27171=CARTESIAN_POINT('Ctrl Pts',(-22.3514674645701,47.2392142866714,-28.1538607605649));
#27172=CARTESIAN_POINT('Ctrl Pts',(-18.9737180230564,46.5217702416014,-27.9959122373724));
#27173=CARTESIAN_POINT('Ctrl Pts',(-16.5264672360391,48.9579313168502,-27.8379637141799));
#27174=CARTESIAN_POINT('Ctrl Pts',(-17.2285629654577,52.3389044059643,-27.6800151909875));
#27175=CARTESIAN_POINT('Ctrl Pts',(-20.4434363605156,53.599263941172,-27.522066667795));
#27176=CARTESIAN_POINT('Ctrl Pts',(-23.2562595022286,51.5962804541496,-27.3641181446025));
#27177=CARTESIAN_POINT('Ctrl Pts',(-23.1167311715492,48.1459977760775,-27.2061696214101));
#27178=CARTESIAN_POINT('Ctrl Pts',(-20.151357511322,46.3766830290446,-27.0482210982176));
#27179=CARTESIAN_POINT('Ctrl Pts',(-17.0487525340105,47.892518582992,-26.8902725750251));
#27180=CARTESIAN_POINT('Ctrl Pts',(-16.6219540051685,51.3191454290078,-26.7323240518326));
#27181=CARTESIAN_POINT('Ctrl Pts',(-19.2579267840424,53.5497392783032,-26.5743755286402));
#27182=CARTESIAN_POINT('Ctrl Pts',(-22.5667152906276,52.5619003598412,-26.4164270054477));
#27183=CARTESIAN_POINT('Ctrl Pts',(-23.5483400872305,49.251248624616,-26.2584784822553));
#27184=CARTESIAN_POINT('Ctrl Pts',(-21.3127948732631,46.619498196827,-26.1005299590628));
#27185=CARTESIAN_POINT('Ctrl Pts',(-17.8869744362753,47.0526838174963,-25.9425814358703));
#27186=CARTESIAN_POINT('Ctrl Pts',(-16.3769780519003,50.158235047232,-25.7846329126779));
#27187=CARTESIAN_POINT('Ctrl Pts',(-18.1518494766411,53.1200731989091,-25.6266843894854));
#27188=CARTESIAN_POINT('Ctrl Pts',(-21.6024146227446,53.2535259255151,-25.4687358662929));
#27189=CARTESIAN_POINT('Ctrl Pts',(-23.6000558056709,50.4361300140704,-25.3107873431005));
#27190=CARTESIAN_POINT('Ctrl Pts',(-22.3337614586311,47.2252518860991,-25.152838819908));
#27191=CARTESIAN_POINT('Ctrl Pts',(-18.9512736956997,46.5262657145773,-24.9948902967155));
#27192=CARTESIAN_POINT('Ctrl Pts',(-16.520037414612,48.9847755076057,-24.836941773523));
#27193=CARTESIAN_POINT('Ctrl Pts',(-17.003216778308,51.2245165804373,-24.7316427580614));
#27194=CARTESIAN_POINT('Ctrl Pts',(-17.6639373423038,51.9973015569306,-24.6789932503306));
#27195=CARTESIAN_POINT('Ctrl Pts',(-19.2540671456531,47.2098224301578,-40.1070022498898));
#27196=CARTESIAN_POINT('Ctrl Pts',(-18.3310579529763,47.4565819515315,-40.054352742159));
#27197=CARTESIAN_POINT('Ctrl Pts',(-16.7646996300298,48.9338668755566,-39.9490537266973));
#27198=CARTESIAN_POINT('Ctrl Pts',(-17.3388415686086,52.1318673886832,-39.7911052035049));
#27199=CARTESIAN_POINT('Ctrl Pts',(-20.3303277650369,53.391013708655,-39.6331566803124));
#27200=CARTESIAN_POINT('Ctrl Pts',(-23.0200583353412,51.5785124707825,-39.47520815712));
#27201=CARTESIAN_POINT('Ctrl Pts',(-22.9727256631686,48.333383685198,-39.3172596339274));
#27202=CARTESIAN_POINT('Ctrl Pts',(-20.2295446624681,46.600047037023,-39.159311110735));
#27203=CARTESIAN_POINT('Ctrl Pts',(-17.278528010172,47.9489817891393,-39.0013625875425));
#27204=CARTESIAN_POINT('Ctrl Pts',(-16.7948438148646,51.1576944951099,-38.8434140643501));
#27205=CARTESIAN_POINT('Ctrl Pts',(-19.2172493024601,53.3166693237904,-38.6854655411576));
#27206=CARTESIAN_POINT('Ctrl Pts',(-22.3493148467294,52.4685669077014,-38.5275170179651));
#27207=CARTESIAN_POINT('Ctrl Pts',(-23.3513462529859,49.3822668668425,-38.3695684947726));
#27208=CARTESIAN_POINT('Ctrl Pts',(-21.314804804338,46.8560582684008,-38.2116199715802));
#27209=CARTESIAN_POINT('Ctrl Pts',(-18.0861744160049,47.1803601930261,-38.0536714483877));
#27210=CARTESIAN_POINT('Ctrl Pts',(-16.5927491733059,50.0611467020172,-37.8957229251953));
#27211=CARTESIAN_POINT('Ctrl Pts',(-18.1885757862396,52.8864918856763,-37.7377744020028));
#27212=CARTESIAN_POINT('Ctrl Pts',(-21.4267650601314,53.0947434038844,-37.5798258788103));
#27213=CARTESIAN_POINT('Ctrl Pts',(-23.3713501393079,50.4970848291154,-37.4218773556178));
#27214=CARTESIAN_POINT('Ctrl Pts',(-22.2592344353625,47.448734744332,-37.2639288324254));
#27215=CARTESIAN_POINT('Ctrl Pts',(-19.0987396541238,46.7135391800028,-37.1059803092329));
#27216=CARTESIAN_POINT('Ctrl Pts',(-16.7553901808531,48.9580777350151,-36.9480317860405));
#27217=CARTESIAN_POINT('Ctrl Pts',(-17.3538297688648,52.1472954954265,-36.790083262848));
#27218=CARTESIAN_POINT('Ctrl Pts',(-20.3514714164691,53.3896257490454,-36.6321347396555));
#27219=CARTESIAN_POINT('Ctrl Pts',(-23.0304446249768,51.5586854208488,-36.474186216463));
#27220=CARTESIAN_POINT('Ctrl Pts',(-22.961805856466,48.3145324298384,-36.3162376932706));
#27221=CARTESIAN_POINT('Ctrl Pts',(-20.2077877983358,46.5985416220098,-36.1582891700781));
#27222=CARTESIAN_POINT('Ctrl Pts',(-17.2653748624394,47.9665496755805,-36.0003406468856));
#27223=CARTESIAN_POINT('Ctrl Pts',(-16.8023633692043,51.1782252933267,-35.8423921236932));
#27224=CARTESIAN_POINT('Ctrl Pts',(-19.2385517572395,53.3216398719068,-35.6844436005007));
#27225=CARTESIAN_POINT('Ctrl Pts',(-22.3651221086596,52.4534246016432,-35.5264950773082));
#27226=CARTESIAN_POINT('Ctrl Pts',(-23.3473081760575,49.3607638626542,-35.3685465541158));
#27227=CARTESIAN_POINT('Ctrl Pts',(-21.2945917240194,46.8476790878841,-35.2105980309233));
#27228=CARTESIAN_POINT('Ctrl Pts',(-18.0681083290308,47.1927078106349,-35.0526495077308));
#27229=CARTESIAN_POINT('Ctrl Pts',(-16.5932123562856,50.0830229815446,-34.8947009845384));
#27230=CARTESIAN_POINT('Ctrl Pts',(-18.2071471273313,52.8980637401206,-34.7367524613459));
#27231=CARTESIAN_POINT('Ctrl Pts',(-21.4466070708717,53.0855182461522,-34.5788039381534));
#27232=CARTESIAN_POINT('Ctrl Pts',(-23.3744723798173,50.4754272001937,-34.4208554149609));
#27233=CARTESIAN_POINT('Ctrl Pts',(-22.2428062119211,47.434280771284,-34.2629068917685));
#27234=CARTESIAN_POINT('Ctrl Pts',(-19.0776558635433,46.7193939342282,-34.104958368576));
#27235=CARTESIAN_POINT('Ctrl Pts',(-16.7487668918621,48.9789328418844,-33.9470098453835));
#27236=CARTESIAN_POINT('Ctrl Pts',(-17.3676720975443,52.1642422874502,-33.7890613221911));
#27237=CARTESIAN_POINT('Ctrl Pts',(-20.3732289537489,53.3872990734386,-33.6311127989986));
#27238=CARTESIAN_POINT('Ctrl Pts',(-23.0403904688349,51.5391948095847,-33.4731642758062));
#27239=CARTESIAN_POINT('Ctrl Pts',(-22.9509224151245,48.2955494243743,-33.3152157526136));
#27240=CARTESIAN_POINT('Ctrl Pts',(-20.185942755869,46.5972775375629,-33.1572672294212));
#27241=CARTESIAN_POINT('Ctrl Pts',(-17.2523744550604,47.9841506183174,-32.9993187062287));
#27242=CARTESIAN_POINT('Ctrl Pts',(-16.8099946705951,51.1987330241562,-32.8413701830363));
#27243=CARTESIAN_POINT('Ctrl Pts',(-19.2598956986747,53.3264606548093,-32.6834216598438));
#27244=CARTESIAN_POINT('Ctrl Pts',(-22.3808267875112,52.4381875794745,-32.5254731366513));
#27245=CARTESIAN_POINT('Ctrl Pts',(-23.3431346376848,49.3392839799533,-32.3675246134589));
#27246=CARTESIAN_POINT('Ctrl Pts',(-21.2743239887134,46.8394315010391,-32.2095760902664));
#27247=CARTESIAN_POINT('Ctrl Pts',(-18.0501225359877,47.2051703557871,-32.0516275670739));
#27248=CARTESIAN_POINT('Ctrl Pts',(-16.5938156770396,50.1048962480416,-31.8936790438815));
#27249=CARTESIAN_POINT('Ctrl Pts',(-18.2257925493063,52.909515902472,-31.735730520689));
#27250=CARTESIAN_POINT('Ctrl Pts',(-21.4663893570366,53.0761659770572,-31.5777819974965));
#27251=CARTESIAN_POINT('Ctrl Pts',(-23.3774555329581,50.4537499176037,-31.4198334743041));
#27252=CARTESIAN_POINT('Ctrl Pts',(-22.2262854978131,47.4199326080388,-31.2618849511116));
#27253=CARTESIAN_POINT('Ctrl Pts',(-19.0566101112138,46.7253839335625,-31.1039364279191));
#27254=CARTESIAN_POINT('Ctrl Pts',(-16.7422776448703,48.9998300535794,-30.9459879047266));
#27255=CARTESIAN_POINT('Ctrl Pts',(-17.3816229587763,52.1810998452219,-30.7880393815342));
#27256=CARTESIAN_POINT('Ctrl Pts',(-20.3949711016219,53.384832742355,-30.6300908583417));
#27257=CARTESIAN_POINT('Ctrl Pts',(-23.0502109591299,51.5196407370289,-30.4721423351493));
#27258=CARTESIAN_POINT('Ctrl Pts',(-22.9399173079678,48.276636693223,-30.3141938119568));
#27259=CARTESIAN_POINT('Ctrl Pts',(-20.1640900472143,46.5961537459451,-30.1562452887643));
#27260=CARTESIAN_POINT('Ctrl Pts',(-17.2394873312249,48.0018346739166,-29.9982967655719));
#27261=CARTESIAN_POINT('Ctrl Pts',(-16.8177574948161,51.2191913315927,-29.8403482423794));
#27262=CARTESIAN_POINT('Ctrl Pts',(-19.2812701543271,53.3311442889496,-29.6823997191869));
#27263=CARTESIAN_POINT('Ctrl Pts',(-22.3964333057287,52.4228500316744,-29.5244511959944));
#27264=CARTESIAN_POINT('Ctrl Pts',(-23.3388232630524,49.3178313383634,-29.3665026728019));
#27265=CARTESIAN_POINT('Ctrl Pts',(-21.2540037134818,46.8313142232752,-29.2085541496095));
#27266=CARTESIAN_POINT('Ctrl Pts',(-18.0322171357041,47.2177481308435,-29.050605626417));
#27267=CARTESIAN_POINT('Ctrl Pts',(-16.5945594335573,50.1267651895682,-28.8926571032246));
#27268=CARTESIAN_POINT('Ctrl Pts',(-18.2445111212424,52.9208481067826,-28.7347085800321));
#27269=CARTESIAN_POINT('Ctrl Pts',(-21.4861111844538,53.0666868781967,-28.5767600568396));
#27270=CARTESIAN_POINT('Ctrl Pts',(-23.3802994348738,50.4320539281265,-28.4188115336471));
#27271=CARTESIAN_POINT('Ctrl Pts',(-22.2096729946064,47.4056908179454,-28.2608630104547));
#27272=CARTESIAN_POINT('Ctrl Pts',(-19.035603254788,46.7315089483602,-28.1029144872622));
#27273=CARTESIAN_POINT('Ctrl Pts',(-16.7359227120721,49.0207684935577,-27.9449659640697));
#27274=CARTESIAN_POINT('Ctrl Pts',(-17.3956817758482,52.1978674936802,-27.7870174408773));
#27275=CARTESIAN_POINT('Ctrl Pts',(-20.4166969628207,53.3822268226544,-27.6290689176848));
#27276=CARTESIAN_POINT('Ctrl Pts',(-23.0599056946001,51.5000240762409,-27.4711203944924));
#27277=CARTESIAN_POINT('Ctrl Pts',(-22.9287909805204,48.2577948843147,-27.3131718712999));
#27278=CARTESIAN_POINT('Ctrl Pts',(-20.1422305901903,46.5951705553014,-27.1552233481074));
#27279=CARTESIAN_POINT('Ctrl Pts',(-17.2267139884967,48.0196005924119,-26.9972748249149));
#27280=CARTESIAN_POINT('Ctrl Pts',(-16.8256515891527,51.2396004088323,-26.8393263017225));
#27281=CARTESIAN_POINT('Ctrl Pts',(-19.3026741088157,53.3356885176355,-26.68137777853));
#27282=CARTESIAN_POINT('Ctrl Pts',(-22.4119412868763,52.4074166984269,-26.5234292553375));
#27283=CARTESIAN_POINT('Ctrl Pts',(-23.3343736983688,49.2963986451912,-26.3654807321451));
#27284=CARTESIAN_POINT('Ctrl Pts',(-21.2336327942506,46.8233438670796,-26.2075322089526));
#27285=CARTESIAN_POINT('Ctrl Pts',(-18.0143907600572,47.2304082139468,-26.0495836857601));
#27286=CARTESIAN_POINT('Ctrl Pts',(-16.5954477881557,50.1486934078131,-25.8916351625677));
#27287=CARTESIAN_POINT('Ctrl Pts',(-18.263293724891,52.931931482235,-25.7336866393752));
#27288=CARTESIAN_POINT('Ctrl Pts',(-21.5057883519083,53.0573369537037,-25.5757381161827));
#27289=CARTESIAN_POINT('Ctrl Pts',(-23.3829709373934,50.4098311921169,-25.4177895929903));
#27290=CARTESIAN_POINT('Ctrl Pts',(-22.1930346682185,47.3925703559575,-25.2598410697978));
#27291=CARTESIAN_POINT('Ctrl Pts',(-19.0145123297425,46.7357333424386,-25.1018925466053));
#27292=CARTESIAN_POINT('Ctrl Pts',(-16.7298806115618,49.0459939684019,-24.9439440234128));
#27293=CARTESIAN_POINT('Ctrl Pts',(-17.1839240578764,51.1506777193426,-24.8386450079512));
#27294=CARTESIAN_POINT('Ctrl Pts',(-17.8048028959808,51.8768634390787,-24.7859955002204));
#27295=CARTESIAN_POINT('Ctrl Pts',(-19.301933573839,47.3888678140614,-40.2140044997796));
#27296=CARTESIAN_POINT('Ctrl Pts',(-18.438153778257,47.6197928044311,-40.1613549920488));
#27297=CARTESIAN_POINT('Ctrl Pts',(-16.9723084944424,49.0022805194126,-40.0560559765871));
#27298=CARTESIAN_POINT('Ctrl Pts',(-17.5096078087671,51.995065695786,-39.8981074533947));
#27299=CARTESIAN_POINT('Ctrl Pts',(-20.3091306691444,53.1734127366413,-39.7401589302022));
#27300=CARTESIAN_POINT('Ctrl Pts',(-22.8262615283184,51.4772195013377,-39.5822104070098));
#27301=CARTESIAN_POINT('Ctrl Pts',(-22.7819661884474,48.4403302685011,-39.4242618838173));
#27302=CARTESIAN_POINT('Ctrl Pts',(-20.2148148070429,46.8182216399908,-39.2663133606248));
#27303=CARTESIAN_POINT('Ctrl Pts',(-17.4531645646581,48.0805953993001,-39.1083648374324));
#27304=CARTESIAN_POINT('Ctrl Pts',(-17.0005183302937,51.0834053682957,-38.9504163142398));
#27305=CARTESIAN_POINT('Ctrl Pts',(-19.2674783275431,53.1038390226735,-38.7924677910475));
#27306=CARTESIAN_POINT('Ctrl Pts',(-22.1985595746674,52.3101592441684,-38.6345192678549));
#27307=CARTESIAN_POINT('Ctrl Pts',(-23.1362907371846,49.4219067331978,-38.4765707446625));
#27308=CARTESIAN_POINT('Ctrl Pts',(-21.2304339264787,47.0578046591641,-38.31862222147));
#27309=CARTESIAN_POINT('Ctrl Pts',(-18.2089843905794,47.3612961654051,-38.1606736982775));
#27310=CARTESIAN_POINT('Ctrl Pts',(-16.8113920793757,50.0572229249588,-38.002725175085));
#27311=CARTESIAN_POINT('Ctrl Pts',(-18.3048146762911,52.7012660228526,-37.8447766518926));
#27312=CARTESIAN_POINT('Ctrl Pts',(-21.3352097051273,52.896154064331,-37.6868281287001));
#27313=CARTESIAN_POINT('Ctrl Pts',(-23.1550109763493,50.4651869509934,-37.5288796055076));
#27314=CARTESIAN_POINT('Ctrl Pts',(-22.1142596132653,47.6124491516436,-37.3709310823152));
#27315=CARTESIAN_POINT('Ctrl Pts',(-19.1565734301417,46.9244310047958,-37.2129825591227));
#27316=CARTESIAN_POINT('Ctrl Pts',(-16.9635964315826,49.0249377707161,-37.0550340359303));
#27317=CARTESIAN_POINT('Ctrl Pts',(-17.5236342178822,52.0095037826378,-36.8970855127378));
#27318=CARTESIAN_POINT('Ctrl Pts',(-20.328917534819,53.1721138422453,-36.7391369895453));
#27319=CARTESIAN_POINT('Ctrl Pts',(-22.8359813309048,51.45866475099,-36.5811884663528));
#27320=CARTESIAN_POINT('Ctrl Pts',(-22.7717471045247,48.4226886960985,-36.4232399431604));
#27321=CARTESIAN_POINT('Ctrl Pts',(-20.1944540784587,46.8168128272913,-36.2652914199679));
#27322=CARTESIAN_POINT('Ctrl Pts',(-17.4408554529505,48.0970359564251,-36.1073428967755));
#27323=CARTESIAN_POINT('Ctrl Pts',(-17.0075553556689,51.1026187074776,-35.9493943735829));
#27324=CARTESIAN_POINT('Ctrl Pts',(-19.2874138061719,53.1084906112709,-35.7914458503905));
#27325=CARTESIAN_POINT('Ctrl Pts',(-22.21335248636,52.2959886182035,-35.633497327198));
#27326=CARTESIAN_POINT('Ctrl Pts',(-23.132511783203,49.4017835743933,-35.4755488040056));
#27327=CARTESIAN_POINT('Ctrl Pts',(-21.2115179172729,47.049963169728,-35.3176002808131));
#27328=CARTESIAN_POINT('Ctrl Pts',(-18.1920776023944,47.3728514377671,-35.1596517576207));
#27329=CARTESIAN_POINT('Ctrl Pts',(-16.8118255399552,50.0776954060655,-35.0017032344282));
#27330=CARTESIAN_POINT('Ctrl Pts',(-18.3221942964933,52.712095312686,-34.8437547112357));
#27331=CARTESIAN_POINT('Ctrl Pts',(-21.3537784562482,52.8875208839431,-34.6858061880432));
#27332=CARTESIAN_POINT('Ctrl Pts',(-23.1579328630329,50.4449190897075,-34.5278576648507));
#27333=CARTESIAN_POINT('Ctrl Pts',(-22.0988855870924,47.5989226884362,-34.3699091416583));
#27334=CARTESIAN_POINT('Ctrl Pts',(-19.1368425840546,46.9299100600946,-34.2119606184658));
#27335=CARTESIAN_POINT('Ctrl Pts',(-16.9573981583085,49.0444546077003,-34.0540120952734));
#27336=CARTESIAN_POINT('Ctrl Pts',(-17.536588285872,52.0253631009049,-33.8960635720809));
#27337=CARTESIAN_POINT('Ctrl Pts',(-20.3492788933548,53.169936469153,-33.7381150488884));
#27338=CARTESIAN_POINT('Ctrl Pts',(-22.8452889510702,51.44042485008,-33.580166525696));
#27339=CARTESIAN_POINT('Ctrl Pts',(-22.7615620524019,48.4049238279808,-33.4222180025034));
#27340=CARTESIAN_POINT('Ctrl Pts',(-20.1740108299341,46.8156298590027,-33.2642694793111));
#27341=CARTESIAN_POINT('Ctrl Pts',(-17.4286892802651,48.1135074486268,-33.1063209561185));
#27342=CARTESIAN_POINT('Ctrl Pts',(-17.0146969572993,51.1218104595037,-32.9483724329261));
#27343=CARTESIAN_POINT('Ctrl Pts',(-19.3073881092624,53.1130020450714,-32.7904239097336));
#27344=CARTESIAN_POINT('Ctrl Pts',(-22.2280493977188,52.2817293540503,-32.6324753865412));
#27345=CARTESIAN_POINT('Ctrl Pts',(-23.1286060603229,49.3816820533731,-32.4745268633487));
#27346=CARTESIAN_POINT('Ctrl Pts',(-21.1925507602843,47.0422448296122,-32.3165783401562));
#27347=CARTESIAN_POINT('Ctrl Pts',(-18.1752459556877,47.3845142627849,-32.1586298169637));
#27348=CARTESIAN_POINT('Ctrl Pts',(-16.8123901456836,50.0981650674874,-32.0006812937713));
#27349=CARTESIAN_POINT('Ctrl Pts',(-18.3396432438168,52.7228125910548,-31.8427327705788));
#27350=CARTESIAN_POINT('Ctrl Pts',(-21.3722913153132,52.8787687489144,-31.6847842473863));
#27351=CARTESIAN_POINT('Ctrl Pts',(-23.1607245875689,50.424632835927,-31.5268357241939));
#27352=CARTESIAN_POINT('Ctrl Pts',(-22.0834250053688,47.5854952452285,-31.3688872010014));
#27353=CARTESIAN_POINT('Ctrl Pts',(-19.117147335308,46.9355156818388,-31.2109386778089));
#27354=CARTESIAN_POINT('Ctrl Pts',(-16.9513253255734,49.0640108476483,-31.0529901546165));
#27355=CARTESIAN_POINT('Ctrl Pts',(-17.5496439218925,52.0411389110718,-30.895041631424));
#27356=CARTESIAN_POINT('Ctrl Pts',(-20.3696258500203,53.1676284022605,-30.7370931082315));
#27357=CARTESIAN_POINT('Ctrl Pts',(-22.8544792615967,51.4221255601822,-30.579144585039));
#27358=CARTESIAN_POINT('Ctrl Pts',(-22.7512631417458,48.387224724681,-30.4211960618466));
#27359=CARTESIAN_POINT('Ctrl Pts',(-20.1535604071599,46.8145781809679,-30.2632475386541));
#27360=CARTESIAN_POINT('Ctrl Pts',(-17.4166291217309,48.1300567203476,-30.1052990154616));
#27361=CARTESIAN_POINT('Ctrl Pts',(-17.0219616419547,51.1409559596307,-29.9473504922692));
#27362=CARTESIAN_POINT('Ctrl Pts',(-19.3273909684762,53.1173851309305,-29.7894019690767));
#27363=CARTESIAN_POINT('Ctrl Pts',(-22.2426544474004,52.2673760149844,-29.6314534458842));
#27364=CARTESIAN_POINT('Ctrl Pts',(-23.1245713461204,49.3616060254048,-29.4735049226918));
#27365=CARTESIAN_POINT('Ctrl Pts',(-21.1735344348511,47.0346484366585,-29.3155563994993));
#27366=CARTESIAN_POINT('Ctrl Pts',(-18.1584895429461,47.3962849234167,-29.1576078763069));
#27367=CARTESIAN_POINT('Ctrl Pts',(-16.8130861754284,50.1186306814719,-28.9996593531144));
#27368=CARTESIAN_POINT('Ctrl Pts',(-18.3571606470765,52.733417609077,-28.8417108299219));
#27369=CARTESIAN_POINT('Ctrl Pts',(-21.3907475952616,52.869897922772,-28.6837623067294));
#27370=CARTESIAN_POINT('Ctrl Pts',(-23.1633859966154,50.4043290756782,-28.525813783537));
#27371=CARTESIAN_POINT('Ctrl Pts',(-22.0678785246426,47.5721673492192,-28.3678652603445));
#27372=CARTESIAN_POINT('Ctrl Pts',(-19.0974884865195,46.941247655119,-28.209916737152));
#27373=CARTESIAN_POINT('Ctrl Pts',(-16.9453781881051,49.0836056702652,-28.0519682139596));
#27374=CARTESIAN_POINT('Ctrl Pts',(-17.5628005862387,52.0568305813959,-27.8940196907671));
#27375=CARTESIAN_POINT('Ctrl Pts',(-20.3899575651257,53.1651897041368,-27.7360711675746));
#27376=CARTESIAN_POINT('Ctrl Pts',(-22.8635518869715,51.4037676983321,-27.5781226443821));
#27377=CARTESIAN_POINT('Ctrl Pts',(-22.7408507894916,48.3695919925519,-27.4201741211897));
#27378=CARTESIAN_POINT('Ctrl Pts',(-20.1331036690585,46.8136580815583,-27.2622255979972));
#27379=CARTESIAN_POINT('Ctrl Pts',(-17.4046754429829,48.1466826018318,-27.1042770748048));
#27380=CARTESIAN_POINT('Ctrl Pts',(-17.0293491731369,51.1600553886568,-26.9463285516123));
#27381=CARTESIAN_POINT('Ctrl Pts',(-19.3474214335891,53.1216377569678,-26.7883800284198));
#27382=CARTESIAN_POINT('Ctrl Pts',(-22.257167283125,52.2529330370124,-26.6304315052273));
#27383=CARTESIAN_POINT('Ctrl Pts',(-23.120407309507,49.3415486657664,-26.4724829820349));
#27384=CARTESIAN_POINT('Ctrl Pts',(-21.1544707152382,47.0271895373323,-26.3145344588424));
#27385=CARTESIAN_POINT('Ctrl Pts',(-18.1418070838391,47.4081326103973,-26.1565859356499));
#27386=CARTESIAN_POINT('Ctrl Pts',(-16.8139175244112,50.1391517683944,-25.9986374124575));
#27387=CARTESIAN_POINT('Ctrl Pts',(-18.3747379731408,52.7437897655609,-25.840688889265));
#27388=CARTESIAN_POINT('Ctrl Pts',(-21.409162081072,52.8611479818924,-25.6827403660725));
#27389=CARTESIAN_POINT('Ctrl Pts',(-23.1658860691158,50.3835323701632,-25.5247918428801));
#27390=CARTESIAN_POINT('Ctrl Pts',(-22.052307877806,47.5598888258158,-25.3668433196876));
#27391=CARTESIAN_POINT('Ctrl Pts',(-19.0777509637852,46.9452009702999,-25.2088947964951));
#27392=CARTESIAN_POINT('Ctrl Pts',(-16.9397238085116,49.1072124291981,-25.0509462733027));
#27393=CARTESIAN_POINT('Ctrl Pts',(-17.3646313374448,51.076838858248,-24.945647257841));
#27394=CARTESIAN_POINT('Ctrl Pts',(-17.9456684496579,51.7564253212268,-24.8929977501102));
#27395=CARTESIAN_POINT('Ctrl Pts',(-19.3498000020249,47.5679131979649,-40.3210067496694));
#27396=CARTESIAN_POINT('Ctrl Pts',(-18.5452496035378,47.7830036573307,-40.2683572419386));
#27397=CARTESIAN_POINT('Ctrl Pts',(-17.1799173588551,49.0706941632686,-40.163058226477));
#27398=CARTESIAN_POINT('Ctrl Pts',(-17.6803740489257,51.8582640028888,-40.0051097032845));
#27399=CARTESIAN_POINT('Ctrl Pts',(-20.2879335732519,52.9558117646276,-39.847161180092));
#27400=CARTESIAN_POINT('Ctrl Pts',(-22.6324647212955,51.3759265318928,-39.6892126568996));
#27401=CARTESIAN_POINT('Ctrl Pts',(-22.5912067137262,48.5472768518042,-39.5312641337071));
#27402=CARTESIAN_POINT('Ctrl Pts',(-20.2000849516176,47.0363962429587,-39.3733156105146));
#27403=CARTESIAN_POINT('Ctrl Pts',(-17.6278011191441,48.2122090094609,-39.2153670873221));
#27404=CARTESIAN_POINT('Ctrl Pts',(-17.2061928457228,51.0091162414817,-39.0574185641297));
#27405=CARTESIAN_POINT('Ctrl Pts',(-19.3177073526262,52.8910087215565,-38.8994700409372));
#27406=CARTESIAN_POINT('Ctrl Pts',(-22.0478043026054,52.1517515806355,-38.7415215177447));
#27407=CARTESIAN_POINT('Ctrl Pts',(-22.9212352213833,49.461546599553,-38.5835729945523));
#27408=CARTESIAN_POINT('Ctrl Pts',(-21.1460630486194,47.2595510499276,-38.4256244713598));
#27409=CARTESIAN_POINT('Ctrl Pts',(-18.331794365154,47.5422321377839,-38.2676759481673));
#27410=CARTESIAN_POINT('Ctrl Pts',(-17.0300349854455,50.0532991479006,-38.1097274249749));
#27411=CARTESIAN_POINT('Ctrl Pts',(-18.4210535663425,52.5160401600288,-37.9517789017824));
#27412=CARTESIAN_POINT('Ctrl Pts',(-21.2436543501232,52.6975647247778,-37.79383037859));
#27413=CARTESIAN_POINT('Ctrl Pts',(-22.9386718133906,50.4332890728714,-37.6358818553974));
#27414=CARTESIAN_POINT('Ctrl Pts',(-21.969284791168,47.7761635589552,-37.477933332205));
#27415=CARTESIAN_POINT('Ctrl Pts',(-19.2144072061596,47.1353228295887,-37.3199848090125));
#27416=CARTESIAN_POINT('Ctrl Pts',(-17.1718026823121,49.0917978064171,-37.1620362858201));
#27417=CARTESIAN_POINT('Ctrl Pts',(-17.6934386668996,51.8717120698492,-37.0040877626276));
#27418=CARTESIAN_POINT('Ctrl Pts',(-20.306363653169,52.9546019354452,-36.8461392394351));
#27419=CARTESIAN_POINT('Ctrl Pts',(-22.6415180368327,51.3586440811311,-36.6881907162426));
#27420=CARTESIAN_POINT('Ctrl Pts',(-22.5816883525835,48.5308449623585,-36.5302421930502));
#27421=CARTESIAN_POINT('Ctrl Pts',(-20.1811203585817,47.035084032573,-36.3722936698577));
#27422=CARTESIAN_POINT('Ctrl Pts',(-17.6163360434617,48.2275222372696,-36.2143451466653));
#27423=CARTESIAN_POINT('Ctrl Pts',(-17.2127473421335,51.0270121216285,-36.0563966234728));
#27424=CARTESIAN_POINT('Ctrl Pts',(-19.3362758551043,52.8953413506349,-35.8984481002803));
#27425=CARTESIAN_POINT('Ctrl Pts',(-22.0615828640604,52.1385526347637,-35.7404995770878));
#27426=CARTESIAN_POINT('Ctrl Pts',(-22.9177153903485,49.4428032861326,-35.5825510538954));
#27427=CARTESIAN_POINT('Ctrl Pts',(-21.1284441105265,47.2522472515719,-35.4246025307029));
#27428=CARTESIAN_POINT('Ctrl Pts',(-18.3160468757579,47.5529950648994,-35.2666540075104));
#27429=CARTESIAN_POINT('Ctrl Pts',(-17.0304387236248,50.0723678305864,-35.108705484318));
#27430=CARTESIAN_POINT('Ctrl Pts',(-18.4372414656552,52.5261268852514,-34.9507569611255));
#27431=CARTESIAN_POINT('Ctrl Pts',(-21.2609498416249,52.689523521734,-34.792808437933));
#27432=CARTESIAN_POINT('Ctrl Pts',(-22.9413933462485,50.4144109792213,-34.6348599147405));
#27433=CARTESIAN_POINT('Ctrl Pts',(-21.9549649622637,47.7635646055886,-34.4769113915481));
#27434=CARTESIAN_POINT('Ctrl Pts',(-19.1960293045659,47.140426185961,-34.3189628683556));
#27435=CARTESIAN_POINT('Ctrl Pts',(-17.1660294247548,49.1099763735163,-34.1610143451632));
#27436=CARTESIAN_POINT('Ctrl Pts',(-17.7055044741997,51.8864839143595,-34.0030658219707));
#27437=CARTESIAN_POINT('Ctrl Pts',(-20.3253288329608,52.9525738648675,-33.8451172987782));
#27438=CARTESIAN_POINT('Ctrl Pts',(-22.6501874333055,51.3416548905751,-33.6871687755858));
#27439=CARTESIAN_POINT('Ctrl Pts',(-22.5722016896794,48.5142982315872,-33.5292202523932));
#27440=CARTESIAN_POINT('Ctrl Pts',(-20.1620789039991,47.0339821804424,-33.3712717292009));
#27441=CARTESIAN_POINT('Ctrl Pts',(-17.6050041054698,48.2428642789362,-33.2133232060083));
#27442=CARTESIAN_POINT('Ctrl Pts',(-17.2193992440036,51.0448878948513,-33.0553746828159));
#27443=CARTESIAN_POINT('Ctrl Pts',(-19.3548805198501,52.8995434353335,-32.8974261596234));
#27444=CARTESIAN_POINT('Ctrl Pts',(-22.0752720079264,52.1252711286261,-32.739477636431));
#27445=CARTESIAN_POINT('Ctrl Pts',(-22.9140774829609,49.4240801267929,-32.5815291132385));
#27446=CARTESIAN_POINT('Ctrl Pts',(-21.1107775318551,47.2450581581855,-32.423580590046));
#27447=CARTESIAN_POINT('Ctrl Pts',(-18.3003693753878,47.5638581697826,-32.2656320668535));
#27448=CARTESIAN_POINT('Ctrl Pts',(-17.0309646143276,50.0914338869334,-32.1076835436611));
#27449=CARTESIAN_POINT('Ctrl Pts',(-18.4534939383272,52.5361092796376,-31.9497350204686));
#27450=CARTESIAN_POINT('Ctrl Pts',(-21.2781932735898,52.6813715207715,-31.7917864972761));
#27451=CARTESIAN_POINT('Ctrl Pts',(-22.9439936421797,50.3955157542503,-31.6338379740837));
#27452=CARTESIAN_POINT('Ctrl Pts',(-21.9405645129244,47.7510578824183,-31.4758894508912));
#27453=CARTESIAN_POINT('Ctrl Pts',(-19.1776845594024,47.145647430115,-31.3179409276988));
#27454=CARTESIAN_POINT('Ctrl Pts',(-17.1603730062766,49.1281916417172,-31.1599924045062));
#27455=CARTESIAN_POINT('Ctrl Pts',(-17.7176648850087,51.9011779769217,-31.0020438813138));
#27456=CARTESIAN_POINT('Ctrl Pts',(-20.3442805984188,52.9504240621659,-30.8440953581213));
#27457=CARTESIAN_POINT('Ctrl Pts',(-22.6587475640635,51.3246103833355,-30.6861468349288));
#27458=CARTESIAN_POINT('Ctrl Pts',(-22.5626089755239,48.4978127561391,-30.5281983117364));
#27459=CARTESIAN_POINT('Ctrl Pts',(-20.1430307671055,47.0330026159906,-30.3702497885439));
#27460=CARTESIAN_POINT('Ctrl Pts',(-17.5937709122369,48.2582787667788,-30.2123012653514));
#27461=CARTESIAN_POINT('Ctrl Pts',(-17.2261657890932,51.0627205876685,-30.054352742159));
#27462=CARTESIAN_POINT('Ctrl Pts',(-19.3735117826252,52.9036259729115,-29.8964042189665));
#27463=CARTESIAN_POINT('Ctrl Pts',(-22.0888755890722,52.1119019982943,-29.7384556957741));
#27464=CARTESIAN_POINT('Ctrl Pts',(-22.9103194291884,49.4053807124462,-29.5805071725816));
#27465=CARTESIAN_POINT('Ctrl Pts',(-21.0930651562203,47.2379826500416,-29.4225586493891));
#27466=CARTESIAN_POINT('Ctrl Pts',(-18.2847619501882,47.5748217159901,-29.2646101261967));
#27467=CARTESIAN_POINT('Ctrl Pts',(-17.0316129172995,50.1104961733757,-29.1066616030041));
#27468=CARTESIAN_POINT('Ctrl Pts',(-18.4698101729106,52.5459871113712,-28.9487130798117));
#27469=CARTESIAN_POINT('Ctrl Pts',(-21.2953840060693,52.6731089673473,-28.7907645566192));
#27470=CARTESIAN_POINT('Ctrl Pts',(-22.946472558357,50.3766042232299,-28.6328160334268));
#27471=CARTESIAN_POINT('Ctrl Pts',(-21.9260840546788,47.738643880493,-28.4748675102343));
#27472=CARTESIAN_POINT('Ctrl Pts',(-19.159373718251,47.1509863618779,-28.3169189870418));
#27473=CARTESIAN_POINT('Ctrl Pts',(-17.1548336641381,49.1464428469726,-28.1589704638494));
#27474=CARTESIAN_POINT('Ctrl Pts',(-17.7299193966292,51.9157936691118,-28.0010219406569));
#27475=CARTESIAN_POINT('Ctrl Pts',(-20.3632181674306,52.9481525856191,-27.8430734174644));
#27476=CARTESIAN_POINT('Ctrl Pts',(-22.667198079343,51.3075113204235,-27.685124894272));
#27477=CARTESIAN_POINT('Ctrl Pts',(-22.5529105984627,48.4813891007891,-27.5271763710795));
#27478=CARTESIAN_POINT('Ctrl Pts',(-20.1239767479268,47.0321456078151,-27.3692278478871));
#27479=CARTESIAN_POINT('Ctrl Pts',(-17.5826368974691,48.2737646112518,-27.2112793246946));
#27480=CARTESIAN_POINT('Ctrl Pts',(-17.2330467571211,51.0805103684813,-27.0533308015021));
#27481=CARTESIAN_POINT('Ctrl Pts',(-19.3921687583624,52.9075869963002,-26.8953822783096));
#27482=CARTESIAN_POINT('Ctrl Pts',(-22.1023932793737,52.0984493755979,-26.7374337551172));
#27483=CARTESIAN_POINT('Ctrl Pts',(-22.9064409206452,49.3866986863416,-26.5794852319247));
#27484=CARTESIAN_POINT('Ctrl Pts',(-21.0753086362257,47.2310352075848,-26.4215367087322));
#27485=CARTESIAN_POINT('Ctrl Pts',(-18.269223407621,47.5858570068479,-26.2635881855397));
#27486=CARTESIAN_POINT('Ctrl Pts',(-17.0323872606667,50.1296101289755,-26.1056396623473));
#27487=CARTESIAN_POINT('Ctrl Pts',(-18.4861822213906,52.5556480488868,-25.9476911391548));
#27488=CARTESIAN_POINT('Ctrl Pts',(-21.3125358102357,52.6649590100811,-25.7897426159623));
#27489=CARTESIAN_POINT('Ctrl Pts',(-22.9488012008383,50.3572335482097,-25.6317940927699));
#27490=CARTESIAN_POINT('Ctrl Pts',(-21.9115810873935,47.7272072956741,-25.4738455695774));
#27491=CARTESIAN_POINT('Ctrl Pts',(-19.1409895978279,47.1546685981612,-25.3158970463849));
#27492=CARTESIAN_POINT('Ctrl Pts',(-17.1495670054614,49.1684308899942,-25.1579485231925));
#27493=CARTESIAN_POINT('Ctrl Pts',(-17.5453386170133,51.0029999971534,-25.0526495077308));
#27494=CARTESIAN_POINT('Ctrl Pts',(-18.0865340033349,51.6359872033749,-25.));
#27495=CARTESIAN_POINT('Ctrl Pts',(-17.4850543912228,50.0017607343381,-39.112583302492));
#27496=CARTESIAN_POINT('Ctrl Pts',(-17.4831411703387,50.2933091094334,-39.0941950563712));
#27497=CARTESIAN_POINT('Ctrl Pts',(-17.5300111809499,50.5842626429816,-39.0758068102504));
#27498=CARTESIAN_POINT('Ctrl Pts',(-17.6283799757769,50.856613782824,-39.0574185641297));
#27499=CARTESIAN_POINT('Ctrl Pts',(-17.9100310146906,51.63641373484,-39.0047690563988));
#27500=CARTESIAN_POINT('Ctrl Pts',(-18.6138691836584,52.2637112281982,-38.952119548668));
#27501=CARTESIAN_POINT('Ctrl Pts',(-19.4208044264721,52.4541504513905,-38.8994700409372));
#27502=CARTESIAN_POINT('Ctrl Pts',(-20.2277396692859,52.6445896745828,-38.8468205332064));
#27503=CARTESIAN_POINT('Ctrl Pts',(-21.1377719859456,52.3981706276091,-38.7941710254755));
#27504=CARTESIAN_POINT('Ctrl Pts',(-21.7383599640718,51.8265936072752,-38.7415215177447));
#27505=CARTESIAN_POINT('Ctrl Pts',(-22.338947942198,51.2550165869413,-38.6888720100139));
#27506=CARTESIAN_POINT('Ctrl Pts',(-22.6300915817907,50.3582815932472,-38.6362225022831));
#27507=CARTESIAN_POINT('Ctrl Pts',(-22.479801372793,49.5429148381292,-38.5835729945523));
#27508=CARTESIAN_POINT('Ctrl Pts',(-22.3295111637953,48.7275480830112,-38.5309234868215));
#27509=CARTESIAN_POINT('Ctrl Pts',(-21.7377871062073,47.9935495664694,-38.4782739790906));
#27510=CARTESIAN_POINT('Ctrl Pts',(-20.9728802968358,47.6736638228412,-38.4256244713598));
#27511=CARTESIAN_POINT('Ctrl Pts',(-20.2079734874642,47.353778079213,-38.372974963629));
#27512=CARTESIAN_POINT('Ctrl Pts',(-19.2698839263091,47.4480051084985,-38.3203254558981));
#27513=CARTESIAN_POINT('Ctrl Pts',(-18.5838792491135,47.913629791494,-38.2676759481673));
#27514=CARTESIAN_POINT('Ctrl Pts',(-17.9102782670879,48.370835484323,-38.2159783996089));
#27515=CARTESIAN_POINT('Ctrl Pts',(-17.4797286554972,49.1861297197598,-38.1642808510505));
#27516=CARTESIAN_POINT('Ctrl Pts',(-17.4784633668112,50.000273285299,-38.112583302492));
#27517=CARTESIAN_POINT('Origin',(-20.,50.,-32.));
#27518=CARTESIAN_POINT('Origin',(20.,50.,-25.));
#27519=CARTESIAN_POINT('',(17.2889091374855,49.9985242304765,-25.));
#27520=CARTESIAN_POINT('',(20.,50.,-25.));
#27521=CARTESIAN_POINT('Ctrl Pts',(17.2903182801745,49.9970484609529,-25.));
#27522=CARTESIAN_POINT('Ctrl Pts',(17.3003554510133,50.0895165684837,-25.));
#27523=CARTESIAN_POINT('Ctrl Pts',(17.3149872105963,50.1814113532663,-25.));
#27524=CARTESIAN_POINT('Ctrl Pts',(17.3341158855755,50.2723525936389,-25.));
#27525=CARTESIAN_POINT('Ctrl Pts',(17.3530415853084,50.3623288523453,-25.));
#27526=CARTESIAN_POINT('Ctrl Pts',(17.3763697243841,50.451372568364,-25.));
#27527=CARTESIAN_POINT('Ctrl Pts',(17.4040502467771,50.5390918450153,-25.));
#27528=CARTESIAN_POINT('Ctrl Pts',(17.4311163433268,50.6248640128022,-25.));
#27529=CARTESIAN_POINT('Ctrl Pts',(17.462344211455,50.7093705725007,-25.));
#27530=CARTESIAN_POINT('Ctrl Pts',(17.4977230419429,50.7922110937693,-25.));
#27531=CARTESIAN_POINT('Ctrl Pts',(17.5030373595978,50.8046547172202,-25.));
#27532=CARTESIAN_POINT('Ctrl Pts',(17.508445398048,50.8170606740681,-25.));
#27533=CARTESIAN_POINT('Ctrl Pts',(17.5139471830861,50.8294275242323,-25.));
#27534=CARTESIAN_POINT('Ctrl Pts',(17.5197445462543,50.8424587715735,-25.));
#27535=CARTESIAN_POINT('Ctrl Pts',(17.5256427668021,50.855439266843,-25.));
#27536=CARTESIAN_POINT('Ctrl Pts',(17.5316394080788,50.8683630331091,-25.));
#27537=CARTESIAN_POINT('Ctrl Pts',(17.5691316358145,50.949165063062,-25.));
#27538=CARTESIAN_POINT('Ctrl Pts',(17.6104933370969,51.0278095381119,-25.));
#27539=CARTESIAN_POINT('Ctrl Pts',(17.6556548012464,51.1039483466422,-25.));
#27540=CARTESIAN_POINT('Ctrl Pts',(17.7000564873693,51.1788062269566,-25.));
#27541=CARTESIAN_POINT('Ctrl Pts',(17.7481316148364,51.2512427099282,-25.));
#27542=CARTESIAN_POINT('Ctrl Pts',(17.7998501210591,51.3208927635814,-25.));
#27543=CARTESIAN_POINT('Ctrl Pts',(17.8499884667776,51.3884147924337,-25.));
#27544=CARTESIAN_POINT('Ctrl Pts',(17.9035514021835,51.4533185000313,-25.));
#27545=CARTESIAN_POINT('Ctrl Pts',(17.9605392204434,51.5152310005998,-25.));
#27546=CARTESIAN_POINT('Ctrl Pts',(17.9814440127658,51.5379423098947,-25.));
#27547=CARTESIAN_POINT('Ctrl Pts',(18.0028099126018,51.5602506790986,-25.));
#27548=CARTESIAN_POINT('Ctrl Pts',(18.0246377367992,51.5821361070304,-25.));
#27549=CARTESIAN_POINT('Ctrl Pts',(18.0437155989477,51.6012643157499,-25.));
#27550=CARTESIAN_POINT('Ctrl Pts',(18.0631463473053,51.62006941552,-25.));
#27551=CARTESIAN_POINT('Ctrl Pts',(18.0829198466036,51.6385462881155,-25.));
#27552=CARTESIAN_POINT('Origin',(20.,50.,-25.));
#27553=CARTESIAN_POINT('',(22.7115651190295,49.998177688036,-25.));
#27554=CARTESIAN_POINT('',(20.,50.,-25.));
#27555=CARTESIAN_POINT('Ctrl Pts',(22.710630238059,49.9963553760719,-25.));
#27556=CARTESIAN_POINT('Ctrl Pts',(22.7207573802718,49.904718898415,-25.));
#27557=CARTESIAN_POINT('Ctrl Pts',(22.7262776163321,49.8126183039993,-25.));
#27558=CARTESIAN_POINT('Ctrl Pts',(22.7270623951531,49.7204044776374,-25.));
#27559=CARTESIAN_POINT('Ctrl Pts',(22.7273484059302,49.6867973676626,-25.));
#27560=CARTESIAN_POINT('Ctrl Pts',(22.727004959792,49.653175122374,-25.));
#27561=CARTESIAN_POINT('Ctrl Pts',(22.7260241092612,49.6195545302368,-25.));
#27562=CARTESIAN_POINT('Ctrl Pts',(22.7254188474339,49.598807983854,-25.));
#27563=CARTESIAN_POINT('Ctrl Pts',(22.7245703770593,49.578055290145,-25.));
#27564=CARTESIAN_POINT('Ctrl Pts',(22.7234788618636,49.5573357485101,-25.));
#27565=CARTESIAN_POINT('Ctrl Pts',(22.7184418927117,49.46172215333,-25.));
#27566=CARTESIAN_POINT('Ctrl Pts',(22.7082329871324,49.3667044947841,-25.));
#27567=CARTESIAN_POINT('Ctrl Pts',(22.6927840010366,49.2726790977239,-25.));
#27568=CARTESIAN_POINT('Ctrl Pts',(22.6895875629464,49.2532249821753,-25.));
#27569=CARTESIAN_POINT('Ctrl Pts',(22.6861666387365,49.2338132767972,-25.));
#27570=CARTESIAN_POINT('Ctrl Pts',(22.6825203611591,49.2144474008277,-25.));
#27571=CARTESIAN_POINT('Ctrl Pts',(22.6655781463071,49.1244649942471,-25.));
#27572=CARTESIAN_POINT('Ctrl Pts',(22.6437749797271,49.0354721758651,-25.));
#27573=CARTESIAN_POINT('Ctrl Pts',(22.6174136918534,48.9477014940599,-25.));
#27574=CARTESIAN_POINT('Ctrl Pts',(22.590455165839,48.8579422903335,-25.));
#27575=CARTESIAN_POINT('Ctrl Pts',(22.5587294332582,48.7694605271934,-25.));
#27576=CARTESIAN_POINT('Ctrl Pts',(22.5225061276495,48.6825085791675,-25.));
#27577=CARTESIAN_POINT('Ctrl Pts',(22.5100294497312,48.6525590361409,-25.));
#27578=CARTESIAN_POINT('Ctrl Pts',(22.4970187421463,48.6227910672584,-25.));
#27579=CARTESIAN_POINT('Ctrl Pts',(22.4834836559862,48.5932153229631,-25.));
#27580=CARTESIAN_POINT('Ctrl Pts',(22.4768078375194,48.5786278798098,-25.));
#27581=CARTESIAN_POINT('Ctrl Pts',(22.4700044436617,48.5640872024162,-25.));
#27582=CARTESIAN_POINT('Ctrl Pts',(22.4630745736532,48.5495945909901,-25.));
#27583=CARTESIAN_POINT('Ctrl Pts',(22.4569730159819,48.5368342499856,-25.));
#27584=CARTESIAN_POINT('Ctrl Pts',(22.4507741704977,48.5241128967816,-25.));
#27585=CARTESIAN_POINT('Ctrl Pts',(22.4444842391951,48.5114418836784,-25.));
#27586=CARTESIAN_POINT('Ctrl Pts',(22.4016248337138,48.4251019759247,-25.));
#27587=CARTESIAN_POINT('Ctrl Pts',(22.3544763058254,48.3409633756465,-25.));
#27588=CARTESIAN_POINT('Ctrl Pts',(22.3033812187404,48.2592763321126,-25.));
#27589=CARTESIAN_POINT('Ctrl Pts',(22.2512764478704,48.1759750808731,-25.));
#27590=CARTESIAN_POINT('Ctrl Pts',(22.1950672860939,48.095222460128,-25.));
#27591=CARTESIAN_POINT('Ctrl Pts',(22.1350620407109,48.0172910149967,-25.));
#27592=CARTESIAN_POINT('Ctrl Pts',(22.0745784028941,47.9387382606202,-25.));
#27593=CARTESIAN_POINT('Ctrl Pts',(22.0102374503671,47.8630510071298,-25.));
#27594=CARTESIAN_POINT('Ctrl Pts',(21.9423056830507,47.7905278044699,-25.));
#27595=CARTESIAN_POINT('Ctrl Pts',(21.9053598556853,47.7510848482316,-25.));
#27596=CARTESIAN_POINT('Ctrl Pts',(21.8673510860636,47.7125781999077,-25.));
#27597=CARTESIAN_POINT('Ctrl Pts',(21.8283169663557,47.6750596468976,-25.));
#27598=CARTESIAN_POINT('Ctrl Pts',(21.8156599013896,47.662894014204,-25.));
#27599=CARTESIAN_POINT('Ctrl Pts',(21.8028950020426,47.6508322966046,-25.));
#27600=CARTESIAN_POINT('Ctrl Pts',(21.7900234751583,47.6388763339766,-25.));
#27601=CARTESIAN_POINT('Ctrl Pts',(21.7785389308687,47.6282086965192,-25.));
#27602=CARTESIAN_POINT('Ctrl Pts',(21.7669748807076,47.6176302985802,-25.));
#27603=CARTESIAN_POINT('Ctrl Pts',(21.7553377463642,47.6071469065118,-25.));
#27604=CARTESIAN_POINT('Ctrl Pts',(21.6795229583253,47.5388486361528,-25.));
#27605=CARTESIAN_POINT('Ctrl Pts',(21.6005419880646,47.4745177252953,-25.));
#27606=CARTESIAN_POINT('Ctrl Pts',(21.5187212121605,47.4144372276439,-25.));
#27607=CARTESIAN_POINT('Ctrl Pts',(21.4368280436309,47.3543035725284,-25.));
#27608=CARTESIAN_POINT('Ctrl Pts',(21.3520894649761,47.2984270171853,-25.));
#27609=CARTESIAN_POINT('Ctrl Pts',(21.2647877502657,47.2471175615949,-25.));
#27610=CARTESIAN_POINT('Ctrl Pts',(21.1792482856417,47.1968438255531,-25.));
#27611=CARTESIAN_POINT('Ctrl Pts',(21.0912474535113,47.1509539946296,-25.));
#27612=CARTESIAN_POINT('Ctrl Pts',(21.0010170240259,47.1097758121714,-25.));
#27613=CARTESIAN_POINT('Ctrl Pts',(20.9635971819417,47.0926986343979,-25.));
#27614=CARTESIAN_POINT('Ctrl Pts',(20.9257935259626,47.0764322950928,-25.));
#27615=CARTESIAN_POINT('Ctrl Pts',(20.8876212384296,47.0610024698252,-25.));
#27616=CARTESIAN_POINT('Ctrl Pts',(20.8571995126747,47.048705540742,-25.));
#27617=CARTESIAN_POINT('Ctrl Pts',(20.8265436358766,47.0369399483188,-25.));
#27618=CARTESIAN_POINT('Ctrl Pts',(20.7956658684167,47.0257030027424,-25.));
#27619=CARTESIAN_POINT('Ctrl Pts',(19.2062007174671,47.0307770462543,-25.));
#27620=CARTESIAN_POINT('Ctrl Pts',(19.1113557060478,47.0654717751014,-25.));
#27621=CARTESIAN_POINT('Ctrl Pts',(19.0185537598898,47.1051548199859,-25.));
#27622=CARTESIAN_POINT('Ctrl Pts',(18.9280360104757,47.1495064600839,-25.));
#27623=CARTESIAN_POINT('Ctrl Pts',(18.836253198687,47.1944779519955,-25.));
#27624=CARTESIAN_POINT('Ctrl Pts',(18.746818208596,47.2442501473846,-25.));
#27625=CARTESIAN_POINT('Ctrl Pts',(18.6600164517859,47.2985304009372,-25.));
#27626=CARTESIAN_POINT('Ctrl Pts',(18.6355002698107,47.3138612493285,-25.));
#27627=CARTESIAN_POINT('Ctrl Pts',(18.6111943852541,47.3295519227208,-25.));
#27628=CARTESIAN_POINT('Ctrl Pts',(18.5871058251638,47.3455962834916,-25.));
#27629=CARTESIAN_POINT('Ctrl Pts',(18.5677884079412,47.3584627898298,-25.));
#27630=CARTESIAN_POINT('Ctrl Pts',(18.5486086595491,47.3715583683707,-25.));
#27631=CARTESIAN_POINT('Ctrl Pts',(18.5295894598327,47.3848661134958,-25.));
#27632=CARTESIAN_POINT('Ctrl Pts',(18.4468808414566,47.4427373819723,-25.));
#27633=CARTESIAN_POINT('Ctrl Pts',(18.3671268101558,47.5046689052355,-25.));
#27634=CARTESIAN_POINT('Ctrl Pts',(18.2905938480462,47.5703640699442,-25.));
#27635=CARTESIAN_POINT('Ctrl Pts',(18.231599184729,47.6210045262486,-25.));
#27636=CARTESIAN_POINT('Ctrl Pts',(18.1745190969985,47.6738822270316,-25.));
#27637=CARTESIAN_POINT('Ctrl Pts',(18.1194932079197,47.7288730846741,-25.));
#27638=CARTESIAN_POINT('Ctrl Pts',(18.0902009127033,47.7581467313745,-25.));
#27639=CARTESIAN_POINT('Ctrl Pts',(18.0614910173884,47.7880193581185,-25.));
#27640=CARTESIAN_POINT('Ctrl Pts',(18.0333866071095,47.8184730778813,-25.));
#27641=CARTESIAN_POINT('Ctrl Pts',(18.0237499891656,47.8289152419193,-25.));
#27642=CARTESIAN_POINT('Ctrl Pts',(18.0141852981564,47.8394250112168,-25.));
#27643=CARTESIAN_POINT('Ctrl Pts',(18.0047000948839,47.8499940608166,-25.));
#27644=CARTESIAN_POINT('Ctrl Pts',(17.9389018416694,47.9233108872281,-25.));
#27645=CARTESIAN_POINT('Ctrl Pts',(17.8768356848677,47.9995741977793,-25.));
#27646=CARTESIAN_POINT('Ctrl Pts',(17.8187455012205,48.0785061517174,-25.));
#27647=CARTESIAN_POINT('Ctrl Pts',(17.7611817077828,48.1567228555884,-25.));
#27648=CARTESIAN_POINT('Ctrl Pts',(17.707521722539,48.2375608408771,-25.));
#27649=CARTESIAN_POINT('Ctrl Pts',(17.6580485957965,48.3207721465544,-25.));
#27650=CARTESIAN_POINT('Ctrl Pts',(17.6099912397688,48.4016021972458,-25.));
#27651=CARTESIAN_POINT('Ctrl Pts',(17.5658843324267,48.4846723754761,-25.));
#27652=CARTESIAN_POINT('Ctrl Pts',(17.5260350964086,48.5697657528252,-25.));
#27653=CARTESIAN_POINT('Ctrl Pts',(17.5052300089039,48.6141925810086,-25.));
#27654=CARTESIAN_POINT('Ctrl Pts',(17.4855863091861,48.659171009271,-25.));
#27655=CARTESIAN_POINT('Ctrl Pts',(17.4671534140155,48.7046704056706,-25.));
#27656=CARTESIAN_POINT('Ctrl Pts',(17.4600943600105,48.7220948359301,-25.));
#27657=CARTESIAN_POINT('Ctrl Pts',(17.4532129229748,48.7395956691933,-25.));
#27658=CARTESIAN_POINT('Ctrl Pts',(17.4465120404535,48.7571711764424,-25.));
#27659=CARTESIAN_POINT('Ctrl Pts',(17.441270606043,48.7709187489726,-25.));
#27660=CARTESIAN_POINT('Ctrl Pts',(17.4361395441369,48.784712508465,-25.));
#27661=CARTESIAN_POINT('Ctrl Pts',(17.4311253885978,48.798536919806,-25.));
#27662=CARTESIAN_POINT('Ctrl Pts',(17.3994429641943,48.8858877935106,-25.));
#27663=CARTESIAN_POINT('Ctrl Pts',(17.3723693458196,48.9746019981721,-25.));
#27664=CARTESIAN_POINT('Ctrl Pts',(17.3501558549811,49.0644566530551,-25.));
#27665=CARTESIAN_POINT('Ctrl Pts',(17.3451709794145,49.0846207180789,-25.));
#27666=CARTESIAN_POINT('Ctrl Pts',(17.340431057112,49.1048422545129,-25.));
#27667=CARTESIAN_POINT('Ctrl Pts',(17.335939289229,49.1251187994171,-25.));
#27668=CARTESIAN_POINT('Ctrl Pts',(17.3155161680488,49.217311972456,-25.));
#27669=CARTESIAN_POINT('Ctrl Pts',(17.300219006952,49.3106426726263,-25.));
#27670=CARTESIAN_POINT('Ctrl Pts',(17.2899369956297,49.4047153321239,-25.));
#27671=CARTESIAN_POINT('Ctrl Pts',(17.2792457471088,49.5025322037636,-25.));
#27672=CARTESIAN_POINT('Ctrl Pts',(17.2739768612926,49.6011525024422,-25.));
#27673=CARTESIAN_POINT('Ctrl Pts',(17.2740630915786,49.7001168903436,-25.));
#27674=CARTESIAN_POINT('Ctrl Pts',(17.2740904232784,49.731484812998,-25.));
#27675=CARTESIAN_POINT('Ctrl Pts',(17.2746561692793,49.7628871202482,-25.));
#27676=CARTESIAN_POINT('Ctrl Pts',(17.2757593065841,49.7943085770565,-25.));
#27677=CARTESIAN_POINT('Ctrl Pts',(17.2762349624895,49.8078570278432,-25.));
#27678=CARTESIAN_POINT('Ctrl Pts',(17.2768106643348,49.8214115392031,-25.));
#27679=CARTESIAN_POINT('Ctrl Pts',(17.27748594917,49.8349628018775,-25.));
#27680=CARTESIAN_POINT('Ctrl Pts',(17.280185572062,49.889137421273,-25.));
#27681=CARTESIAN_POINT('Ctrl Pts',(17.2844721284628,49.9431903973805,-25.));
#27682=CARTESIAN_POINT('Ctrl Pts',(17.2903182801745,49.9970484609529,-25.));
#27683=CARTESIAN_POINT('',(20.,50.,-25.));
#27684=CARTESIAN_POINT('Origin',(20.,50.,-25.));
#27685=CARTESIAN_POINT('Origin',(20.,50.,-25.));
#27686=CARTESIAN_POINT('',(20.,50.,-25.));
#27687=CARTESIAN_POINT('Ctrl Pts',(21.9134659966651,51.6359872033749,-25.));
#27688=CARTESIAN_POINT('Ctrl Pts',(21.9760669584728,51.57715767109,-25.));
#27689=CARTESIAN_POINT('Ctrl Pts',(22.0352443081274,51.5150279920012,-25.));
#27690=CARTESIAN_POINT('Ctrl Pts',(22.0909852410533,51.449982471831,-25.));
#27691=CARTESIAN_POINT('Ctrl Pts',(22.1343869490307,51.3993359088211,-25.));
#27692=CARTESIAN_POINT('Ctrl Pts',(22.1757048720029,51.346920405304,-25.));
#27693=CARTESIAN_POINT('Ctrl Pts',(22.2149216400472,51.2928987320259,-25.));
#27694=CARTESIAN_POINT('Ctrl Pts',(22.238544542541,51.2603578373004,-25.));
#27695=CARTESIAN_POINT('Ctrl Pts',(22.2614048485299,51.2272338518059,-25.));
#27696=CARTESIAN_POINT('Ctrl Pts',(22.2834967784221,51.1935599636263,-25.));
#27697=CARTESIAN_POINT('Ctrl Pts',(22.2954179674691,51.1753889487401,-25.));
#27698=CARTESIAN_POINT('Ctrl Pts',(22.3071167276197,51.1570553689352,-25.));
#27699=CARTESIAN_POINT('Ctrl Pts',(22.3185794803464,51.1385851146828,-25.));
#27700=CARTESIAN_POINT('Ctrl Pts',(22.3655670889394,51.0628726660144,-25.));
#27701=CARTESIAN_POINT('Ctrl Pts',(22.408638498604,50.9847977644774,-25.));
#27702=CARTESIAN_POINT('Ctrl Pts',(22.4477592672363,50.9047425113829,-25.));
#27703=CARTESIAN_POINT('Ctrl Pts',(22.4825528251087,50.8335422978156,-25.));
#27704=CARTESIAN_POINT('Ctrl Pts',(22.5142211416441,50.7607746036135,-25.));
#27705=CARTESIAN_POINT('Ctrl Pts',(22.5427166787335,50.686684346716,-25.));
#27706=CARTESIAN_POINT('Ctrl Pts',(22.5500219910964,50.667690057611,-25.));
#27707=CARTESIAN_POINT('Ctrl Pts',(22.5571186539646,50.6486087488088,-25.));
#27708=CARTESIAN_POINT('Ctrl Pts',(22.5640056073642,50.6294443637264,-25.));
#27709=CARTESIAN_POINT('Ctrl Pts',(22.5692938298803,50.6147287809691,-25.));
#27710=CARTESIAN_POINT('Ctrl Pts',(22.5744584523851,50.5999638327569,-25.));
#27711=CARTESIAN_POINT('Ctrl Pts',(22.5794944484737,50.5851652200462,-25.));
#27712=CARTESIAN_POINT('Ctrl Pts',(22.6091525619276,50.4980128619004,-25.));
#27713=CARTESIAN_POINT('Ctrl Pts',(22.6343958352894,50.4095773703735,-25.));
#27714=CARTESIAN_POINT('Ctrl Pts',(22.6551922384222,50.3202540828574,-25.));
#27715=CARTESIAN_POINT('Ctrl Pts',(22.6763398077743,50.2294224902284,-25.));
#27716=CARTESIAN_POINT('Ctrl Pts',(22.6928895667938,50.137672075038,-25.));
#27717=CARTESIAN_POINT('Ctrl Pts',(22.704766333404,50.0453852273788,-25.));
#27718=CARTESIAN_POINT('Ctrl Pts',(22.7068675349265,50.0290581182278,-25.));
#27719=CARTESIAN_POINT('Ctrl Pts',(22.7088223589801,50.012714154031,-25.));
#27720=CARTESIAN_POINT('Ctrl Pts',(22.710630238059,49.9963553760719,-25.));
#27721=CARTESIAN_POINT('Origin',(20.,50.,-42.2084234471774));
#27722=CARTESIAN_POINT('Ctrl Pts',(23.0767446582541,50.0019103494728,-39.7084234471775));
#27723=CARTESIAN_POINT('Ctrl Pts',(23.0776698137548,50.1251794436804,-39.7020198504182));
#27724=CARTESIAN_POINT('Ctrl Pts',(23.0151644123476,51.2610383915795,-39.642966745928));
#27725=CARTESIAN_POINT('Ctrl Pts',(21.6024147148416,53.2535259157778,-39.5312641337071));
#27726=CARTESIAN_POINT('Ctrl Pts',(18.1518494020808,53.1200733432643,-39.3733156105146));
#27727=CARTESIAN_POINT('Ctrl Pts',(16.376977963313,50.1582350183397,-39.2153670873222));
#27728=CARTESIAN_POINT('Ctrl Pts',(17.8869743722217,47.0526837548,-39.0574185641297));
#27729=CARTESIAN_POINT('Ctrl Pts',(21.3127949123184,46.6194980929628,-38.8994700409373));
#27730=CARTESIAN_POINT('Ctrl Pts',(22.9593110635881,48.5578259751719,-38.7831383352865));
#27731=CARTESIAN_POINT('Ctrl Pts',(23.076186491933,49.7844436463546,-38.7194561373665));
#27732=CARTESIAN_POINT('Ctrl Pts',(23.074254699799,49.9973154728993,-38.7084234471775));
#27733=CARTESIAN_POINT('Ctrl Pts',(23.0703066071761,49.9966560053347,-39.7915765528225));
#27734=CARTESIAN_POINT('Ctrl Pts',(23.0652969469962,50.6897753512944,-39.7557520197534));
#27735=CARTESIAN_POINT('Ctrl Pts',(22.4928178620874,52.4114019306593,-39.6672779789534));
#27736=CARTESIAN_POINT('Ctrl Pts',(19.6484751064271,53.6086153775441,-39.5261544304226));
#27737=CARTESIAN_POINT('Ctrl Pts',(16.7861446928906,51.6798052066136,-39.3682059072302));
#27738=CARTESIAN_POINT('Ctrl Pts',(16.8365147494583,48.2264371981741,-39.2102573840376));
#27739=CARTESIAN_POINT('Ctrl Pts',(19.7557254495835,46.3818721760905,-39.0523088608452));
#27740=CARTESIAN_POINT('Ctrl Pts',(22.5305076755622,47.6502487962456,-38.9127485837735));
#27741=CARTESIAN_POINT('Ctrl Pts',(23.0660295697572,49.3389604422763,-38.8258378144326));
#27742=CARTESIAN_POINT('Ctrl Pts',(23.0703815974152,50.0021496035415,-38.7915765528225));
#27743=CARTESIAN_POINT('Ctrl Pts',(18.086534003335,51.635987203375,-40.));
#27744=CARTESIAN_POINT('Ctrl Pts',(17.5453386170133,51.0029999971535,-39.9473504922692));
#27745=CARTESIAN_POINT('Ctrl Pts',(17.1495677130931,49.1684301437675,-39.8420514768075));
#27746=CARTESIAN_POINT('Ctrl Pts',(19.1409892366488,47.1546688770413,-39.6841029536151));
#27747=CARTESIAN_POINT('Ctrl Pts',(21.9115813032277,47.7272070111674,-39.5261544304226));
#27748=CARTESIAN_POINT('Ctrl Pts',(22.9488012025699,50.3572336945348,-39.3682059072301));
#27749=CARTESIAN_POINT('Ctrl Pts',(21.3125358856723,52.6649590021054,-39.2102573840377));
#27750=CARTESIAN_POINT('Ctrl Pts',(18.4861821603183,52.5556481671279,-39.0523088608452));
#27751=CARTESIAN_POINT('Ctrl Pts',(17.0323871881049,50.1296101053101,-38.8943603376527));
#27752=CARTESIAN_POINT('Ctrl Pts',(18.2692233551548,47.5858569554934,-38.7364118144602));
#27753=CARTESIAN_POINT('Ctrl Pts',(21.0753086682159,47.2310351225099,-38.5784632912678));
#27754=CARTESIAN_POINT('Ctrl Pts',(22.9064409998485,49.3866986741128,-38.4205147680753));
#27755=CARTESIAN_POINT('Ctrl Pts',(22.102393338019,52.098449431005,-38.2625662448829));
#27756=CARTESIAN_POINT('Ctrl Pts',(19.3921687412977,52.9075870780541,-38.1046177216904));
#27757=CARTESIAN_POINT('Ctrl Pts',(17.2330466807883,51.0805103975822,-37.9466691984979));
#27758=CARTESIAN_POINT('Ctrl Pts',(17.5826368306021,48.2737645639559,-37.7887206753054));
#27759=CARTESIAN_POINT('Ctrl Pts',(20.123976751384,47.0321455255811,-37.630772152113));
#27760=CARTESIAN_POINT('Ctrl Pts',(22.5529106689962,48.4813890589392,-37.4728236289205));
#27761=CARTESIAN_POINT('Ctrl Pts',(22.6671981530575,51.3075113564941,-37.314875105728));
#27762=CARTESIAN_POINT('Ctrl Pts',(20.3632181774645,52.948152667123,-37.1569265825356));
#27763=CARTESIAN_POINT('Ctrl Pts',(17.7299193338982,51.9157937220368,-36.9989780593431));
#27764=CARTESIAN_POINT('Ctrl Pts',(17.154833585512,49.1464428233941,-36.8410295361507));
#27765=CARTESIAN_POINT('Ctrl Pts',(19.159373695021,47.1509862831415,-36.6830810129581));
#27766=CARTESIAN_POINT('Ctrl Pts',(21.9260841079052,47.7386438180038,-36.5251324897658));
#27767=CARTESIAN_POINT('Ctrl Pts',(22.9464726397818,50.3766042336357,-36.3671839665732));
#27768=CARTESIAN_POINT('Ctrl Pts',(21.2953840418668,52.6731090412184,-36.2092354433808));
#27769=CARTESIAN_POINT('Ctrl Pts',(18.4698101306244,52.5459871817283,-36.0512869201882));
#27770=CARTESIAN_POINT('Ctrl Pts',(17.0316128352692,50.1104961764295,-35.8933383969959));
#27771=CARTESIAN_POINT('Ctrl Pts',(18.2847619027881,47.574821648971,-35.7353898738033));
#27772=CARTESIAN_POINT('Ctrl Pts',(21.0930651864267,47.2379825737144,-35.5774413506109));
#27773=CARTESIAN_POINT('Ctrl Pts',(22.910319509614,49.4053806960139,-35.4194928274184));
#27774=CARTESIAN_POINT('Ctrl Pts',(22.0888756467976,52.1119020566559,-35.261544304226));
#27775=CARTESIAN_POINT('Ctrl Pts',(19.3735117653125,52.9036260531522,-35.1035957810335));
#27776=CARTESIAN_POINT('Ctrl Pts',(17.2261657124394,51.0627206170365,-34.945647257841));
#27777=CARTESIAN_POINT('Ctrl Pts',(17.5937708457415,48.258278718647,-34.7876987346485));
#27778=CARTESIAN_POINT('Ctrl Pts',(20.143030771058,47.0330025339987,-34.6297502114561));
#27779=CARTESIAN_POINT('Ctrl Pts',(22.5626090463406,48.4978127146266,-34.4718016882636));
#27780=CARTESIAN_POINT('Ctrl Pts',(22.6587476375371,51.3246104199406,-34.3138531650712));
#27781=CARTESIAN_POINT('Ctrl Pts',(20.3442806079329,52.9504241436998,-34.1559046418787));
#27782=CARTESIAN_POINT('Ctrl Pts',(17.7176648219373,51.9011780294602,-33.9979561186862));
#27783=CARTESIAN_POINT('Ctrl Pts',(17.1603729278045,49.1281916176252,-33.8400075954937));
#27784=CARTESIAN_POINT('Ctrl Pts',(19.1776845366779,47.145647351236,-33.6820590723013));
#27785=CARTESIAN_POINT('Ctrl Pts',(21.9405645665512,47.7510578202695,-33.5241105491088));
#27786=CARTESIAN_POINT('Ctrl Pts',(22.9439937235359,50.3955157651801,-33.3661620259163));
#27787=CARTESIAN_POINT('Ctrl Pts',(21.2781933089123,52.6813715948702,-33.2082135027239));
#27788=CARTESIAN_POINT('Ctrl Pts',(18.4534938955901,52.5361093497221,-33.0502649795314));
#27789=CARTESIAN_POINT('Ctrl Pts',(17.0309645322794,50.0914338894602,-32.8923164563389));
#27790=CARTESIAN_POINT('Ctrl Pts',(18.300369328419,47.5638581024608,-32.7343679331465));
#27791=CARTESIAN_POINT('Ctrl Pts',(21.1107775625509,47.2450580820535,-32.576419409954));
#27792=CARTESIAN_POINT('Ctrl Pts',(22.9140775634904,49.4240801108775,-32.4184708867615));
#27793=CARTESIAN_POINT('Ctrl Pts',(22.0752720652759,52.1252711873571,-32.260522363569));
#27794=CARTESIAN_POINT('Ctrl Pts',(19.3548805020225,52.8995435154614,-32.1025738403766));
#27795=CARTESIAN_POINT('Ctrl Pts',(17.2193991671627,51.0448879237265,-31.9446253171841));
#27796=CARTESIAN_POINT('Ctrl Pts',(17.605004039285,48.2428642303784,-31.7866767939917));
#27797=CARTESIAN_POINT('Ctrl Pts',(20.162078908478,47.0339820984776,-31.6287282707991));
#27798=CARTESIAN_POINT('Ctrl Pts',(22.5722017607613,48.5142981905304,-31.4707797476067));
#27799=CARTESIAN_POINT('Ctrl Pts',(22.6501875065425,51.3416549276512,-31.3128312244142));
#27800=CARTESIAN_POINT('Ctrl Pts',(20.3253288419512,52.9525739464609,-31.1548827012218));
#27801=CARTESIAN_POINT('Ctrl Pts',(17.7055044107922,51.8864839664918,-30.9969341780293));
#27802=CARTESIAN_POINT('Ctrl Pts',(17.1660293464391,49.1099763489209,-30.8389856548369));
#27803=CARTESIAN_POINT('Ctrl Pts',(19.1960292823484,47.1404261069377,-30.6810371316443));
#27804=CARTESIAN_POINT('Ctrl Pts',(21.9549650162884,47.7635645437854,-30.5230886084519));
#27805=CARTESIAN_POINT('Ctrl Pts',(22.9413934275329,50.4144109906734,-30.3651400852594));
#27806=CARTESIAN_POINT('Ctrl Pts',(21.2609498764708,52.6895235960579,-30.207191562067));
#27807=CARTESIAN_POINT('Ctrl Pts',(18.437241422469,52.5261269550601,-30.0492430388745));
#27808=CARTESIAN_POINT('Ctrl Pts',(17.030438641562,50.0723678325863,-29.891294515682));
#27809=CARTESIAN_POINT('Ctrl Pts',(18.3160468292225,47.5529949972773,-29.7333459924896));
#27810=CARTESIAN_POINT('Ctrl Pts',(21.1284441417105,47.2522471756388,-29.5753974692971));
#27811=CARTESIAN_POINT('Ctrl Pts',(22.9177154709785,49.4428032707346,-29.4174489461046));
#27812=CARTESIAN_POINT('Ctrl Pts',(22.0615829210316,52.1385526938618,-29.2595004229121));
#27813=CARTESIAN_POINT('Ctrl Pts',(19.3362758367626,52.8953414306466,-29.1015518997197));
#27814=CARTESIAN_POINT('Ctrl Pts',(17.2127472651087,51.0270121500097,-28.9436033765272));
#27815=CARTESIAN_POINT('Ctrl Pts',(17.61633597759,48.2275221882877,-28.7856548533347));
#27816=CARTESIAN_POINT('Ctrl Pts',(20.1811203635866,47.0350839506389,-28.6277063301423));
#27817=CARTESIAN_POINT('Ctrl Pts',(22.5816884239278,48.5308449217582,-28.4697578069498));
#27818=CARTESIAN_POINT('Ctrl Pts',(22.6415181098295,51.358644118678,-28.3118092837574));
#27819=CARTESIAN_POINT('Ctrl Pts',(20.3063636616365,52.9546020170924,-28.1538607605649));
#27820=CARTESIAN_POINT('Ctrl Pts',(17.6934386031563,51.8717121215775,-27.9959122373724));
#27821=CARTESIAN_POINT('Ctrl Pts',(17.1718026041603,49.0917977813112,-27.8379637141799));
#27822=CARTESIAN_POINT('Ctrl Pts',(19.2144071844416,47.1353227504398,-27.6800151909875));
#27823=CARTESIAN_POINT('Ctrl Pts',(21.9692848456041,47.7761634974712,-27.522066667795));
#27824=CARTESIAN_POINT('Ctrl Pts',(22.9386718945708,50.4332890849004,-27.3641181446025));
#27825=CARTESIAN_POINT('Ctrl Pts',(21.2436543845446,52.6975647992193,-27.2061696214101));
#27826=CARTESIAN_POINT('Ctrl Pts',(18.421053522611,52.5160402297565,-27.0482210982176));
#27827=CARTESIAN_POINT('Ctrl Pts',(17.03003490355,50.053299149001,-26.8902725750251));
#27828=CARTESIAN_POINT('Ctrl Pts',(18.3317943187318,47.5422320705639,-26.7323240518327));
#27829=CARTESIAN_POINT('Ctrl Pts',(21.1460630808652,47.2595509728877,-26.5743755286402));
#27830=CARTESIAN_POINT('Ctrl Pts',(22.9212353010978,49.4615465871111,-26.4164270054477));
#27831=CARTESIAN_POINT('Ctrl Pts',(22.0478043609502,52.1517516355771,-26.2584784822553));
#27832=CARTESIAN_POINT('Ctrl Pts',(19.3177073307994,52.8910088097876,-26.1005299590628));
#27833=CARTESIAN_POINT('Ctrl Pts',(17.206192773396,51.0091162540841,-25.9425814358703));
#27834=CARTESIAN_POINT('Ctrl Pts',(17.6278010459406,48.2122089878618,-25.7846329126778));
#27835=CARTESIAN_POINT('Ctrl Pts',(20.2000849682644,47.0363961109221,-25.6266843894854));
#27836=CARTESIAN_POINT('Ctrl Pts',(22.5912067713758,48.5472769011073,-25.4687358662929));
#27837=CARTESIAN_POINT('Ctrl Pts',(22.6324648056073,51.3759264122866,-25.3107873431004));
#27838=CARTESIAN_POINT('Ctrl Pts',(20.287933589965,52.9558121213478,-25.152838819908));
#27839=CARTESIAN_POINT('Ctrl Pts',(17.6803739092466,51.8582635684763,-24.9948902967155));
#27840=CARTESIAN_POINT('Ctrl Pts',(17.1799175193219,49.0706951790677,-24.836941773523));
#27841=CARTESIAN_POINT('Ctrl Pts',(18.5452496035378,47.7830036573307,-24.7316427580614));
#27842=CARTESIAN_POINT('Ctrl Pts',(19.3498000020249,47.5679131979649,-24.6789932503306));
#27843=CARTESIAN_POINT('Ctrl Pts',(17.9456684496579,51.7564253212269,-40.1070022498898));
#27844=CARTESIAN_POINT('Ctrl Pts',(17.3646313374449,51.0768388582481,-40.054352742159));
#27845=CARTESIAN_POINT('Ctrl Pts',(16.9397245682378,49.1072116280355,-39.9490537266973));
#27846=CARTESIAN_POINT('Ctrl Pts',(19.0777505760168,46.9452012697107,-39.7911052035049));
#27847=CARTESIAN_POINT('Ctrl Pts',(22.0523081095296,47.5598885203642,-39.6331566803124));
#27848=CARTESIAN_POINT('Ctrl Pts',(23.1658860709749,50.3835325272606,-39.47520815712));
#27849=CARTESIAN_POINT('Ctrl Pts',(21.4091621620621,52.8611479733296,-39.3172596339275));
#27850=CARTESIAN_POINT('Ctrl Pts',(18.3747379075725,52.7437898925067,-39.159311110735));
#27851=CARTESIAN_POINT('Ctrl Pts',(16.8139174465076,50.1391517429866,-39.0013625875426));
#27852=CARTESIAN_POINT('Ctrl Pts',(18.1418070275104,47.4081325552623,-38.84341406435));
#27853=CARTESIAN_POINT('Ctrl Pts',(21.1544707495834,47.0271894459942,-38.6854655411577));
#27854=CARTESIAN_POINT('Ctrl Pts',(23.1204073945411,49.3415486526373,-38.5275170179651));
#27855=CARTESIAN_POINT('Ctrl Pts',(22.2571673460876,52.2529330964984,-38.3695684947727));
#27856=CARTESIAN_POINT('Ctrl Pts',(19.3474214152682,53.1216378447405,-38.2116199715801));
#27857=CARTESIAN_POINT('Ctrl Pts',(17.0293490911846,51.1600554199,-38.0536714483878));
#27858=CARTESIAN_POINT('Ctrl Pts',(17.4046753711933,48.1466825510542,-37.8957229251952));
#27859=CARTESIAN_POINT('Ctrl Pts',(20.1331036727703,46.8136579932703,-37.7377744020028));
#27860=CARTESIAN_POINT('Ctrl Pts',(22.7408508652176,48.3695919476212,-37.5798258788103));
#27861=CARTESIAN_POINT('Ctrl Pts',(22.8635519661128,51.4037677370582,-37.4218773556178));
#27862=CARTESIAN_POINT('Ctrl Pts',(20.3899575758982,53.1651897916408,-37.2639288324254));
#27863=CARTESIAN_POINT('Ctrl Pts',(17.5628005188895,52.0568306382172,-37.1059803092329));
#27864=CARTESIAN_POINT('Ctrl Pts',(16.9453781036908,49.0836056449508,-36.9480317860405));
#27865=CARTESIAN_POINT('Ctrl Pts',(19.0974884615793,46.9412475705864,-36.790083262848));
#27866=CARTESIAN_POINT('Ctrl Pts',(22.0678785817874,47.5721672821295,-36.6321347396555));
#27867=CARTESIAN_POINT('Ctrl Pts',(23.1633860840345,50.4043290868502,-36.474186216463));
#27868=CARTESIAN_POINT('Ctrl Pts',(21.3907476336944,52.8698980020813,-36.3162376932706));
#27869=CARTESIAN_POINT('Ctrl Pts',(18.3571606016773,52.7334176846136,-36.1582891700781));
#27870=CARTESIAN_POINT('Ctrl Pts',(16.8130860873592,50.1186306847505,-36.0003406468856));
#27871=CARTESIAN_POINT('Ctrl Pts',(18.1584894920566,47.396284851464,-35.8423921236932));
#27872=CARTESIAN_POINT('Ctrl Pts',(21.1735344672812,47.034648354712,-35.6844436005007));
#27873=CARTESIAN_POINT('Ctrl Pts',(23.1245714324667,49.3616060077629,-35.5264950773082));
#27874=CARTESIAN_POINT('Ctrl Pts',(22.2426545093755,52.2673760776425,-35.3685465541158));
#27875=CARTESIAN_POINT('Ctrl Pts',(19.3273909498889,53.1173852170784,-35.2105980309233));
#27876=CARTESIAN_POINT('Ctrl Pts',(17.0219615596577,51.1409559911606,-35.0526495077308));
#27877=CARTESIAN_POINT('Ctrl Pts',(17.4166290503403,48.1300566686725,-34.8947009845384));
#27878=CARTESIAN_POINT('Ctrl Pts',(20.1535604114034,46.8145780929399,-34.7367524613459));
#27879=CARTESIAN_POINT('Ctrl Pts',(22.7512632177759,48.3872246801124,-34.5788039381534));
#27880=CARTESIAN_POINT('Ctrl Pts',(22.8544793404793,51.4221255994822,-34.420855414961));
#27881=CARTESIAN_POINT('Ctrl Pts',(20.3696258602349,53.1676284897966,-34.2629068917685));
#27882=CARTESIAN_POINT('Ctrl Pts',(17.5496438541779,52.0411389674781,-34.104958368576));
#27883=CARTESIAN_POINT('Ctrl Pts',(16.9513252413244,49.0640108217826,-33.9470098453835));
#27884=CARTESIAN_POINT('Ctrl Pts',(19.1171473109107,46.9355155971529,-33.7890613221911));
#27885=CARTESIAN_POINT('Ctrl Pts',(22.0834250629434,47.5854951785045,-33.6311127989986));
#27886=CARTESIAN_POINT('Ctrl Pts',(23.1607246749144,50.4246328476615,-33.4731642758061));
#27887=CARTESIAN_POINT('Ctrl Pts',(21.3722913532361,52.8787688284681,-33.3152157526137));
#27888=CARTESIAN_POINT('Ctrl Pts',(18.3396431979335,52.7228126662988,-33.1572672294212));
#27889=CARTESIAN_POINT('Ctrl Pts',(16.8123900575951,50.0981650702003,-32.9993187062287));
#27890=CARTESIAN_POINT('Ctrl Pts',(18.1752459052613,47.3845141905069,-32.8413701830363));
#27891=CARTESIAN_POINT('Ctrl Pts',(21.1925507932399,47.0422447478757,-32.6834216598438));
#27892=CARTESIAN_POINT('Ctrl Pts',(23.1286061467808,49.381682036286,-32.5254731366513));
#27893=CARTESIAN_POINT('Ctrl Pts',(22.2280494592902,52.281729417105,-32.3675246134589));
#27894=CARTESIAN_POINT('Ctrl Pts',(19.3073880901224,53.1130021310981,-32.2095760902664));
#27895=CARTESIAN_POINT('Ctrl Pts',(17.0146968748016,51.1218104905046,-32.0516275670739));
#27896=CARTESIAN_POINT('Ctrl Pts',(17.4286892092078,48.1135073964944,-31.8936790438815));
#27897=CARTESIAN_POINT('Ctrl Pts',(20.1740108347427,46.8156297710037,-31.735730520689));
#27898=CARTESIAN_POINT('Ctrl Pts',(22.7615621287167,48.4049237839014,-31.5777819974965));
#27899=CARTESIAN_POINT('Ctrl Pts',(22.8452890296988,51.4404248898854,-31.4198334743041));
#27900=CARTESIAN_POINT('Ctrl Pts',(20.3492789030071,53.1699365567532,-31.2618849511116));
#27901=CARTESIAN_POINT('Ctrl Pts',(17.5365882177965,52.025363156875,-31.1039364279191));
#27902=CARTESIAN_POINT('Ctrl Pts',(16.9573980742272,49.0444545812943,-30.9459879047267));
#27903=CARTESIAN_POINT('Ctrl Pts',(19.1368425602015,46.9299099752538,-30.7880393815342));
#27904=CARTESIAN_POINT('Ctrl Pts',(22.0988856450943,47.5989226220833,-30.6300908583417));
#27905=CARTESIAN_POINT('Ctrl Pts',(23.1579329503013,50.4449191020027,-30.4721423351493));
#27906=CARTESIAN_POINT('Ctrl Pts',(21.3537784936595,52.8875209637386,-30.3141938119568));
#27907=CARTESIAN_POINT('Ctrl Pts',(18.3221942501278,52.7120953876339,-30.1562452887643));
#27908=CARTESIAN_POINT('Ctrl Pts',(16.8118254518511,50.0776954082126,-29.9982967655718));
#27909=CARTESIAN_POINT('Ctrl Pts',(18.192077552433,47.372851365167,-29.8403482423794));
#27910=CARTESIAN_POINT('Ctrl Pts',(21.2115179507527,47.0499630882047,-29.6823997191869));
#27911=CARTESIAN_POINT('Ctrl Pts',(23.1325118697688,49.4017835578618,-29.5244511959945));
#27912=CARTESIAN_POINT('Ctrl Pts',(22.2133525475253,52.2959886816523,-29.3665026728019));
#27913=CARTESIAN_POINT('Ctrl Pts',(19.2874137864799,53.1084906971728,-29.2085541496095));
#27914=CARTESIAN_POINT('Ctrl Pts',(17.0075552729738,51.1026187379482,-29.050605626417));
#27915=CARTESIAN_POINT('Ctrl Pts',(17.4408553822296,48.0970359038373,-28.8926571032246));
#27916=CARTESIAN_POINT('Ctrl Pts',(20.1944540838321,46.8168127393254,-28.7347085800321));
#27917=CARTESIAN_POINT('Ctrl Pts',(22.7717471811213,48.4226886525094,-28.5767600568397));
#27918=CARTESIAN_POINT('Ctrl Pts',(22.8359814092754,51.4586647913009,-28.4188115336471));
#27919=CARTESIAN_POINT('Ctrl Pts',(20.3289175439099,53.1721139299031,-28.2608630104547));
#27920=CARTESIAN_POINT('Ctrl Pts',(17.5236341494462,52.0095038381744,-28.1029144872622));
#27921=CARTESIAN_POINT('Ctrl Pts',(16.9635963476774,49.024937743762,-27.9449659640698));
#27922=CARTESIAN_POINT('Ctrl Pts',(19.1565734068249,46.9244309198201,-27.7870174408773));
#27923=CARTESIAN_POINT('Ctrl Pts',(22.1142596717088,47.6124490856331,-27.6290689176848));
#27924=CARTESIAN_POINT('Ctrl Pts',(23.1550110635058,50.4651869639081,-27.4711203944923));
#27925=CARTESIAN_POINT('Ctrl Pts',(21.3352097420827,52.8961541442528,-27.3131718712999));
#27926=CARTESIAN_POINT('Ctrl Pts',(18.3048146293401,52.7012660977134,-27.1552233481074));
#27927=CARTESIAN_POINT('Ctrl Pts',(16.8113919914512,50.0572229261403,-26.9972748249149));
#27928=CARTESIAN_POINT('Ctrl Pts',(18.2089843407397,47.3612960932364,-26.8393263017225));
#27929=CARTESIAN_POINT('Ctrl Pts',(21.2304339610984,47.0578045764528,-26.68137777853));
#27930=CARTESIAN_POINT('Ctrl Pts',(23.1362908227675,49.4219067198399,-26.5234292553375));
#27931=CARTESIAN_POINT('Ctrl Pts',(22.1985596373075,52.3101593031548,-26.3654807321451));
#27932=CARTESIAN_POINT('Ctrl Pts',(19.2674783041096,53.1038391173999,-26.2075322089526));
#27933=CARTESIAN_POINT('Ctrl Pts',(17.0005182526424,51.083405381826,-26.0495836857601));
#27934=CARTESIAN_POINT('Ctrl Pts',(17.4531644860655,48.0805953761109,-25.8916351625676));
#27935=CARTESIAN_POINT('Ctrl Pts',(20.2148148249151,46.818221498234,-25.7336866393752));
#27936=CARTESIAN_POINT('Ctrl Pts',(22.7819662503411,48.4403303214338,-25.5757381161827));
#27937=CARTESIAN_POINT('Ctrl Pts',(22.8262616188369,51.4772193729263,-25.4177895929902));
#27938=CARTESIAN_POINT('Ctrl Pts',(20.3091306870879,53.1734131196224,-25.2598410697978));
#27939=CARTESIAN_POINT('Ctrl Pts',(17.5096076588051,51.995065229393,-25.1018925466053));
#27940=CARTESIAN_POINT('Ctrl Pts',(16.9723086667225,49.0022816099927,-24.9439440234128));
#27941=CARTESIAN_POINT('Ctrl Pts',(18.438153778257,47.6197928044311,-24.8386450079512));
#27942=CARTESIAN_POINT('Ctrl Pts',(19.301933573839,47.3888678140614,-24.7859955002204));
#27943=CARTESIAN_POINT('Ctrl Pts',(17.8048028959809,51.8768634390788,-40.2140044997796));
#27944=CARTESIAN_POINT('Ctrl Pts',(17.1839240578764,51.1506777193428,-40.1613549920488));
#27945=CARTESIAN_POINT('Ctrl Pts',(16.7298814233824,49.0459931123036,-40.0560559765871));
#27946=CARTESIAN_POINT('Ctrl Pts',(19.0145119153848,46.7357336623799,-39.8981074533947));
#27947=CARTESIAN_POINT('Ctrl Pts',(22.1930349158314,47.392570029561,-39.7401589302022));
#27948=CARTESIAN_POINT('Ctrl Pts',(23.3829709393799,50.4098313599865,-39.5822104070097));
#27949=CARTESIAN_POINT('Ctrl Pts',(21.5057884384518,53.0573369445537,-39.4242618838173));
#27950=CARTESIAN_POINT('Ctrl Pts',(18.2632936548267,52.9319316178855,-39.2663133606248));
#27951=CARTESIAN_POINT('Ctrl Pts',(16.5954477049103,50.1486933806631,-39.1083648374324));
#27952=CARTESIAN_POINT('Ctrl Pts',(18.014390699866,47.2304081550311,-38.9504163142398));
#27953=CARTESIAN_POINT('Ctrl Pts',(21.2336328309509,46.8233437694785,-38.7924677910474));
#27954=CARTESIAN_POINT('Ctrl Pts',(23.3343737892337,49.2963986311619,-38.6345192678549));
#27955=CARTESIAN_POINT('Ctrl Pts',(22.4119413541563,52.4074167619917,-38.4765707446625));
#27956=CARTESIAN_POINT('Ctrl Pts',(19.3026740892386,53.3356886114267,-38.31862222147));
#27957=CARTESIAN_POINT('Ctrl Pts',(16.8256515015809,51.2396004422179,-38.1606736982775));
#27958=CARTESIAN_POINT('Ctrl Pts',(17.2267139117844,48.0196005381524,-38.0027251750851));
#27959=CARTESIAN_POINT('Ctrl Pts',(20.1422305941565,46.5951704609596,-37.8447766518926));
#27960=CARTESIAN_POINT('Ctrl Pts',(22.9287910614389,48.257794836303,-37.6868281287001));
#27961=CARTESIAN_POINT('Ctrl Pts',(23.0599057791681,51.5000241176224,-37.5288796055076));
#27962=CARTESIAN_POINT('Ctrl Pts',(20.4166969743319,53.3822269161586,-37.3709310823152));
#27963=CARTESIAN_POINT('Ctrl Pts',(17.3956817038809,52.1978675543976,-37.2129825591227));
#27964=CARTESIAN_POINT('Ctrl Pts',(16.7359226218695,49.0207684665076,-37.0550340359303));
#27965=CARTESIAN_POINT('Ctrl Pts',(19.0356032281376,46.7315088580311,-36.8970855127378));
#27966=CARTESIAN_POINT('Ctrl Pts',(22.2096730556696,47.4056907462554,-36.7391369895453));
#27967=CARTESIAN_POINT('Ctrl Pts',(23.3802995282873,50.4320539400645,-36.5811884663528));
#27968=CARTESIAN_POINT('Ctrl Pts',(21.486111225522,53.0666869629442,-36.4232399431604));
#27969=CARTESIAN_POINT('Ctrl Pts',(18.2445110727302,52.9208481874989,-36.2652914199679));
#27970=CARTESIAN_POINT('Ctrl Pts',(16.5945593394492,50.1267651930716,-36.1073428967755));
#27971=CARTESIAN_POINT('Ctrl Pts',(18.0322170813251,47.2177480539569,-35.949394373583));
#27972=CARTESIAN_POINT('Ctrl Pts',(21.2540037481356,46.8313141357098,-35.7914458503905));
#27973=CARTESIAN_POINT('Ctrl Pts',(23.3388233553195,49.3178313195118,-35.6334973271981));
#27974=CARTESIAN_POINT('Ctrl Pts',(22.3964333719533,52.422850098629,-35.4755488040055));
#27975=CARTESIAN_POINT('Ctrl Pts',(19.2812701344654,53.3311443810046,-35.3176002808131));
#27976=CARTESIAN_POINT('Ctrl Pts',(16.817757406876,51.2191913652847,-35.1596517576206));
#27977=CARTESIAN_POINT('Ctrl Pts',(17.2394872549391,48.0018346186981,-35.0017032344282));
#27978=CARTESIAN_POINT('Ctrl Pts',(20.1640900517487,46.596153651881,-34.8437547112357));
#27979=CARTESIAN_POINT('Ctrl Pts',(22.9399173892113,48.2766366455985,-34.6858061880432));
#27980=CARTESIAN_POINT('Ctrl Pts',(23.0502110434214,51.5196407790236,-34.5278576648508));
#27981=CARTESIAN_POINT('Ctrl Pts',(20.3949711125369,53.3848328358937,-34.3699091416583));
#27982=CARTESIAN_POINT('Ctrl Pts',(17.3816228864185,52.1810999054958,-34.2119606184658));
#27983=CARTESIAN_POINT('Ctrl Pts',(16.7422775548443,48.9998300259402,-34.0540120952734));
#27984=CARTESIAN_POINT('Ctrl Pts',(19.0566100851434,46.7253838430697,-33.8960635720809));
#27985=CARTESIAN_POINT('Ctrl Pts',(22.2262855593357,47.4199325367396,-33.7381150488884));
#27986=CARTESIAN_POINT('Ctrl Pts',(23.3774556262928,50.4537499301427,-33.580166525696));
#27987=CARTESIAN_POINT('Ctrl Pts',(21.4663893975598,53.0761660620659,-33.4222180025035));
#27988=CARTESIAN_POINT('Ctrl Pts',(18.2257925002768,52.9095159828755,-33.264269479311));
#27989=CARTESIAN_POINT('Ctrl Pts',(16.5938155829109,50.1048962509405,-33.1063209561186));
#27990=CARTESIAN_POINT('Ctrl Pts',(18.0501224821035,47.205170278553,-32.9483724329261));
#27991=CARTESIAN_POINT('Ctrl Pts',(21.2743240239289,46.8394314136979,-32.7904239097336));
#27992=CARTESIAN_POINT('Ctrl Pts',(23.3431347300711,49.3392839616946,-32.6324753865411));
#27993=CARTESIAN_POINT('Ctrl Pts',(22.3808268533046,52.4381876468528,-32.4745268633487));
#27994=CARTESIAN_POINT('Ctrl Pts',(19.2598956782223,53.3264607467349,-32.3165783401562));
#27995=CARTESIAN_POINT('Ctrl Pts',(16.8099945824404,51.1987330572828,-32.1586298169637));
#27996=CARTESIAN_POINT('Ctrl Pts',(17.2523743791307,47.9841505626103,-32.0006812937713));
#27997=CARTESIAN_POINT('Ctrl Pts',(20.1859427610074,46.5972774435298,-31.8427327705788));
#27998=CARTESIAN_POINT('Ctrl Pts',(22.9509224966721,48.2955493772724,-31.6847842473863));
#27999=CARTESIAN_POINT('Ctrl Pts',(23.040390552855,51.5391948521197,-31.5268357241939));
#28000=CARTESIAN_POINT('Ctrl Pts',(20.373228964063,53.3872991670454,-31.3688872010014));
#28001=CARTESIAN_POINT('Ctrl Pts',(17.3676720248009,52.1642423472583,-31.210938677809));
#28002=CARTESIAN_POINT('Ctrl Pts',(16.7487668020154,48.9789328136677,-31.0529901546164));
#28003=CARTESIAN_POINT('Ctrl Pts',(19.0776558380546,46.7193938435699,-30.895041631424));
#28004=CARTESIAN_POINT('Ctrl Pts',(22.2428062739001,47.4342807003812,-30.7370931082315));
#28005=CARTESIAN_POINT('Ctrl Pts',(23.3744724730697,50.4754272133319,-30.5791445850391));
#28006=CARTESIAN_POINT('Ctrl Pts',(21.4466071108482,53.0855183314193,-30.4211960618466));
#28007=CARTESIAN_POINT('Ctrl Pts',(18.2071470777866,52.8980638202076,-30.2632475386541));
#28008=CARTESIAN_POINT('Ctrl Pts',(16.5932122621402,50.0830229838389,-30.1052990154616));
#28009=CARTESIAN_POINT('Ctrl Pts',(18.0681082756436,47.1927077330565,-29.9473504922692));
#28010=CARTESIAN_POINT('Ctrl Pts',(21.2945917597949,46.8476790007708,-29.7894019690767));
#28011=CARTESIAN_POINT('Ctrl Pts',(23.3473082685591,49.3607638449891,-29.6314534458843));
#28012=CARTESIAN_POINT('Ctrl Pts',(22.365122174019,52.4534246694427,-29.4735049226918));
#28013=CARTESIAN_POINT('Ctrl Pts',(19.2385517361972,53.3216399636991,-29.3155563994993));
#28014=CARTESIAN_POINT('Ctrl Pts',(16.8023632808387,51.1782253258867,-29.1576078763069));
#28015=CARTESIAN_POINT('Ctrl Pts',(17.2653747868691,47.9665496193868,-28.9996593531143));
#28016=CARTESIAN_POINT('Ctrl Pts',(20.2077878040777,46.598541528012,-28.8417108299219));
#28017=CARTESIAN_POINT('Ctrl Pts',(22.9618059383148,48.3145323832604,-28.6837623067294));
#28018=CARTESIAN_POINT('Ctrl Pts',(23.0304447087213,51.5586854639238,-28.525813783537));
#28019=CARTESIAN_POINT('Ctrl Pts',(20.3514714261833,53.3896258427139,-28.3678652603445));
#28020=CARTESIAN_POINT('Ctrl Pts',(17.3538296957362,52.1472955547711,-28.209916737152));
#28021=CARTESIAN_POINT('Ctrl Pts',(16.7553900911946,48.9580777062127,-28.0519682139596));
#28022=CARTESIAN_POINT('Ctrl Pts',(19.0987396292081,46.7135390892003,-27.8940196907671));
#28023=CARTESIAN_POINT('Ctrl Pts',(22.2592344978135,47.4487346737953,-27.7360711675746));
#28024=CARTESIAN_POINT('Ctrl Pts',(23.3713502324408,50.4970848429156,-27.5781226443821));
#28025=CARTESIAN_POINT('Ctrl Pts',(21.4267650996209,53.0947434892864,-27.4201741211897));
#28026=CARTESIAN_POINT('Ctrl Pts',(18.1885757360692,52.8864919656703,-27.2622255979972));
#28027=CARTESIAN_POINT('Ctrl Pts',(16.5927490793524,50.0611467032797,-27.1042770748047));
#28028=CARTESIAN_POINT('Ctrl Pts',(18.0861743627476,47.1803601159088,-26.9463285516123));
#28029=CARTESIAN_POINT('Ctrl Pts',(21.3148048413315,46.8560581800179,-26.7883800284198));
#28030=CARTESIAN_POINT('Ctrl Pts',(23.3513463444372,49.3822668525686,-26.6304315052273));
#28031=CARTESIAN_POINT('Ctrl Pts',(22.3493149136648,52.4685669707326,-26.4724829820349));
#28032=CARTESIAN_POINT('Ctrl Pts',(19.2172492774196,53.3166694250122,-26.3145344588424));
#28033=CARTESIAN_POINT('Ctrl Pts',(16.7948437318888,51.1576945095679,-26.1565859356499));
#28034=CARTESIAN_POINT('Ctrl Pts',(17.2785279261903,47.94898176436,-25.9986374124574));
#28035=CARTESIAN_POINT('Ctrl Pts',(20.2295446815659,46.6000468855458,-25.840688889265));
#28036=CARTESIAN_POINT('Ctrl Pts',(22.9727257293063,48.3333837417603,-25.6827403660725));
#28037=CARTESIAN_POINT('Ctrl Pts',(23.0200584320667,51.578512333566,-25.5247918428801));
#28038=CARTESIAN_POINT('Ctrl Pts',(20.3303277842108,53.3910141178971,-25.3668433196876));
#28039=CARTESIAN_POINT('Ctrl Pts',(17.3388414083637,52.1318668903096,-25.2088947964951));
#28040=CARTESIAN_POINT('Ctrl Pts',(16.7646998141231,48.9338680409178,-25.0509462733026));
#28041=CARTESIAN_POINT('Ctrl Pts',(18.3310579529763,47.4565819515315,-24.945647257841));
#28042=CARTESIAN_POINT('Ctrl Pts',(19.2540671456531,47.2098224301578,-24.8929977501102));
#28043=CARTESIAN_POINT('Ctrl Pts',(17.6639373423039,51.9973015569307,-40.3210067496694));
#28044=CARTESIAN_POINT('Ctrl Pts',(17.003216778308,51.2245165804374,-40.2683572419386));
#28045=CARTESIAN_POINT('Ctrl Pts',(16.520038278527,48.9847745965717,-40.163058226477));
#28046=CARTESIAN_POINT('Ctrl Pts',(18.9512732547528,46.5262660550493,-40.0051097032845));
#28047=CARTESIAN_POINT('Ctrl Pts',(22.3337617221332,47.2252515387578,-39.847161180092));
#28048=CARTESIAN_POINT('Ctrl Pts',(23.6000558077849,50.4361301927122,-39.6892126568996));
#28049=CARTESIAN_POINT('Ctrl Pts',(21.6024147148416,53.2535259157778,-39.5312641337071));
#28050=CARTESIAN_POINT('Ctrl Pts',(18.1518494020808,53.1200733432643,-39.3733156105146));
#28051=CARTESIAN_POINT('Ctrl Pts',(16.376977963313,50.1582350183397,-39.2153670873222));
#28052=CARTESIAN_POINT('Ctrl Pts',(17.8869743722217,47.0526837548,-39.0574185641297));
#28053=CARTESIAN_POINT('Ctrl Pts',(21.3127949123184,46.6194980929628,-38.8994700409373));
#28054=CARTESIAN_POINT('Ctrl Pts',(23.5483401839262,49.2512486096866,-38.7415215177447));
#28055=CARTESIAN_POINT('Ctrl Pts',(22.566715362225,52.561900427485,-38.5835729945523));
#28056=CARTESIAN_POINT('Ctrl Pts',(19.257926763209,53.5497393781131,-38.4256244713598));
#28057=CARTESIAN_POINT('Ctrl Pts',(16.6219539119773,51.3191454645357,-38.2676759481674));
#28058=CARTESIAN_POINT('Ctrl Pts',(17.0487524523756,47.8925185252508,-38.1097274249749));
#28059=CARTESIAN_POINT('Ctrl Pts',(20.1513575155428,46.3766829286487,-37.9517789017824));
#28060=CARTESIAN_POINT('Ctrl Pts',(23.1167312576603,48.1459977249851,-37.79383037859));
#28061=CARTESIAN_POINT('Ctrl Pts',(23.2562595922233,51.5962804981864,-37.6358818553975));
#28062=CARTESIAN_POINT('Ctrl Pts',(20.4434363727656,53.5992640406764,-37.477933332205));
#28063=CARTESIAN_POINT('Ctrl Pts',(17.2285628888723,52.338904470578,-37.3199848090125));
#28064=CARTESIAN_POINT('Ctrl Pts',(16.5264671400482,48.9579312880643,-37.1620362858201));
#28065=CARTESIAN_POINT('Ctrl Pts',(18.9737179946959,46.5217701454759,-37.0040877626275));
#28066=CARTESIAN_POINT('Ctrl Pts',(22.3514675295518,47.2392142103812,-36.8461392394352));
#28067=CARTESIAN_POINT('Ctrl Pts',(23.59721297254,50.4597787932788,-36.6881907162426));
#28068=CARTESIAN_POINT('Ctrl Pts',(21.5814748173496,53.2634759238072,-36.5302421930502));
#28069=CARTESIAN_POINT('Ctrl Pts',(18.1318615437831,53.1082786903842,-36.3722936698577));
#28070=CARTESIAN_POINT('Ctrl Pts',(16.3760325915391,50.1348997013926,-36.2143451466653));
#28071=CARTESIAN_POINT('Ctrl Pts',(17.9059446705936,47.0392112564499,-36.0563966234728));
#28072=CARTESIAN_POINT('Ctrl Pts',(21.3344730289901,46.6279799167075,-35.8984481002803));
#28073=CARTESIAN_POINT('Ctrl Pts',(23.5530752781723,49.2740566312607,-35.7404995770878));
#28074=CARTESIAN_POINT('Ctrl Pts',(22.5502122345312,52.5783241196155,-35.5825510538954));
#28075=CARTESIAN_POINT('Ctrl Pts',(19.2351493190419,53.5449035449308,-35.4246025307029));
#28076=CARTESIAN_POINT('Ctrl Pts',(16.6135532540943,51.2974267394088,-35.2666540075105));
#28077=CARTESIAN_POINT('Ctrl Pts',(17.0623454595379,47.8736125687236,-35.108705484318));
#28078=CARTESIAN_POINT('Ctrl Pts',(20.1746196920941,46.3777292108223,-34.9507569611255));
#28079=CARTESIAN_POINT('Ctrl Pts',(23.1285715606466,48.1660486110843,-34.792808437933));
#28080=CARTESIAN_POINT('Ctrl Pts',(23.2459427463636,51.6171559585651,-34.6348599147406));
#28081=CARTESIAN_POINT('Ctrl Pts',(20.4203163648388,53.6020371819906,-34.4769113915481));
#28082=CARTESIAN_POINT('Ctrl Pts',(17.2136019186591,52.3210608435138,-34.3189628683557));
#28083=CARTESIAN_POINT('Ctrl Pts',(16.5332298683643,48.9356492300977,-34.1610143451631));
#28084=CARTESIAN_POINT('Ctrl Pts',(18.9960728593762,46.5152520889867,-34.0030658219707));
#28085=CARTESIAN_POINT('Ctrl Pts',(22.3691460557279,47.2543698949745,-33.8451172987782));
#28086=CARTESIAN_POINT('Ctrl Pts',(23.5941865776713,50.4828670126241,-33.6871687755858));
#28087=CARTESIAN_POINT('Ctrl Pts',(21.5604874418836,53.2735632956638,-33.5292202523933));
#28088=CARTESIAN_POINT('Ctrl Pts',(18.1119418026202,53.0962192994522,-33.3712717292008));
#28089=CARTESIAN_POINT('Ctrl Pts',(16.3752411082267,50.1116274316806,-33.2133232060084));
#28090=CARTESIAN_POINT('Ctrl Pts',(17.9249990589457,47.0258263665991,-33.0553746828159));
#28091=CARTESIAN_POINT('Ctrl Pts',(21.3560972546178,46.63661807952,-32.8974261596234));
#28092=CARTESIAN_POINT('Ctrl Pts',(23.5576633133616,49.2968858871031,-32.739477636431));
#28093=CARTESIAN_POINT('Ctrl Pts',(22.5336042473189,52.5946458766007,-32.5815291132385));
#28094=CARTESIAN_POINT('Ctrl Pts',(19.2124032663222,53.5399193623716,-32.423580590046));
#28095=CARTESIAN_POINT('Ctrl Pts',(16.6052922900793,51.2756556240609,-32.2656320668535));
#28096=CARTESIAN_POINT('Ctrl Pts',(17.0760595490536,47.8547937287262,-32.1076835436611));
#28097=CARTESIAN_POINT('Ctrl Pts',(20.197874687272,46.378925116056,-31.9497350204686));
#28098=CARTESIAN_POINT('Ctrl Pts',(23.1402828646275,48.1861749706435,-31.7917864972762));
#28099=CARTESIAN_POINT('Ctrl Pts',(23.2354920760113,51.637964814354,-31.6338379740837));
#28100=CARTESIAN_POINT('Ctrl Pts',(20.397179025119,53.6046617773376,-31.4758894508912));
#28101=CARTESIAN_POINT('Ctrl Pts',(17.1987558318052,52.3031215376416,-31.3179409276987));
#28102=CARTESIAN_POINT('Ctrl Pts',(16.5401355298036,48.913411046041,-31.1599924045062));
#28103=CARTESIAN_POINT('Ctrl Pts',(19.0184691159077,46.508877711886,-31.0020438813138));
#28104=CARTESIAN_POINT('Ctrl Pts',(22.3867269027061,47.2696387786791,-30.8440953581213));
#28105=CARTESIAN_POINT('Ctrl Pts',(23.591011995838,50.5059353246612,-30.6861468349289));
#28106=CARTESIAN_POINT('Ctrl Pts',(21.5394357280369,53.2835156991,-30.5281983117364));
#28107=CARTESIAN_POINT('Ctrl Pts',(18.0920999054453,53.0840322527814,-30.370249788544));
#28108=CARTESIAN_POINT('Ctrl Pts',(16.3745990724293,50.0883505594653,-30.2123012653514));
#28109=CARTESIAN_POINT('Ctrl Pts',(17.9441389988542,47.012564100946,-30.054352742159));
#28110=CARTESIAN_POINT('Ctrl Pts',(21.3776655688371,46.6453949133369,-29.8964042189665));
#28111=CARTESIAN_POINT('Ctrl Pts',(23.5621046673495,49.3197441321162,-29.7384556957741));
#28112=CARTESIAN_POINT('Ctrl Pts',(22.5168918005126,52.6108606572331,-29.5805071725816));
#28113=CARTESIAN_POINT('Ctrl Pts',(19.1896896859145,53.5347892302254,-29.4225586493891));
#28114=CARTESIAN_POINT('Ctrl Pts',(16.5971712887038,51.2538319138251,-29.2646101261966));
#28115=CARTESIAN_POINT('Ctrl Pts',(17.0898941915086,47.8360633349363,-29.1066616030042));
#28116=CARTESIAN_POINT('Ctrl Pts',(20.2211215243232,46.3802703166986,-28.9487130798117));
#28117=CARTESIAN_POINT('Ctrl Pts',(23.1518646955083,48.2063761140114,-28.7907645566193));
#28118=CARTESIAN_POINT('Ctrl Pts',(23.2249080081672,51.6587061365469,-28.6328160334268));
#28119=CARTESIAN_POINT('Ctrl Pts',(20.3740253084567,53.6071377555246,-28.4748675102343));
#28120=CARTESIAN_POINT('Ctrl Pts',(17.1840252420261,52.2850872713679,-28.3169189870418));
#28121=CARTESIAN_POINT('Ctrl Pts',(16.5471838347117,48.8912176686634,-28.1589704638494));
#28122=CARTESIAN_POINT('Ctrl Pts',(19.0409058515914,46.5026472585805,-28.0010219406569));
#28123=CARTESIAN_POINT('Ctrl Pts',(22.4042093239182,47.2850202619573,-27.8430734174644));
#28124=CARTESIAN_POINT('Ctrl Pts',(23.5876894013757,50.5289827219232,-27.685124894272));
#28125=CARTESIAN_POINT('Ctrl Pts',(21.518320457159,53.29333283432,-27.5271763710795));
#28126=CARTESIAN_POINT('Ctrl Pts',(18.0723368427983,53.0717178336273,-27.369227847887));
#28127=CARTESIAN_POINT('Ctrl Pts',(16.3741061672535,50.0650704804189,-27.2112793246946));
#28128=CARTESIAN_POINT('Ctrl Pts',(17.9633643847556,46.9994241385813,-27.0533308015021));
#28129=CARTESIAN_POINT('Ctrl Pts',(21.3991757215647,46.654311783583,-26.8953822783096));
#28130=CARTESIAN_POINT('Ctrl Pts',(23.5664018661069,49.3426269852974,-26.7374337551172));
#28131=CARTESIAN_POINT('Ctrl Pts',(22.5000701900221,52.6269746383103,-26.5794852319247));
#28132=CARTESIAN_POINT('Ctrl Pts',(19.1670202507297,53.5294997326245,-26.4215367087322));
#28133=CARTESIAN_POINT('Ctrl Pts',(16.5891692111351,51.2319836373097,-26.2635881855398));
#28134=CARTESIAN_POINT('Ctrl Pts',(17.1038913663152,47.8173681526091,-26.1056396623473));
#28135=CARTESIAN_POINT('Ctrl Pts',(20.2442745382167,46.3818722728576,-25.9476911391548));
#28136=CARTESIAN_POINT('Ctrl Pts',(23.1634852082715,48.2264371620868,-25.7897426159623));
#28137=CARTESIAN_POINT('Ctrl Pts',(23.2138552452965,51.6798052942057,-25.6317940927699));
#28138=CARTESIAN_POINT('Ctrl Pts',(20.3515248813337,53.6086151161717,-25.4738455695774));
#28139=CARTESIAN_POINT('Ctrl Pts',(17.1680751579223,52.2686685512262,-25.3158970463849));
#28140=CARTESIAN_POINT('Ctrl Pts',(16.5570909615237,48.8654544718428,-25.1579485231925));
#28141=CARTESIAN_POINT('Ctrl Pts',(18.2239621276955,47.2933710986319,-25.0526495077308));
#28142=CARTESIAN_POINT('Ctrl Pts',(19.2062007174672,47.0307770462543,-25.));
#28143=CARTESIAN_POINT('Ctrl Pts',(22.51811817366,49.9978011072146,-38.387416697508));
#28144=CARTESIAN_POINT('Ctrl Pts',(22.5197005021771,49.8234380607443,-38.3984493876971));
#28145=CARTESIAN_POINT('Ctrl Pts',(22.5031152203389,49.6493741016012,-38.4094820778862));
#28146=CARTESIAN_POINT('Ctrl Pts',(22.4672443342715,49.4793798749943,-38.4205147680753));
#28147=CARTESIAN_POINT('Ctrl Pts',(22.296063555971,48.6681441569118,-38.4731642758061));
#28148=CARTESIAN_POINT('Ctrl Pts',(21.6856861120934,47.9495896397109,-38.525813783537));
#28149=CARTESIAN_POINT('Ctrl Pts',(20.9128165046445,47.6494493532743,-38.5784632912678));
#28150=CARTESIAN_POINT('Ctrl Pts',(20.1399468971955,47.3493090668377,-38.6311127989986));
#28151=CARTESIAN_POINT('Ctrl Pts',(19.2045851261751,47.4675830111656,-38.6837623067294));
#28152=CARTESIAN_POINT('Ctrl Pts',(18.53076487949,47.9506788416322,-38.7364118144602));
#28153=CARTESIAN_POINT('Ctrl Pts',(17.8569446328048,48.4337746720989,-38.7890613221911));
#28154=CARTESIAN_POINT('Ctrl Pts',(17.4446659104548,49.2816923887045,-38.8417108299219));
#28155=CARTESIAN_POINT('Ctrl Pts',(17.4808257113154,50.1099909239769,-38.8943603376527));
#28156=CARTESIAN_POINT('Ctrl Pts',(17.516985512176,50.9382894592493,-38.9470098453835));
#28157=CARTESIAN_POINT('Ctrl Pts',(18.0015838362472,51.7469688131886,-38.9996593531144));
#28158=CARTESIAN_POINT('Ctrl Pts',(18.7149419525084,52.1695269626545,-39.0523088608452));
#28159=CARTESIAN_POINT('Ctrl Pts',(19.4283000687697,52.5920851121204,-39.104958368576));
#28160=CARTESIAN_POINT('Ctrl Pts',(20.370417977221,52.6285220571129,-39.1576078763068));
#28161=CARTESIAN_POINT('Ctrl Pts',(21.1141878175962,52.2621196450141,-39.2102573840377));
#28162=CARTESIAN_POINT('Ctrl Pts',(21.8579576579715,51.8957172329152,-39.2629068917685));
#28163=CARTESIAN_POINT('Ctrl Pts',(22.4033794302707,51.126475463725,-39.3155563994993));
#28164=CARTESIAN_POINT('Ctrl Pts',(22.5032203331966,50.3035167985687,-39.3682059072301));
#28165=CARTESIAN_POINT('Ctrl Pts',(22.5153636733716,50.2034228818663,-39.3746095039894));
#28166=CARTESIAN_POINT('Ctrl Pts',(22.5209154892233,50.1025343255133,-39.3810131007487));
#28167=CARTESIAN_POINT('Ctrl Pts',(22.5201576955115,50.0015647648602,-39.387416697508));
#28168=CARTESIAN_POINT('Ctrl Pts',(20.7937992825328,47.0307770462543,-40.));
#28169=CARTESIAN_POINT('Ctrl Pts',(21.7760378723045,47.2933710986319,-39.9473504922692));
#28170=CARTESIAN_POINT('Ctrl Pts',(23.4429089208816,48.865455216316,-39.8420514768075));
#28171=CARTESIAN_POINT('Ctrl Pts',(22.8319249444368,52.2686682330012,-39.6841029536151));
#28172=CARTESIAN_POINT('Ctrl Pts',(19.6484751064271,53.6086153775441,-39.5261544304226));
#28173=CARTESIAN_POINT('Ctrl Pts',(16.7861446928906,51.6798052066136,-39.3682059072302));
#28174=CARTESIAN_POINT('Ctrl Pts',(16.8365147494583,48.2264371981741,-39.2102573840376));
#28175=CARTESIAN_POINT('Ctrl Pts',(19.7557254495835,46.3818721760905,-39.0523088608452));
#28176=CARTESIAN_POINT('Ctrl Pts',(22.8961086873501,47.8173681367529,-38.8943603376527));
#28177=CARTESIAN_POINT('Ctrl Pts',(23.4108308418939,51.2319836465612,-38.7364118144603));
#28178=CARTESIAN_POINT('Ctrl Pts',(20.8329797652707,53.529499797304,-38.5784632912678));
#28179=CARTESIAN_POINT('Ctrl Pts',(17.4999297672036,52.6269746785947,-38.4205147680753));
#28180=CARTESIAN_POINT('Ctrl Pts',(16.4335980754498,49.3426269761734,-38.2625662448828));
#28181=CARTESIAN_POINT('Ctrl Pts',(18.6008242547947,46.6543117271026,-38.1046177216904));
#28182=CARTESIAN_POINT('Ctrl Pts',(22.0366356492785,46.9994240892982,-37.9466691984979));
#28183=CARTESIAN_POINT('Ctrl Pts',(23.6258938927882,50.065070481226,-37.7887206753055));
#28184=CARTESIAN_POINT('Ctrl Pts',(21.9276631892634,53.0717178847477,-37.6307721521129));
#28185=CARTESIAN_POINT('Ctrl Pts',(18.4816795176051,53.2933328888968,-37.4728236289205));
#28186=CARTESIAN_POINT('Ctrl Pts',(16.4123105391071,50.5289827307422,-37.314875105728));
#28187=CARTESIAN_POINT('Ctrl Pts',(17.595790636172,47.2850202168804,-37.1569265825356));
#28188=CARTESIAN_POINT('Ctrl Pts',(20.959094164331,46.5026472005525,-36.9989780593431));
#28189=CARTESIAN_POINT('Ctrl Pts',(23.4528162225852,48.891217650257,-36.8410295361507));
#28190=CARTESIAN_POINT('Ctrl Pts',(22.8159748047073,52.2850873092924,-36.6830810129581));
#28191=CARTESIAN_POINT('Ctrl Pts',(19.6259746853353,53.6071378153842,-36.5251324897657));
#28192=CARTESIAN_POINT('Ctrl Pts',(16.7750919383154,51.6587061640742,-36.3671839665732));
#28193=CARTESIAN_POINT('Ctrl Pts',(16.8481352521856,48.2063760842456,-36.2092354433807));
#28194=CARTESIAN_POINT('Ctrl Pts',(19.7788784720074,46.3802702566287,-36.0512869201883));
#28195=CARTESIAN_POINT('Ctrl Pts',(22.910105856785,47.8360632990252,-35.8933383969958));
#28196=CARTESIAN_POINT('Ctrl Pts',(23.4028287677669,51.2538319346328,-35.7353898738033));
#28197=CARTESIAN_POINT('Ctrl Pts',(20.8103103275328,53.5347892888857,-35.5774413506109));
#28198=CARTESIAN_POINT('Ctrl Pts',(17.4831081577191,52.610860700561,-35.4194928274184));
#28199=CARTESIAN_POINT('Ctrl Pts',(16.4378952735367,49.3197441208273,-35.2615443042259));
#28200=CARTESIAN_POINT('Ctrl Pts',(18.6223344083003,46.6453948576666,-35.1035957810335));
#28201=CARTESIAN_POINT('Ctrl Pts',(22.0558610352632,47.012564051369,-34.945647257841));
#28202=CARTESIAN_POINT('Ctrl Pts',(23.6254009877349,50.0883505609314,-34.7876987346485));
#28203=CARTESIAN_POINT('Ctrl Pts',(21.9079001262167,53.0840323039615,-34.6297502114561));
#28204=CARTESIAN_POINT('Ctrl Pts',(18.4605642464159,53.2835157535905,-34.4718016882636));
#28205=CARTESIAN_POINT('Ctrl Pts',(16.4089879445684,50.5059353330574,-34.3138531650712));
#28206=CARTESIAN_POINT('Ctrl Pts',(17.6132730576857,47.2696387333682,-34.1559046418787));
#28207=CARTESIAN_POINT('Ctrl Pts',(20.9815309003809,46.5088776539501,-33.9979561186862));
#28208=CARTESIAN_POINT('Ctrl Pts',(23.4598645276135,48.9134110280088,-33.8400075954937));
#28209=CARTESIAN_POINT('Ctrl Pts',(22.801244214682,52.3031215758622,-33.6820590723013));
#28210=CARTESIAN_POINT('Ctrl Pts',(19.6028209682899,53.6046618371577,-33.5241105491088));
#28211=CARTESIAN_POINT('Ctrl Pts',(16.7645078702952,51.6379648415364,-33.3661620259164));
#28212=CARTESIAN_POINT('Ctrl Pts',(16.8597170832589,48.1861749405428,-33.2082135027238));
#28213=CARTESIAN_POINT('Ctrl Pts',(19.8021253094441,46.3789250559636,-33.0502649795314));
#28214=CARTESIAN_POINT('Ctrl Pts',(22.9239404994698,47.854793693126,-32.8923164563389));
#28215=CARTESIAN_POINT('Ctrl Pts',(23.3947077662565,51.2756556452305,-32.7343679331465));
#28216=CARTESIAN_POINT('Ctrl Pts',(20.7875967467482,53.5399194211172,-32.5764194099539));
#28217=CARTESIAN_POINT('Ctrl Pts',(17.4663957106355,52.5946459196594,-32.4184708867616));
#28218=CARTESIAN_POINT('Ctrl Pts',(16.4423366275984,49.2968858754349,-32.260522363569));
#28219=CARTESIAN_POINT('Ctrl Pts',(18.6439027228774,46.6366180237041,-32.1025738403766));
#28220=CARTESIAN_POINT('Ctrl Pts',(22.0750009754893,47.0258263172421,-31.9446253171841));
#28221=CARTESIAN_POINT('Ctrl Pts',(23.6247589519268,50.111627433533,-31.7866767939916));
#28222=CARTESIAN_POINT('Ctrl Pts',(21.8880582287126,53.0962193508344,-31.6287282707992));
#28223=CARTESIAN_POINT('Ctrl Pts',(18.4395125322199,53.2735633499893,-31.4707797476067));
#28224=CARTESIAN_POINT('Ctrl Pts',(16.4058133626825,50.4828670206375,-31.3128312244142));
#28225=CARTESIAN_POINT('Ctrl Pts',(17.6308539049556,47.2543698494103,-31.1548827012218));
#28226=CARTESIAN_POINT('Ctrl Pts',(21.0039271572841,46.5152520311566,-30.9969341780293));
#28227=CARTESIAN_POINT('Ctrl Pts',(23.4667701891674,48.9356492124344,-30.8389856548368));
#28228=CARTESIAN_POINT('Ctrl Pts',(22.7863981275818,52.3210608820322,-30.6810371316443));
#28229=CARTESIAN_POINT('Ctrl Pts',(19.5796836281861,53.602037241767,-30.5230886084519));
#28230=CARTESIAN_POINT('Ctrl Pts',(16.7540571997694,51.6171559854022,-30.3651400852594));
#28231=CARTESIAN_POINT('Ctrl Pts',(16.8714283874341,48.1660485806496,-30.207191562067));
#28232=CARTESIAN_POINT('Ctrl Pts',(19.825380305008,46.3777291507101,-30.0492430388745));
#28233=CARTESIAN_POINT('Ctrl Pts',(22.937654589213,47.8736125334356,-29.891294515682));
#28234=CARTESIAN_POINT('Ctrl Pts',(23.3864468021045,51.2974267609398,-29.7333459924896));
#28235=CARTESIAN_POINT('Ctrl Pts',(20.7648506936511,53.5449036037592,-29.5753974692971));
#28236=CARTESIAN_POINT('Ctrl Pts',(17.4497877231476,52.5783241624032,-29.4174489461046));
#28237=CARTESIAN_POINT('Ctrl Pts',(16.4469246628638,49.2740566192138,-29.2595004229122));
#28238=CARTESIAN_POINT('Ctrl Pts',(18.665526948864,46.6279798607482,-29.1015518997197));
#28239=CARTESIAN_POINT('Ctrl Pts',(22.0940553641576,47.0392112073149,-28.9436033765272));
#28240=CARTESIAN_POINT('Ctrl Pts',(23.6239674686013,50.1348997036314,-28.7856548533348));
#28241=CARTESIAN_POINT('Ctrl Pts',(21.868138487219,53.1082787419663,-28.6277063301423));
#28242=CARTESIAN_POINT('Ctrl Pts',(18.4185251564057,53.2634759779658,-28.4697578069498));
#28243=CARTESIAN_POINT('Ctrl Pts',(16.4027869677635,50.4597788009081,-28.3118092837573));
#28244=CARTESIAN_POINT('Ctrl Pts',(17.6485324314252,47.2392141645673,-28.1538607605649));
#28245=CARTESIAN_POINT('Ctrl Pts',(21.026282022335,46.5217700877505,-27.9959122373724));
#28246=CARTESIAN_POINT('Ctrl Pts',(23.4735329175963,48.9579312707775,-27.83796371418));
#28247=CARTESIAN_POINT('Ctrl Pts',(22.771437157119,52.3389045093798,-27.6800151909875));
#28248=CARTESIAN_POINT('Ctrl Pts',(19.5565636198783,53.5992641004309,-27.522066667795));
#28249=CARTESIAN_POINT('Ctrl Pts',(16.743740353733,51.5962805246318,-27.3641181446025));
#28250=CARTESIAN_POINT('Ctrl Pts',(16.8832686906281,48.1459976943029,-27.2061696214101));
#28251=CARTESIAN_POINT('Ctrl Pts',(19.8486424819224,46.3766828683592,-27.0482210982176));
#28252=CARTESIAN_POINT('Ctrl Pts',(22.9512475966477,47.8925184905753,-26.8902725750252));
#28253=CARTESIAN_POINT('Ctrl Pts',(23.3780461439863,51.3191454858715,-26.7323240518326));
#28254=CARTESIAN_POINT('Ctrl Pts',(20.7420732493018,53.5497394380497,-26.5743755286402));
#28255=CARTESIAN_POINT('Ctrl Pts',(17.4332845947801,52.5619004681089,-26.4164270054477));
#28256=CARTESIAN_POINT('Ctrl Pts',(16.4516597580046,49.2512486007173,-26.2584784822552));
#28257=CARTESIAN_POINT('Ctrl Pts',(18.6872050642303,46.6194980305971,-26.1005299590628));
#28258=CARTESIAN_POINT('Ctrl Pts',(22.113025666239,47.0526837171379,-25.9425814358703));
#28259=CARTESIAN_POINT('Ctrl Pts',(23.6230220898943,50.1582350010085,-25.7846329126779));
#28260=CARTESIAN_POINT('Ctrl Pts',(21.8481506426783,53.1200734299207,-25.6266843894854));
#28261=CARTESIAN_POINT('Ctrl Pts',(18.3975852298821,53.2535259099818,-25.4687358662929));
#28262=CARTESIAN_POINT('Ctrl Pts',(16.3999441908908,50.4361302999107,-25.3107873431005));
#28263=CARTESIAN_POINT('Ctrl Pts',(17.6662381197281,47.2252513302932,-25.1528388199079));
#28264=CARTESIAN_POINT('Ctrl Pts',(21.0487270098574,46.5262662593188,-24.9948902967155));
#28265=CARTESIAN_POINT('Ctrl Pts',(23.4799612028624,48.9847740496603,-24.836941773523));
#28266=CARTESIAN_POINT('Ctrl Pts',(22.996783221692,51.2245165804373,-24.7316427580614));
#28267=CARTESIAN_POINT('Ctrl Pts',(22.3360626576962,51.9973015569306,-24.6789932503306));
#28268=CARTESIAN_POINT('Ctrl Pts',(20.7459328543469,47.2098224301578,-40.1070022498898));
#28269=CARTESIAN_POINT('Ctrl Pts',(21.6689420470237,47.4565819515315,-40.054352742159));
#28270=CARTESIAN_POINT('Ctrl Pts',(23.2353000753732,48.9338687404989,-39.9490537266973));
#28271=CARTESIAN_POINT('Ctrl Pts',(22.6611586878231,52.1318665912736,-39.7911052035049));
#28272=CARTESIAN_POINT('Ctrl Pts',(19.669672204288,53.3910143635086,-39.6331566803124));
#28273=CARTESIAN_POINT('Ctrl Pts',(16.9799415098477,51.5785122512557,-39.4752081571199));
#28274=CARTESIAN_POINT('Ctrl Pts',(17.0272742309725,48.3333837756716,-39.3172596339275));
#28275=CARTESIAN_POINT('Ctrl Pts',(19.7704553069699,46.6000467946138,-39.159311110735));
#28276=CARTESIAN_POINT('Ctrl Pts',(22.7214721242389,47.9489817494599,-39.0013625875425));
#28277=CARTESIAN_POINT('Ctrl Pts',(23.2051563179425,51.1576945182614,-38.8434140643501));
#28278=CARTESIAN_POINT('Ctrl Pts',(20.782750737616,53.3166694857916,-38.6854655411576));
#28279=CARTESIAN_POINT('Ctrl Pts',(17.6506850461402,52.4685670085878,-38.5275170179651));
#28280=CARTESIAN_POINT('Ctrl Pts',(16.6486536006437,49.3822668439948,-38.3695684947727));
#28281=CARTESIAN_POINT('Ctrl Pts',(18.6851951364534,46.8560581269433,-38.2116199715802));
#28282=CARTESIAN_POINT('Ctrl Pts',(21.9138256692342,47.1803600695975,-38.0536714483877));
#28283=CARTESIAN_POINT('Ctrl Pts',(23.4072509770689,50.0611467040381,-37.8957229251952));
#28284=CARTESIAN_POINT('Ctrl Pts',(21.8114242940591,52.8864920137083,-37.7377744020028));
#28285=CARTESIAN_POINT('Ctrl Pts',(18.573234876665,53.0947435405722,-37.5798258788103));
#28286=CARTESIAN_POINT('Ctrl Pts',(16.628649711631,50.4970848512028,-37.4218773556178));
#28287=CARTESIAN_POINT('Ctrl Pts',(17.7407654646833,47.4487346314366,-37.2639288324254));
#28288=CARTESIAN_POINT('Ctrl Pts',(20.9012603857541,46.7135390346713,-37.1059803092329));
#28289=CARTESIAN_POINT('Ctrl Pts',(23.2446099626473,48.9580776889162,-36.9480317860404));
#28290=CARTESIAN_POINT('Ctrl Pts',(22.6461703481792,52.1472955904087,-36.790083262848));
#28291=CARTESIAN_POINT('Ctrl Pts',(19.6485285679831,53.3896258989639,-36.6321347396555));
#28292=CARTESIAN_POINT('Ctrl Pts',(16.9695552409884,51.5586854897913,-36.474186216463));
#28293=CARTESIAN_POINT('Ctrl Pts',(17.0381940125332,48.3145323552894,-36.3162376932706));
#28294=CARTESIAN_POINT('Ctrl Pts',(19.7922121924742,46.5985414715644,-36.1582891700781));
#28295=CARTESIAN_POINT('Ctrl Pts',(22.7346252585124,47.9665495856411,-36.0003406468857));
#28296=CARTESIAN_POINT('Ctrl Pts',(23.1976367722267,51.1782253454396,-35.8423921236931));
#28297=CARTESIAN_POINT('Ctrl Pts',(20.7614482764392,53.3216400188223,-35.6844436005007));
#28298=CARTESIAN_POINT('Ctrl Pts',(17.6348777867315,52.4534247101578,-35.5264950773082));
#28299=CARTESIAN_POINT('Ctrl Pts',(16.6526916758916,49.3607638343807,-35.3685465541157));
#28300=CARTESIAN_POINT('Ctrl Pts',(18.7054082187211,46.8476789484576,-35.2105980309233));
#28301=CARTESIAN_POINT('Ctrl Pts',(21.9318917564165,47.1927076864689,-35.0526495077308));
#28302=CARTESIAN_POINT('Ctrl Pts',(23.406787794396,50.0830229852167,-34.8947009845383));
#28303=CARTESIAN_POINT('Ctrl Pts',(21.7928529519662,52.8980638683015,-34.7367524613459));
#28304=CARTESIAN_POINT('Ctrl Pts',(18.5533928651451,53.0855183826241,-34.5788039381534));
#28305=CARTESIAN_POINT('Ctrl Pts',(16.6255274709304,50.4754272212218,-34.4208554149609));
#28306=CARTESIAN_POINT('Ctrl Pts',(17.75719368888,47.4342806578026,-34.2629068917685));
#28307=CARTESIAN_POINT('Ctrl Pts',(20.9223441772518,46.7193937891277,-34.104958368576));
#28308=CARTESIAN_POINT('Ctrl Pts',(23.2512332519394,48.9789327967227,-33.9470098453835));
#28309=CARTESIAN_POINT('Ctrl Pts',(22.6323280188832,52.1642423831742,-33.7890613221911));
#28310=CARTESIAN_POINT('Ctrl Pts',(19.6267710297432,53.3872992232582,-33.6311127989986));
#28311=CARTESIAN_POINT('Ctrl Pts',(16.9596093966892,51.539194877663,-33.4731642758061));
#28312=CARTESIAN_POINT('Ctrl Pts',(17.0490774543567,48.2955493489868,-33.3152157526137));
#28313=CARTESIAN_POINT('Ctrl Pts',(19.8140572359068,46.597277387061,-33.1572672294212));
#28314=CARTESIAN_POINT('Ctrl Pts',(22.7476256664666,47.9841505291569,-32.9993187062288));
#28315=CARTESIAN_POINT('Ctrl Pts',(23.1900054704983,51.1987330771759,-32.8413701830363));
#28316=CARTESIAN_POINT('Ctrl Pts',(20.74010433406,53.3264608019381,-32.6834216598438));
#28317=CARTESIAN_POINT('Ctrl Pts',(17.6191731071852,52.4381876873151,-32.5254731366513));
#28318=CARTESIAN_POINT('Ctrl Pts',(16.6568652144489,49.3392839507299,-32.3675246134589));
#28319=CARTESIAN_POINT('Ctrl Pts',(18.7256759549234,46.8394313612477,-32.2095760902664));
#28320=CARTESIAN_POINT('Ctrl Pts',(21.949877550255,47.2051702321722,-32.0516275670739));
#28321=CARTESIAN_POINT('Ctrl Pts',(23.4061844736153,50.1048962526811,-31.8936790438814));
#28322=CARTESIAN_POINT('Ctrl Pts',(21.7742075291666,52.9095160311594,-31.735730520689));
#28323=CARTESIAN_POINT('Ctrl Pts',(18.5336105781053,53.0761661131155,-31.5777819974965));
#28324=CARTESIAN_POINT('Ctrl Pts',(16.6225443176576,50.4537499376729,-31.419833474304));
#28325=CARTESIAN_POINT('Ctrl Pts',(17.7737144037186,47.4199324939229,-31.2618849511116));
#28326=CARTESIAN_POINT('Ctrl Pts',(20.9433899305122,46.7253837887268,-31.1039364279191));
#28327=CARTESIAN_POINT('Ctrl Pts',(23.2577224992181,48.9998300093421,-30.9459879047267));
#28328=CARTESIAN_POINT('Ctrl Pts',(22.6183771570341,52.1810999416916,-30.7880393815342));
#28329=CARTESIAN_POINT('Ctrl Pts',(19.6050288809086,53.3848328920656,-30.6300908583417));
#28330=CARTESIAN_POINT('Ctrl Pts',(16.9497889059598,51.5196408042424,-30.4721423351492));
#28331=CARTESIAN_POINT('Ctrl Pts',(17.0600825620002,48.276636616999,-30.3141938119568));
#28332=CARTESIAN_POINT('Ctrl Pts',(19.8359099455281,46.5961535953936,-30.1562452887643));
#28333=CARTESIAN_POINT('Ctrl Pts',(22.7605127908721,48.001834585538,-29.9982967655718));
#28334=CARTESIAN_POINT('Ctrl Pts',(23.182242645934,51.2191913855173,-29.8403482423794));
#28335=CARTESIAN_POINT('Ctrl Pts',(20.7187298774621,53.3311444362856,-29.6823997191869));
#28336=CARTESIAN_POINT('Ctrl Pts',(17.6035665882775,52.4228501388366,-29.5244511959944));
#28337=CARTESIAN_POINT('Ctrl Pts',(16.6611765892721,49.3178313081912,-29.366502672802));
#28338=CARTESIAN_POINT('Ctrl Pts',(18.7459962310538,46.8313140831249,-29.2085541496095));
#28339=CARTESIAN_POINT('Ctrl Pts',(21.9677829513306,47.2177480077848,-29.050605626417));
#28340=CARTESIAN_POINT('Ctrl Pts',(23.4054407170648,50.1267651951753,-28.8926571032246));
#28341=CARTESIAN_POINT('Ctrl Pts',(21.7554889564025,52.9208482359706,-28.7347085800321));
#28342=CARTESIAN_POINT('Ctrl Pts',(18.5138887498158,53.0666870138371,-28.5767600568396));
#28343=CARTESIAN_POINT('Ctrl Pts',(16.619700415616,50.4320539472337,-28.4188115336471));
#28344=CARTESIAN_POINT('Ctrl Pts',(17.7903269076605,47.4056907032041,-28.2608630104547));
#28345=CARTESIAN_POINT('Ctrl Pts',(20.9643967878664,46.7315088037866,-28.1029144872622));
#28346=CARTESIAN_POINT('Ctrl Pts',(23.264077432299,49.0207684502632,-27.9449659640697));
#28347=CARTESIAN_POINT('Ctrl Pts',(22.6043183393371,52.1978675908597,-27.7870174408773));
#28348=CARTESIAN_POINT('Ctrl Pts',(19.5833030187556,53.3822269723099,-27.6290689176848));
#28349=CARTESIAN_POINT('Ctrl Pts',(16.9400941700472,51.5000241424731,-27.4711203944923));
#28350=CARTESIAN_POINT('Ctrl Pts',(17.0712088899677,48.2577948074711,-27.3131718712999));
#28351=CARTESIAN_POINT('Ctrl Pts',(19.8577694034615,46.5951704043054,-27.1552233481074));
#28352=CARTESIAN_POINT('Ctrl Pts',(22.7732861342827,48.019600505568,-26.997274824915));
#28353=CARTESIAN_POINT('Ctrl Pts',(23.174348551008,51.2396004622671,-26.8393263017225));
#28354=CARTESIAN_POINT('Ctrl Pts',(20.6973259225178,53.3356886677492,-26.68137777853));
#28355=CARTESIAN_POINT('Ctrl Pts',(17.5880586054414,52.407416800166,-26.5234292553375));
#28356=CARTESIAN_POINT('Ctrl Pts',(16.6656261561987,49.2963986227336,-26.365480732145));
#28357=CARTESIAN_POINT('Ctrl Pts',(18.766367147012,46.8233437108734,-26.2075322089526));
#28358=CARTESIAN_POINT('Ctrl Pts',(21.9856093362754,47.2304081196401,-26.0495836857601));
#28359=CARTESIAN_POINT('Ctrl Pts',(23.4045523450886,50.148693364377,-25.8916351625677));
#28360=CARTESIAN_POINT('Ctrl Pts',(21.7367063872335,52.9319316993164,-25.7336866393752));
#28361=CARTESIAN_POINT('Ctrl Pts',(18.4942115096051,53.0573369391072,-25.5757381161827));
#28362=CARTESIAN_POINT('Ctrl Pts',(16.6170290593757,50.4098314607207,-25.4177895929903));
#28363=CARTESIAN_POINT('Ctrl Pts',(17.8069649355658,47.392569833667,-25.2598410697978));
#28364=CARTESIAN_POINT('Ctrl Pts',(20.9854883332692,46.7357338543319,-25.1018925466053));
#28365=CARTESIAN_POINT('Ctrl Pts',(23.2701180892795,49.0459925983713,-24.9439440234128));
#28366=CARTESIAN_POINT('Ctrl Pts',(22.8160759421236,51.1506777193426,-24.8386450079512));
#28367=CARTESIAN_POINT('Ctrl Pts',(22.1951971040192,51.8768634390787,-24.7859955002204));
#28368=CARTESIAN_POINT('Ctrl Pts',(20.698066426161,47.3888678140614,-40.2140044997796));
#28369=CARTESIAN_POINT('Ctrl Pts',(21.561846221743,47.6197928044311,-40.1613549920488));
#28370=CARTESIAN_POINT('Ctrl Pts',(23.0276912298648,49.0022822646818,-40.0560559765871));
#28371=CARTESIAN_POINT('Ctrl Pts',(22.4903924312093,51.9950649495461,-39.8981074533947));
#28372=CARTESIAN_POINT('Ctrl Pts',(19.6908693021489,53.1734133494731,-39.7401589302022));
#28373=CARTESIAN_POINT('Ctrl Pts',(17.1737383268048,51.4772192958978,-39.5822104070098));
#28374=CARTESIAN_POINT('Ctrl Pts',(17.2180337124866,48.4403303531691,-39.4242618838172));
#28375=CARTESIAN_POINT('Ctrl Pts',(19.7851851643563,46.818221413137,-39.2663133606248));
#28376=CARTESIAN_POINT('Ctrl Pts',(22.5468355611278,48.0805953621669,-39.1083648374323));
#28377=CARTESIAN_POINT('Ctrl Pts',(22.9994817939913,51.0834053899617,-38.9504163142399));
#28378=CARTESIAN_POINT('Ctrl Pts',(20.7325217099613,53.103839174279,-38.7924677910474));
#28379=CARTESIAN_POINT('Ctrl Pts',(17.8014403250768,52.3101593385808,-38.6345192678549));
#28380=CARTESIAN_POINT('Ctrl Pts',(16.8637091258375,49.4219067118163,-38.4765707446625));
#28381=CARTESIAN_POINT('Ctrl Pts',(18.7695660181121,47.0578045267839,-38.31862222147));
#28382=CARTESIAN_POINT('Ctrl Pts',(21.7910156891898,47.3612960498969,-38.1606736982775));
#28383=CARTESIAN_POINT('Ctrl Pts',(23.1886080613495,50.0572229268501,-38.0027251750851));
#28384=CARTESIAN_POINT('Ctrl Pts',(21.6951853988549,52.7012661426686,-37.8447766518926));
#28385=CARTESIAN_POINT('Ctrl Pts',(18.6647902357249,52.8961541922478,-37.6868281287002));
#28386=CARTESIAN_POINT('Ctrl Pts',(16.8449888841548,50.4651869716634,-37.5288796055076));
#28387=CARTESIAN_POINT('Ctrl Pts',(17.8857402931946,47.6124490459927,-37.3709310823153));
#28388=CARTESIAN_POINT('Ctrl Pts',(20.8434266071773,46.9244308687901,-37.2129825591227));
#28389=CARTESIAN_POINT('Ctrl Pts',(23.0364037027094,49.0249377275755,-37.0550340359303));
#28390=CARTESIAN_POINT('Ctrl Pts',(22.4763658916511,52.0095038715251,-36.8970855127378));
#28391=CARTESIAN_POINT('Ctrl Pts',(19.6710824506308,53.1721139825436,-36.7391369895453));
#28392=CARTESIAN_POINT('Ctrl Pts',(17.1640185436614,51.4586648155085,-36.5811884663528));
#28393=CARTESIAN_POINT('Ctrl Pts',(17.2282527728808,48.4226886263332,-36.4232399431604));
#28394=CARTESIAN_POINT('Ctrl Pts',(19.805545912941,46.8168126865001,-36.2652914199679));
#28395=CARTESIAN_POINT('Ctrl Pts',(22.5591446602398,48.097035872257,-36.1073428967755));
#28396=CARTESIAN_POINT('Ctrl Pts',(22.9924447766865,51.1026187562464,-35.9493943735829));
#28397=CARTESIAN_POINT('Ctrl Pts',(20.7125862253456,53.1084907487588,-35.7914458503905));
#28398=CARTESIAN_POINT('Ctrl Pts',(17.7866474157438,52.2959887197547,-35.633497327198));
#28399=CARTESIAN_POINT('Ctrl Pts',(16.8674880782465,49.4017835479343,-35.4755488040056));
#28400=CARTESIAN_POINT('Ctrl Pts',(18.7884820291419,47.0499630392484,-35.3176002808131));
#28401=CARTESIAN_POINT('Ctrl Pts',(21.8079224775697,47.3728513215688,-35.1596517576206));
#28402=CARTESIAN_POINT('Ctrl Pts',(23.1881746010572,50.077695409502,-35.0017032344282));
#28403=CARTESIAN_POINT('Ctrl Pts',(21.6778057777158,52.7120954326415,-34.8437547112357));
#28404=CARTESIAN_POINT('Ctrl Pts',(18.6462214838744,52.8875210116576,-34.6858061880433));
#28405=CARTESIAN_POINT('Ctrl Pts',(16.8420669972922,50.4449191093862,-34.5278576648507));
#28406=CARTESIAN_POINT('Ctrl Pts',(17.9011143200743,47.5989225822371,-34.3699091416583));
#28407=CARTESIAN_POINT('Ctrl Pts',(20.8631574541227,46.9299099243051,-34.2119606184658));
#28408=CARTESIAN_POINT('Ctrl Pts',(23.0426019762653,49.0444545654367,-34.0540120952734));
#28409=CARTESIAN_POINT('Ctrl Pts',(22.4634118230843,52.0253631904863,-33.8960635720809));
#28410=CARTESIAN_POINT('Ctrl Pts',(19.6507210911966,53.1699366093588,-33.7381150488884));
#28411=CARTESIAN_POINT('Ctrl Pts',(17.1547109230832,51.4404249137897,-33.5801665256959));
#28412=CARTESIAN_POINT('Ctrl Pts',(17.2384378254546,48.4049237574308,-33.4222180025035));
#28413=CARTESIAN_POINT('Ctrl Pts',(19.8259891623695,46.8156297181585,-33.264269479311));
#28414=CARTESIAN_POINT('Ctrl Pts',(22.5713108334635,48.1135073651876,-33.1063209561185));
#28415=CARTESIAN_POINT('Ctrl Pts',(22.9853031747401,51.1218105091212,-32.9483724329261));
#28416=CARTESIAN_POINT('Ctrl Pts',(20.6926119213717,53.113002182759,-32.7904239097336));
#28417=CARTESIAN_POINT('Ctrl Pts',(17.7719505037349,52.2817294549708,-32.6324753865412));
#28418=CARTESIAN_POINT('Ctrl Pts',(16.8713938012994,49.381682026025,-32.4745268633487));
#28419=CARTESIAN_POINT('Ctrl Pts',(18.8074491869694,47.0422446987913,-32.3165783401562));
#28420=CARTESIAN_POINT('Ctrl Pts',(21.8247541250208,47.3845141471024,-32.1586298169637));
#28421=CARTESIAN_POINT('Ctrl Pts',(23.1876099953038,50.0981650718293,-32.0006812937713));
#28422=CARTESIAN_POINT('Ctrl Pts',(21.6603568296206,52.7228127114843,-31.8427327705788));
#28423=CARTESIAN_POINT('Ctrl Pts',(18.6277086239906,52.8787688762418,-31.6847842473863));
#28424=CARTESIAN_POINT('Ctrl Pts',(16.8392752726328,50.4246328547084,-31.5268357241939));
#28425=CARTESIAN_POINT('Ctrl Pts',(17.9165749024817,47.5854951384354,-31.3688872010014));
#28426=CARTESIAN_POINT('Ctrl Pts',(20.8828527037404,46.9355155462971,-31.2109386778089));
#28427=CARTESIAN_POINT('Ctrl Pts',(23.0486748092689,49.0640108062497,-31.0529901546164));
#28428=CARTESIAN_POINT('Ctrl Pts',(22.4503561864863,52.0411390013511,-30.895041631424));
#28429=CARTESIAN_POINT('Ctrl Pts',(19.6303741336312,53.1676285423641,-30.7370931082315));
#28430=CARTESIAN_POINT('Ctrl Pts',(17.1455206121502,51.4221256230826,-30.5791445850391));
#28431=CARTESIAN_POINT('Ctrl Pts',(17.2487367365663,48.3872246533482,-30.4211960618466));
#28432=CARTESIAN_POINT('Ctrl Pts',(19.8464395860482,46.8145780400772,-30.2632475386541));
#28433=CARTESIAN_POINT('Ctrl Pts',(22.5833709925312,48.1300566376404,-30.1052990154616));
#28434=CARTESIAN_POINT('Ctrl Pts',(22.9780384897635,51.1409560100949,-29.9473504922692));
#28435=CARTESIAN_POINT('Ctrl Pts',(20.6726090612732,53.117385268812,-29.7894019690767));
#28436=CARTESIAN_POINT('Ctrl Pts',(17.7573454534073,52.2673761152701,-29.6314534458842));
#28437=CARTESIAN_POINT('Ctrl Pts',(16.8754285156804,49.3616059971687,-29.4735049226918));
#28438=CARTESIAN_POINT('Ctrl Pts',(18.8264655132437,47.0346483055016,-29.3155563994993));
#28439=CARTESIAN_POINT('Ctrl Pts',(21.8415105385036,47.3962848082547,-29.1576078763068));
#28440=CARTESIAN_POINT('Ctrl Pts',(23.1869139655283,50.1186306867194,-28.9996593531144));
#28441=CARTESIAN_POINT('Ctrl Pts',(21.642839425586,52.7334177299748,-28.8417108299219));
#28442=CARTESIAN_POINT('Ctrl Pts',(18.609252343226,52.8698980497084,-28.6837623067294));
#28443=CARTESIAN_POINT('Ctrl Pts',(16.8366138634684,50.4043290935593,-28.5258137835369));
#28444=CARTESIAN_POINT('Ctrl Pts',(17.9321213838958,47.5721672418409,-28.3678652603445));
#28445=CARTESIAN_POINT('Ctrl Pts',(20.9025115533977,46.9412475198227,-28.209916737152));
#28446=CARTESIAN_POINT('Ctrl Pts',(23.0546219470018,49.0836056297488,-28.0519682139596));
#28447=CARTESIAN_POINT('Ctrl Pts',(22.4371995215552,52.0568306723395,-27.8940196907671));
#28448=CARTESIAN_POINT('Ctrl Pts',(19.6100424176328,53.1651898441889,-27.7360711675746));
#28449=CARTESIAN_POINT('Ctrl Pts',(17.1364479863613,51.4037677603142,-27.5781226443821));
#28450=CARTESIAN_POINT('Ctrl Pts',(17.2591490893073,48.3695919206393,-27.4201741211897));
#28451=CARTESIAN_POINT('Ctrl Pts',(19.8668963250006,46.8136579402516,-27.2622255979972));
#28452=CARTESIAN_POINT('Ctrl Pts',(22.5953246719178,48.1466825205607,-27.1042770748048));
#28453=CARTESIAN_POINT('Ctrl Pts',(22.9706509580297,51.1600554386627,-26.9463285516123));
#28454=CARTESIAN_POINT('Ctrl Pts',(20.6525785957338,53.1216378974487,-26.7883800284198));
#28455=CARTESIAN_POINT('Ctrl Pts',(17.7428326161027,52.252933132223,-26.6304315052274));
#28456=CARTESIAN_POINT('Ctrl Pts',(16.8795925543929,49.3415486447498,-26.4724829820348));
#28457=CARTESIAN_POINT('Ctrl Pts',(18.8455292297936,47.0271893911498,-26.3145344588424));
#28458=CARTESIAN_POINT('Ctrl Pts',(21.8581930063119,47.4081325221422,-26.1565859356499));
#28459=CARTESIAN_POINT('Ctrl Pts',(23.1860826002829,50.1391517277455,-25.9986374124575));
#28460=CARTESIAN_POINT('Ctrl Pts',(21.6252621317886,52.7437899687123,-25.840688889265));
#28461=CARTESIAN_POINT('Ctrl Pts',(18.590837789328,52.8611479682325,-25.6827403660725));
#28462=CARTESIAN_POINT('Ctrl Pts',(16.8341139278605,50.3835326215309,-25.5247918428801));
#28463=CARTESIAN_POINT('Ctrl Pts',(17.9476917514034,47.5598883370406,-25.3668433196876));
#28464=CARTESIAN_POINT('Ctrl Pts',(20.9222496566812,46.945201449345,-25.2088947964952));
#28465=CARTESIAN_POINT('Ctrl Pts',(23.0602749756965,49.1072111470821,-25.0509462733026));
#28466=CARTESIAN_POINT('Ctrl Pts',(22.6353686625552,51.076838858248,-24.945647257841));
#28467=CARTESIAN_POINT('Ctrl Pts',(22.0543315503421,51.7564253212268,-24.8929977501102));
#28468=CARTESIAN_POINT('Ctrl Pts',(20.6501999979751,47.5679131979649,-40.3210067496694));
#28469=CARTESIAN_POINT('Ctrl Pts',(21.4547503964622,47.7830036573307,-40.2683572419386));
#28470=CARTESIAN_POINT('Ctrl Pts',(22.8200823843564,49.0706957888647,-40.1630582264769));
#28471=CARTESIAN_POINT('Ctrl Pts',(22.3196261745956,51.8582633078185,-40.0051097032845));
#28472=CARTESIAN_POINT('Ctrl Pts',(19.7120664000098,52.9558123354376,-39.847161180092));
#28473=CARTESIAN_POINT('Ctrl Pts',(17.3675351437619,51.37592634054,-39.6892126568996));
#28474=CARTESIAN_POINT('Ctrl Pts',(17.4087931940007,48.5472769306665,-39.5312641337071));
#28475=CARTESIAN_POINT('Ctrl Pts',(19.7999150217428,47.0363960316603,-39.3733156105147));
#28476=CARTESIAN_POINT('Ctrl Pts',(22.3721989980166,48.212208974874,-39.2153670873221));
#28477=CARTESIAN_POINT('Ctrl Pts',(22.79380727004,51.0091162616619,-39.0574185641297));
#28478=CARTESIAN_POINT('Ctrl Pts',(20.6822926823065,52.8910088627665,-38.8994700409372));
#28479=CARTESIAN_POINT('Ctrl Pts',(17.9521956040134,52.151751668574,-38.7415215177447));
#28480=CARTESIAN_POINT('Ctrl Pts',(17.0787646510314,49.4615465796377,-38.5835729945523));
#28481=CARTESIAN_POINT('Ctrl Pts',(18.8539368997708,47.2595509266246,-38.4256244713598));
#28482=CARTESIAN_POINT('Ctrl Pts',(21.6682057091455,47.5422320301962,-38.2676759481674));
#28483=CARTESIAN_POINT('Ctrl Pts',(22.9699651456302,50.0532991496622,-38.1097274249748));
#28484=CARTESIAN_POINT('Ctrl Pts',(21.5789465036507,52.5160402716292,-37.9517789017824));
#28485=CARTESIAN_POINT('Ctrl Pts',(18.7563455947847,52.6975648439231,-37.7938303785899));
#28486=CARTESIAN_POINT('Ctrl Pts',(17.0613280566787,50.4332890921241,-37.6358818553975));
#28487=CARTESIAN_POINT('Ctrl Pts',(18.0307151217059,47.7761634605487,-37.477933332205));
#28488=CARTESIAN_POINT('Ctrl Pts',(20.7855928286004,47.135322702909,-37.3199848090125));
#28489=CARTESIAN_POINT('Ctrl Pts',(22.8281974427715,49.0917977662346,-37.1620362858201));
#28490=CARTESIAN_POINT('Ctrl Pts',(22.306561435123,51.8717121526415,-37.0040877626276));
#28491=CARTESIAN_POINT('Ctrl Pts',(19.6936363332786,52.9546020661232,-36.8461392394351));
#28492=CARTESIAN_POINT('Ctrl Pts',(17.3584818463344,51.3586441412256,-36.6881907162427));
#28493=CARTESIAN_POINT('Ctrl Pts',(17.4183115332283,48.5308448973769,-36.5302421930502));
#28494=CARTESIAN_POINT('Ctrl Pts',(19.8188796334077,47.0350839014358,-36.3722936698577));
#28495=CARTESIAN_POINT('Ctrl Pts',(22.3836640619672,48.2275221588729,-36.2143451466653));
#28496=CARTESIAN_POINT('Ctrl Pts',(22.7872527811463,51.0270121670532,-36.0563966234728));
#28497=CARTESIAN_POINT('Ctrl Pts',(20.663724174252,52.8953414786953,-35.8984481002803));
#28498=CARTESIAN_POINT('Ctrl Pts',(17.9384170447561,52.1385527293516,-35.7404995770879));
#28499=CARTESIAN_POINT('Ctrl Pts',(17.0822844806015,49.4428032614878,-35.5825510538953));
#28500=CARTESIAN_POINT('Ctrl Pts',(18.8715558395627,47.2522471300393,-35.4246025307029));
#28501=CARTESIAN_POINT('Ctrl Pts',(21.683953198723,47.5529949566688,-35.2666540075104));
#28502=CARTESIAN_POINT('Ctrl Pts',(22.9695614077184,50.0723678337872,-35.108705484318));
#28503=CARTESIAN_POINT('Ctrl Pts',(21.5627586034653,52.5261269969816,-34.9507569611255));
#28504=CARTESIAN_POINT('Ctrl Pts',(18.7390501026036,52.6895236406911,-34.7928084379331));
#28505=CARTESIAN_POINT('Ctrl Pts',(17.0586065236542,50.4144109975506,-34.6348599147405));
#28506=CARTESIAN_POINT('Ctrl Pts',(18.0450349512685,47.7635645066714,-34.4769113915481));
#28507=CARTESIAN_POINT('Ctrl Pts',(20.8039707309936,47.1404260594826,-34.3189628683556));
#28508=CARTESIAN_POINT('Ctrl Pts',(22.8339707005912,49.1099763341506,-34.1610143451632));
#28509=CARTESIAN_POINT('Ctrl Pts',(22.2944956272855,51.8864839977984,-34.0030658219707));
#28510=CARTESIAN_POINT('Ctrl Pts',(19.67467115265,52.9525739954594,-33.8451172987782));
#28511=CARTESIAN_POINT('Ctrl Pts',(17.3498124494772,51.3416549499163,-33.6871687755857));
#28512=CARTESIAN_POINT('Ctrl Pts',(17.4277981965525,48.5142981658749,-33.5292202523933));
#28513=CARTESIAN_POINT('Ctrl Pts',(19.8379210888321,47.0339820492559,-33.3712717292008));
#28514=CARTESIAN_POINT('Ctrl Pts',(22.3949960004604,48.2428642012184,-33.2133232060084));
#28515=CARTESIAN_POINT('Ctrl Pts',(22.7806008789819,51.0448879410665,-33.0553746828159));
#28516=CARTESIAN_POINT('Ctrl Pts',(20.6451195086835,52.8995435635799,-32.8974261596234));
#28517=CARTESIAN_POINT('Ctrl Pts',(17.9247279002847,52.1252712226264,-32.7394776364309));
#28518=CARTESIAN_POINT('Ctrl Pts',(17.0859223881499,49.4240801013201,-32.5815291132385));
#28519=CARTESIAN_POINT('Ctrl Pts',(18.8892224190154,47.2450580363348,-32.423580590046));
#28520=CARTESIAN_POINT('Ctrl Pts',(21.6996306997866,47.5638580620325,-32.2656320668536));
#28521=CARTESIAN_POINT('Ctrl Pts',(22.9690355169923,50.0914338909774,-32.1076835436611));
#28522=CARTESIAN_POINT('Ctrl Pts',(21.5465061300745,52.5361093918092,-31.9497350204686));
#28523=CARTESIAN_POINT('Ctrl Pts',(18.721806669876,52.6813716393681,-31.7917864972762));
#28524=CARTESIAN_POINT('Ctrl Pts',(17.056006227608,50.3955157717439,-31.6338379740837));
#28525=CARTESIAN_POINT('Ctrl Pts',(18.0594354012447,47.7510577829479,-31.4758894508912));
#28526=CARTESIAN_POINT('Ctrl Pts',(20.8223154769685,47.1456473038675,-31.3179409276987));
#28527=CARTESIAN_POINT('Ctrl Pts',(22.8396271193197,49.1281916031572,-31.1599924045063));
#28528=CARTESIAN_POINT('Ctrl Pts',(22.2823352159385,51.9011780610106,-31.0020438813138));
#28529=CARTESIAN_POINT('Ctrl Pts',(19.6557193863538,52.9504241926626,-30.8440953581213));
#28530=CARTESIAN_POINT('Ctrl Pts',(17.3412523183405,51.3246104419229,-30.6861468349288));
#28531=CARTESIAN_POINT('Ctrl Pts',(17.4373909111324,48.4978126896975,-30.5281983117364));
#28532=CARTESIAN_POINT('Ctrl Pts',(19.8569692265682,47.0330024847609,-30.370249788544));
#28533=CARTESIAN_POINT('Ctrl Pts',(22.4062291941903,48.2582786897427,-30.2123012653514));
#28534=CARTESIAN_POINT('Ctrl Pts',(22.773834333593,51.0627206346725,-30.054352742159));
#28535=CARTESIAN_POINT('Ctrl Pts',(20.6264882450843,52.9036261013384,-29.8964042189665));
#28536=CARTESIAN_POINT('Ctrl Pts',(17.9111243185372,52.1119020917034,-29.738455695774));
#28537=CARTESIAN_POINT('Ctrl Pts',(17.0896804420887,49.4053806861463,-29.5805071725816));
#28538=CARTESIAN_POINT('Ctrl Pts',(18.9069347954335,47.2379825278782,-29.4225586493891));
#28539=CARTESIAN_POINT('Ctrl Pts',(21.7152381256765,47.5748216087247,-29.2646101261967));
#28540=CARTESIAN_POINT('Ctrl Pts',(22.9683872139918,50.1104961782632,-29.1066616030042));
#28541=CARTESIAN_POINT('Ctrl Pts',(21.5301898947694,52.5459872239793,-28.9487130798117));
#28542=CARTESIAN_POINT('Ctrl Pts',(18.7046159366362,52.6731090855795,-28.7907645566193));
#28543=CARTESIAN_POINT('Ctrl Pts',(17.0535273113208,50.3766042398849,-28.6328160334267));
#28544=CARTESIAN_POINT('Ctrl Pts',(18.0739158601312,47.7386437804777,-28.4748675102343));
#28545=CARTESIAN_POINT('Ctrl Pts',(20.840626318929,47.1509862358588,-28.3169189870418));
#28546=CARTESIAN_POINT('Ctrl Pts',(22.8451664617045,49.1464428092345,-28.1589704638493));
#28547=CARTESIAN_POINT('Ctrl Pts',(22.2700807037733,51.9157937538193,-28.0010219406569));
#28548=CARTESIAN_POINT('Ctrl Pts',(19.6367818165101,52.9481527160679,-27.8430734174644));
#28549=CARTESIAN_POINT('Ctrl Pts',(17.3328018026754,51.3075113781554,-27.685124894272));
#28550=CARTESIAN_POINT('Ctrl Pts',(17.4470892886469,48.4813890338076,-27.5271763710795));
#28551=CARTESIAN_POINT('Ctrl Pts',(19.8760232465397,47.0321454761979,-27.369227847887));
#28552=CARTESIAN_POINT('Ctrl Pts',(22.4173632095528,48.2737645355534,-27.2112793246945));
#28553=CARTESIAN_POINT('Ctrl Pts',(22.7669533650514,51.0805104150582,-27.0533308015021));
#28554=CARTESIAN_POINT('Ctrl Pts',(20.6078312689498,52.9075871271482,-26.8953822783096));
#28555=CARTESIAN_POINT('Ctrl Pts',(17.897606626764,52.0984494642799,-26.7374337551172));
#28556=CARTESIAN_POINT('Ctrl Pts',(17.0935589525871,49.3866986667662,-26.5794852319246));
#28557=CARTESIAN_POINT('Ctrl Pts',(18.9246913125752,47.2310350714261,-26.4215367087322));
#28558=CARTESIAN_POINT('Ctrl Pts',(21.7307766763484,47.5858569246444,-26.2635881855397));
#28559=CARTESIAN_POINT('Ctrl Pts',(22.9676128554771,50.129610091114,-26.1056396623473));
#28560=CARTESIAN_POINT('Ctrl Pts',(21.5138178763438,52.5556482381081,-25.9476911391548));
#28561=CARTESIAN_POINT('Ctrl Pts',(18.687464069051,52.6649589973579,-25.7897426159623));
#28562=CARTESIAN_POINT('Ctrl Pts',(17.0511987963454,50.3572337823409,-25.6317940927699));
#28563=CARTESIAN_POINT('Ctrl Pts',(18.0884185672411,47.7272068404143,-25.4738455695774));
#28564=CARTESIAN_POINT('Ctrl Pts',(20.859010980093,47.1546690443582,-25.3158970463849));
#28565=CARTESIAN_POINT('Ctrl Pts',(22.8504318621136,49.168429695793,-25.1579485231925));
#28566=CARTESIAN_POINT('Ctrl Pts',(22.4546613829867,51.0029999971534,-25.0526495077308));
#28567=CARTESIAN_POINT('Ctrl Pts',(21.9134659966651,51.6359872033749,-25.));
#28568=CARTESIAN_POINT('Ctrl Pts',(22.5149457203491,50.0017607375679,-39.112583302492));
#28569=CARTESIAN_POINT('Ctrl Pts',(22.5168589401434,50.2933091215384,-39.0941950563712));
#28570=CARTESIAN_POINT('Ctrl Pts',(22.4699889263606,50.5842626639725,-39.0758068102504));
#28571=CARTESIAN_POINT('Ctrl Pts',(22.3716201267472,50.856613814048,-39.0574185641297));
#28572=CARTESIAN_POINT('Ctrl Pts',(22.0899690741288,51.6364137953635,-39.0047690563988));
#28573=CARTESIAN_POINT('Ctrl Pts',(21.3861308782177,52.263711329065,-38.952119548668));
#28574=CARTESIAN_POINT('Ctrl Pts',(20.5791956005466,52.4541505635503,-38.8994700409372));
#28575=CARTESIAN_POINT('Ctrl Pts',(19.7722603228755,52.6445897980356,-38.8468205332064));
#28576=CARTESIAN_POINT('Ctrl Pts',(18.8622279634444,52.3981707333048,-38.7941710254756));
#28577=CARTESIAN_POINT('Ctrl Pts',(18.2616399582319,51.8265936861167,-38.7415215177447));
#28578=CARTESIAN_POINT('Ctrl Pts',(17.6610519530194,51.2550166389285,-38.6888720100139));
#28579=CARTESIAN_POINT('Ctrl Pts',(17.3699083020254,50.3582816092831,-38.6362225022831));
#28580=CARTESIAN_POINT('Ctrl Pts',(17.520198517985,49.5429148189582,-38.5835729945523));
#28581=CARTESIAN_POINT('Ctrl Pts',(17.6704887339445,48.7275480286333,-38.5309234868215));
#28582=CARTESIAN_POINT('Ctrl Pts',(18.2622128168577,47.993549477629,-38.4782739790906));
#28583=CARTESIAN_POINT('Ctrl Pts',(19.0271196598767,47.6736637193888,-38.4256244713598));
#28584=CARTESIAN_POINT('Ctrl Pts',(19.7920265028957,47.3537779611485,-38.372974963629));
#28585=CARTESIAN_POINT('Ctrl Pts',(20.7301161060206,47.4480049956724,-38.3203254558982));
#28586=CARTESIAN_POINT('Ctrl Pts',(21.4161208136638,47.913629699512,-38.2676759481674));
#28587=CARTESIAN_POINT('Ctrl Pts',(22.0897218255865,48.3708354128081,-38.2159783996089));
#28588=CARTESIAN_POINT('Ctrl Pts',(22.520271455965,49.1861296837586,-38.1642808510504));
#28589=CARTESIAN_POINT('Ctrl Pts',(22.5215367446411,50.0002732851607,-38.112583302492));
#28590=CARTESIAN_POINT('Origin',(20.,50.,-32.));
#28591=CARTESIAN_POINT('',(20.,47.4825,-24.3199761284063));
#28592=CARTESIAN_POINT('Ctrl Pts',(17.4825,50.,-25.));
#28593=CARTESIAN_POINT('Ctrl Pts',(17.4825,49.6777819917977,-25.));
#28594=CARTESIAN_POINT('Ctrl Pts',(17.5480817994189,49.3379042845386,-24.965994767533));
#28595=CARTESIAN_POINT('Ctrl Pts',(17.8069078640769,48.7191330360028,-24.8434341672334));
#28596=CARTESIAN_POINT('Ctrl Pts',(17.9998598225217,48.439857534204,-24.75619390213));
#28597=CARTESIAN_POINT('Ctrl Pts',(18.4404784589042,47.9992388978215,-24.5883213994305));
#28598=CARTESIAN_POINT('Ctrl Pts',(18.7195457648911,47.8067418484832,-24.4956547875015));
#28599=CARTESIAN_POINT('Ctrl Pts',(19.3374025937984,47.5482850278898,-24.3600905047278));
#28600=CARTESIAN_POINT('Ctrl Pts',(19.6768725637946,47.4825,-24.3199761284063));
#28601=CARTESIAN_POINT('Ctrl Pts',(20.,47.4825,-24.3199761284063));
#28602=CARTESIAN_POINT('Ctrl Pts',(20.,47.4825,-24.3199761284063));
#28603=CARTESIAN_POINT('Ctrl Pts',(20.3231274362054,47.4825,-24.3199761284063));
#28604=CARTESIAN_POINT('Ctrl Pts',(20.6625974062016,47.5482850278898,-24.3600905047278));
#28605=CARTESIAN_POINT('Ctrl Pts',(21.2804542351089,47.8067418484832,-24.4956547875015));
#28606=CARTESIAN_POINT('Ctrl Pts',(21.5595215410957,47.9992388978215,-24.5883213994305));
#28607=CARTESIAN_POINT('Ctrl Pts',(22.0001401774783,48.439857534204,-24.75619390213));
#28608=CARTESIAN_POINT('Ctrl Pts',(22.1930921359231,48.7191330360027,-24.8434341672334));
#28609=CARTESIAN_POINT('Ctrl Pts',(22.4519182005811,49.3379042845385,-24.965994767533));
#28610=CARTESIAN_POINT('Ctrl Pts',(22.5175,49.6777819917977,-25.));
#28611=CARTESIAN_POINT('Ctrl Pts',(22.5175,50.,-25.));
#28612=CARTESIAN_POINT('Origin',(20.,-50.,-25.));
#28613=CARTESIAN_POINT('',(17.2889091698078,-50.0014754277217,-25.));
#28614=CARTESIAN_POINT('',(20.,-50.,-25.));
#28615=CARTESIAN_POINT('Ctrl Pts',(17.2903183448191,-50.0029508554434,-25.));
#28616=CARTESIAN_POINT('Ctrl Pts',(17.3003555066451,-49.9104827882475,-25.));
#28617=CARTESIAN_POINT('Ctrl Pts',(17.314987256537,-49.8185880473882,-25.));
#28618=CARTESIAN_POINT('Ctrl Pts',(17.3341159214449,-49.7276468529595,-25.));
#28619=CARTESIAN_POINT('Ctrl Pts',(17.3530416128693,-49.6376706318372,-25.));
#28620=CARTESIAN_POINT('Ctrl Pts',(17.3763697440335,-49.548626955546,-25.));
#28621=CARTESIAN_POINT('Ctrl Pts',(17.4040502591901,-49.4609077193442,-25.));
#28622=CARTESIAN_POINT('Ctrl Pts',(17.4311163521567,-49.3751355800408,-25.));
#28623=CARTESIAN_POINT('Ctrl Pts',(17.4623442184204,-49.2906290498442,-25.));
#28624=CARTESIAN_POINT('Ctrl Pts',(17.4977230490407,-49.2077885578907,-25.));
#28625=CARTESIAN_POINT('Ctrl Pts',(17.5030373904386,-49.1953448832951,-25.));
#28626=CARTESIAN_POINT('Ctrl Pts',(17.5084454535136,-49.1829388756344,-25.));
#28627=CARTESIAN_POINT('Ctrl Pts',(17.5139472640597,-49.1705719750047,-25.));
#28628=CARTESIAN_POINT('Ctrl Pts',(17.5197445971897,-49.1575408024235,-25.));
#28629=CARTESIAN_POINT('Ctrl Pts',(17.5256427865735,-49.1445603815785,-25.));
#28630=CARTESIAN_POINT('Ctrl Pts',(17.5316393957237,-49.1316366890192,-25.));
#28631=CARTESIAN_POINT('Ctrl Pts',(17.5691316190762,-49.0508346964552,-25.));
#28632=CARTESIAN_POINT('Ctrl Pts',(17.6104933170903,-48.9721902576076,-25.));
#28633=CARTESIAN_POINT('Ctrl Pts',(17.6556547793454,-48.8960514827779,-25.));
#28634=CARTESIAN_POINT('Ctrl Pts',(17.7000564683813,-48.8211936275458,-25.));
#28635=CARTESIAN_POINT('Ctrl Pts',(17.7481316008788,-48.7487571677604,-25.));
#28636=CARTESIAN_POINT('Ctrl Pts',(17.7998501145092,-48.6791071342385,-25.));
#28637=CARTESIAN_POINT('Ctrl Pts',(17.8499884747111,-48.6115851150686,-25.));
#28638=CARTESIAN_POINT('Ctrl Pts',(17.9035514278317,-48.5466814150452,-25.));
#28639=CARTESIAN_POINT('Ctrl Pts',(17.9605392673115,-48.4847689190164,-25.));
#28640=CARTESIAN_POINT('Ctrl Pts',(17.9814440129101,-48.4620576706049,-25.));
#28641=CARTESIAN_POINT('Ctrl Pts',(18.0028098640902,-48.439749359775,-25.));
#28642=CARTESIAN_POINT('Ctrl Pts',(18.0246376377076,-48.4178639875036,-25.));
#28643=CARTESIAN_POINT('Ctrl Pts',(18.0437154987664,-48.3987357842003,-25.));
#28644=CARTESIAN_POINT('Ctrl Pts',(18.0631462461595,-48.3799306892336,-25.));
#28645=CARTESIAN_POINT('Ctrl Pts',(18.082919744614,-48.3614538208575,-25.));
#28646=CARTESIAN_POINT('Origin',(20.,-50.,-25.));
#28647=CARTESIAN_POINT('',(22.7115649000387,-50.0018225476882,-25.));
#28648=CARTESIAN_POINT('',(20.,-50.,-25.));
#28649=CARTESIAN_POINT('Ctrl Pts',(22.7106298000774,-50.0036450953763,-25.));
#28650=CARTESIAN_POINT('Ctrl Pts',(22.7207569197221,-50.0952816165228,-25.));
#28651=CARTESIAN_POINT('Ctrl Pts',(22.7262771338965,-50.1873822523437,-25.));
#28652=CARTESIAN_POINT('Ctrl Pts',(22.7270618926046,-50.2795961166426,-25.));
#28653=CARTESIAN_POINT('Ctrl Pts',(22.7273478963458,-50.3132032750016,-25.));
#28654=CARTESIAN_POINT('Ctrl Pts',(22.7270044421126,-50.3468255682447,-25.));
#28655=CARTESIAN_POINT('Ctrl Pts',(22.7260235824556,-50.3804462077869,-25.));
#28656=CARTESIAN_POINT('Ctrl Pts',(22.7254183178835,-50.4011926844725,-25.));
#28657=CARTESIAN_POINT('Ctrl Pts',(22.72456984669,-50.4219453082198,-25.));
#28658=CARTESIAN_POINT('Ctrl Pts',(22.723478332626,-50.4426647798907,-25.));
#28659=CARTESIAN_POINT('Ctrl Pts',(22.7184413506502,-50.5382783947722,-25.));
#28660=CARTESIAN_POINT('Ctrl Pts',(22.7082324366332,-50.6332960684915,-25.));
#28661=CARTESIAN_POINT('Ctrl Pts',(22.6927834477001,-50.7273214749238,-25.));
#28662=CARTESIAN_POINT('Ctrl Pts',(22.6895870066842,-50.7467756066445,-25.));
#28663=CARTESIAN_POINT('Ctrl Pts',(22.6861660794599,-50.7661873278843,-25.));
#28664=CARTESIAN_POINT('Ctrl Pts',(22.6825197987883,-50.7855532193863,-25.));
#28665=CARTESIAN_POINT('Ctrl Pts',(22.665577577038,-50.8755356584169,-25.));
#28666=CARTESIAN_POINT('Ctrl Pts',(22.6437744061299,-50.964528503021,-25.));
#28667=CARTESIAN_POINT('Ctrl Pts',(22.6174131158025,-51.0522992055656,-25.));
#28668=CARTESIAN_POINT('Ctrl Pts',(22.590454590549,-51.1420584196133,-25.));
#28669=CARTESIAN_POINT('Ctrl Pts',(22.558728861846,-51.2305401876501,-25.));
#28670=CARTESIAN_POINT('Ctrl Pts',(22.5225055623892,-51.3174921359681,-25.));
#28671=CARTESIAN_POINT('Ctrl Pts',(22.5100288523632,-51.3474417612542,-25.));
#28672=CARTESIAN_POINT('Ctrl Pts',(22.4970181100108,-51.3772098108535,-25.));
#28673=CARTESIAN_POINT('Ctrl Pts',(22.4834829864678,-51.4067856342665,-25.));
#28674=CARTESIAN_POINT('Ctrl Pts',(22.4768071327121,-51.4213731532634,-25.));
#28675=CARTESIAN_POINT('Ctrl Pts',(22.4700037022852,-51.4359139058754,-25.));
#28676=CARTESIAN_POINT('Ctrl Pts',(22.4630737944401,-51.4504065918778,-25.));
#28677=CARTESIAN_POINT('Ctrl Pts',(22.4569722275614,-51.4631669481296,-25.));
#28678=CARTESIAN_POINT('Ctrl Pts',(22.4507733728518,-51.4758883159868,-25.));
#28679=CARTESIAN_POINT('Ctrl Pts',(22.4444834321049,-51.4885593435834,-25.));
#28680=CARTESIAN_POINT('Ctrl Pts',(22.4016240141549,-51.5748992455749,-25.));
#28681=CARTESIAN_POINT('Ctrl Pts',(22.3544754754652,-51.6590378348422,-25.));
#28682=CARTESIAN_POINT('Ctrl Pts',(22.303380378344,-51.7407248629369,-25.));
#28683=CARTESIAN_POINT('Ctrl Pts',(22.2512756047644,-51.8240260864021,-25.));
#28684=CARTESIAN_POINT('Ctrl Pts',(22.1950664422593,-51.9047786755034,-25.));
#28685=CARTESIAN_POINT('Ctrl Pts',(22.1350611970561,-51.9827100860122,-25.));
#28686=CARTESIAN_POINT('Ctrl Pts',(22.0745775675633,-52.0612627949147,-25.));
#28687=CARTESIAN_POINT('Ctrl Pts',(22.0102366253224,-52.1369500006744,-25.));
#28688=CARTESIAN_POINT('Ctrl Pts',(21.9423048690762,-52.2094731543011,-25.));
#28689=CARTESIAN_POINT('Ctrl Pts',(21.9053590736893,-52.2489160561597,-25.));
#28690=CARTESIAN_POINT('Ctrl Pts',(21.8673503377721,-52.2874226510328,-25.));
#28691=CARTESIAN_POINT('Ctrl Pts',(21.8283162532303,-52.3249411517793,-25.));
#28692=CARTESIAN_POINT('Ctrl Pts',(21.815658940581,-52.3371070165525,-25.));
#28693=CARTESIAN_POINT('Ctrl Pts',(21.80289378929,-52.3491689621023,-25.));
#28694=CARTESIAN_POINT('Ctrl Pts',(21.7900220062658,-52.361125148447,-25.));
#28695=CARTESIAN_POINT('Ctrl Pts',(21.7785378626427,-52.3717924010652,-25.));
#28696=CARTESIAN_POINT('Ctrl Pts',(21.7669742197933,-52.3823704194089,-25.));
#28697=CARTESIAN_POINT('Ctrl Pts',(21.755337497437,-52.3928534389456,-25.));
#28698=CARTESIAN_POINT('Ctrl Pts',(21.6795227363725,-52.4611516759468,-25.));
#28699=CARTESIAN_POINT('Ctrl Pts',(21.6005417920538,-52.5254825537856,-25.));
#28700=CARTESIAN_POINT('Ctrl Pts',(21.5187210399691,-52.5855630198017,-25.));
#28701=CARTESIAN_POINT('Ctrl Pts',(21.4368278994846,-52.6456966401667,-25.));
#28702=CARTESIAN_POINT('Ctrl Pts',(21.3520893470422,-52.7015731625802,-25.));
#28703=CARTESIAN_POINT('Ctrl Pts',(21.2647876555901,-52.7528825881287,-25.));
#28704=CARTESIAN_POINT('Ctrl Pts',(21.1792482097518,-52.8031562970879,-25.));
#28705=CARTESIAN_POINT('Ctrl Pts',(21.0912473933424,-52.8490461032894,-25.));
#28706=CARTESIAN_POINT('Ctrl Pts',(21.0010169754817,-52.8902242643499,-25.));
#28707=CARTESIAN_POINT('Ctrl Pts',(20.9635971996838,-52.9073014051988,-25.));
#28708=CARTESIAN_POINT('Ctrl Pts',(20.9257936105469,-52.9235677108145,-25.));
#28709=CARTESIAN_POINT('Ctrl Pts',(20.8876213902621,-52.9389975058256,-25.));
#28710=CARTESIAN_POINT('Ctrl Pts',(20.8571996693011,-52.9512944305214,-25.));
#28711=CARTESIAN_POINT('Ctrl Pts',(20.8265437968036,-52.9630600190333,-25.));
#28712=CARTESIAN_POINT('Ctrl Pts',(20.7956660331737,-52.9742969611506,-25.));
#28713=CARTESIAN_POINT('Ctrl Pts',(19.2062007174671,-52.9692229537457,-25.));
#28714=CARTESIAN_POINT('Ctrl Pts',(19.1113557340264,-52.9345282351333,-25.));
#28715=CARTESIAN_POINT('Ctrl Pts',(19.0185538161309,-52.8948451940055,-25.));
#28716=CARTESIAN_POINT('Ctrl Pts',(18.9280360947249,-52.8504935528002,-25.));
#28717=CARTESIAN_POINT('Ctrl Pts',(18.8362532909695,-52.8055220497869,-25.));
#28718=CARTESIAN_POINT('Ctrl Pts',(18.7468183096923,-52.7557498361634,-25.));
#28719=CARTESIAN_POINT('Ctrl Pts',(18.6600165620743,-52.7014695591135,-25.));
#28720=CARTESIAN_POINT('Ctrl Pts',(18.6355003880952,-52.6861387074624,-25.));
#28721=CARTESIAN_POINT('Ctrl Pts',(18.6111945114723,-52.670448030549,-25.));
#28722=CARTESIAN_POINT('Ctrl Pts',(18.5871059592391,-52.6544036660335,-25.));
#28723=CARTESIAN_POINT('Ctrl Pts',(18.5677885117881,-52.6415371323618,-25.));
#28724=CARTESIAN_POINT('Ctrl Pts',(18.5486087336159,-52.6284415254607,-25.));
#28725=CARTESIAN_POINT('Ctrl Pts',(18.529589504657,-52.6151337510479,-25.));
#28726=CARTESIAN_POINT('Ctrl Pts',(18.4468808900083,-52.5572624467948,-25.));
#28727=CARTESIAN_POINT('Ctrl Pts',(18.3671268631708,-52.4953308830207,-25.));
#28728=CARTESIAN_POINT('Ctrl Pts',(18.290593905947,-52.4296356749819,-25.));
#28729=CARTESIAN_POINT('Ctrl Pts',(18.2315992466026,-52.3789951854543,-25.));
#28730=CARTESIAN_POINT('Ctrl Pts',(18.1745191630826,-52.3261174497872,-25.));
#28731=CARTESIAN_POINT('Ctrl Pts',(18.119493278307,-52.2711265564765,-25.));
#28732=CARTESIAN_POINT('Ctrl Pts',(18.0902009918943,-52.2418528972976,-25.));
#28733=CARTESIAN_POINT('Ctrl Pts',(18.0614911051503,-52.2119802581191,-25.));
#28734=CARTESIAN_POINT('Ctrl Pts',(18.0333867031721,-52.1815265260884,-25.));
#28735=CARTESIAN_POINT('Ctrl Pts',(18.0237500866723,-52.1710843563246,-25.));
#28736=CARTESIAN_POINT('Ctrl Pts',(18.0141853970817,-52.1605745812859,-25.));
#28737=CARTESIAN_POINT('Ctrl Pts',(18.0047001952164,-52.1500055259558,-25.));
#28738=CARTESIAN_POINT('Ctrl Pts',(17.938901944737,-52.0766886519643,-25.));
#28739=CARTESIAN_POINT('Ctrl Pts',(17.8768357908346,-52.0004252935808,-25.));
#28740=CARTESIAN_POINT('Ctrl Pts',(17.8187456099699,-51.9214932933958,-25.));
#28741=CARTESIAN_POINT('Ctrl Pts',(17.7611818199286,-51.8432765445658,-25.));
#28742=CARTESIAN_POINT('Ctrl Pts',(17.7075218378801,-51.7624385159295,-25.));
#28743=CARTESIAN_POINT('Ctrl Pts',(17.6580487138489,-51.6792271703209,-25.));
#28744=CARTESIAN_POINT('Ctrl Pts',(17.6099913564333,-51.5983970740766,-25.));
#28745=CARTESIAN_POINT('Ctrl Pts',(17.5658844479073,-51.5153268531393,-25.));
#28746=CARTESIAN_POINT('Ctrl Pts',(17.5260352107221,-51.4302334377047,-25.));
#28747=CARTESIAN_POINT('Ctrl Pts',(17.5052301251829,-51.3858065951351,-25.));
#28748=CARTESIAN_POINT('Ctrl Pts',(17.4855864271477,-51.340828153884,-25.));
#28749=CARTESIAN_POINT('Ctrl Pts',(17.4671535333325,-51.2953287461456,-25.));
#28750=CARTESIAN_POINT('Ctrl Pts',(17.4600944809444,-51.2779043142537,-25.));
#28751=CARTESIAN_POINT('Ctrl Pts',(17.4532130454223,-51.2604034796238,-25.));
#28752=CARTESIAN_POINT('Ctrl Pts',(17.4465121643074,-51.2428279712876,-25.));
#28753=CARTESIAN_POINT('Ctrl Pts',(17.441270730006,-51.2290803953082,-25.));
#28754=CARTESIAN_POINT('Ctrl Pts',(17.4361396681845,-51.2152866325184,-25.));
#28755=CARTESIAN_POINT('Ctrl Pts',(17.4311255127051,-51.2014622180439,-25.));
#28756=CARTESIAN_POINT('Ctrl Pts',(17.3994430851164,-51.1141113147183,-25.));
#28757=CARTESIAN_POINT('Ctrl Pts',(17.3723694636016,-51.0253970866411,-25.));
#28758=CARTESIAN_POINT('Ctrl Pts',(17.3501559694963,-50.9355424162655,-25.));
#28759=CARTESIAN_POINT('Ctrl Pts',(17.3451710965855,-50.9153783614734,-25.));
#28760=CARTESIAN_POINT('Ctrl Pts',(17.3404311765996,-50.8951568357486,-25.));
#28761=CARTESIAN_POINT('Ctrl Pts',(17.3359394106852,-50.874880302046,-25.));
#28762=CARTESIAN_POINT('Ctrl Pts',(17.3155162874091,-50.7826871300692,-25.));
#28763=CARTESIAN_POINT('Ctrl Pts',(17.3002191225768,-50.6893564399051,-25.));
#28764=CARTESIAN_POINT('Ctrl Pts',(17.2899371061862,-50.5952837977441,-25.));
#28765=CARTESIAN_POINT('Ctrl Pts',(17.2792458523533,-50.4974669437472,-25.));
#28766=CARTESIAN_POINT('Ctrl Pts',(17.2739769598257,-50.3988466706342,-25.));
#28767=CARTESIAN_POINT('Ctrl Pts',(17.2740631823385,-50.2998823144491,-25.));
#28768=CARTESIAN_POINT('Ctrl Pts',(17.274090511577,-50.2685143990752,-25.));
#28769=CARTESIAN_POINT('Ctrl Pts',(17.274656255105,-50.2371120997174,-25.));
#28770=CARTESIAN_POINT('Ctrl Pts',(17.275759389936,-50.2056906513608,-25.));
#28771=CARTESIAN_POINT('Ctrl Pts',(17.2762350449305,-50.1921421997773,-25.));
#28772=CARTESIAN_POINT('Ctrl Pts',(17.2768107459306,-50.1785876877151,-25.));
#28773=CARTESIAN_POINT('Ctrl Pts',(17.2774860299861,-50.1650364244566,-25.));
#28774=CARTESIAN_POINT('Ctrl Pts',(17.2801856482179,-50.1108618336893,-25.));
#28775=CARTESIAN_POINT('Ctrl Pts',(17.2844721992041,-50.0568088877183,-25.));
#28776=CARTESIAN_POINT('Ctrl Pts',(17.2903183448191,-50.0029508554434,-25.));
#28777=CARTESIAN_POINT('',(20.,-50.,-25.));
#28778=CARTESIAN_POINT('Origin',(20.,-50.,-25.));
#28779=CARTESIAN_POINT('Origin',(20.,-50.,-25.));
#28780=CARTESIAN_POINT('',(20.,-50.,-25.));
#28781=CARTESIAN_POINT('Ctrl Pts',(21.9134659966651,-48.3640127966251,-25.));
#28782=CARTESIAN_POINT('Ctrl Pts',(21.9760669288874,-48.422842301107,-25.));
#28783=CARTESIAN_POINT('Ctrl Pts',(22.0352442468464,-48.4849719549136,-25.));
#28784=CARTESIAN_POINT('Ctrl Pts',(22.0909851470911,-48.5500174517208,-25.));
#28785=CARTESIAN_POINT('Ctrl Pts',(22.1343868534266,-48.6006640243179,-25.));
#28786=CARTESIAN_POINT('Ctrl Pts',(22.1757047718733,-48.6530795405248,-25.));
#28787=CARTESIAN_POINT('Ctrl Pts',(22.2149215330014,-48.7071012290448,-25.));
#28788=CARTESIAN_POINT('Ctrl Pts',(22.2385444426018,-48.7396421484798,-25.));
#28789=CARTESIAN_POINT('Ctrl Pts',(22.2614047541017,-48.7727661601668,-25.));
#28790=CARTESIAN_POINT('Ctrl Pts',(22.2834966880046,-48.8064400758587,-25.));
#28791=CARTESIAN_POINT('Ctrl Pts',(22.2954178781671,-48.8246111039924,-25.));
#28792=CARTESIAN_POINT('Ctrl Pts',(22.3071166390413,-48.8429446974121,-25.));
#28793=CARTESIAN_POINT('Ctrl Pts',(22.3185793921054,-48.8614149655927,-25.));
#28794=CARTESIAN_POINT('Ctrl Pts',(22.3655669620942,-48.9371274069235,-25.));
#28795=CARTESIAN_POINT('Ctrl Pts',(22.4086383333277,-49.0152023023888,-25.));
#28796=CARTESIAN_POINT('Ctrl Pts',(22.4477590648795,-49.0952575499459,-25.));
#28797=CARTESIAN_POINT('Ctrl Pts',(22.4825526073179,-49.1664577944914,-25.));
#28798=CARTESIAN_POINT('Ctrl Pts',(22.5142209063364,-49.2392255216741,-25.));
#28799=CARTESIAN_POINT('Ctrl Pts',(22.5427164245852,-49.3133158126709,-25.));
#28800=CARTESIAN_POINT('Ctrl Pts',(22.5500217400807,-49.3323101312216,-25.));
#28801=CARTESIAN_POINT('Ctrl Pts',(22.5571184055396,-49.3513914697327,-25.));
#28802=CARTESIAN_POINT('Ctrl Pts',(22.5640053609969,-49.37055588476,-25.));
#28803=CARTESIAN_POINT('Ctrl Pts',(22.5692935788638,-49.3852714731768,-25.));
#28804=CARTESIAN_POINT('Ctrl Pts',(22.5744581966978,-49.4000364270766,-25.));
#28805=CARTESIAN_POINT('Ctrl Pts',(22.5794941881025,-49.414835045487,-25.));
#28806=CARTESIAN_POINT('Ctrl Pts',(22.6091522636753,-49.5019874069421,-25.));
#28807=CARTESIAN_POINT('Ctrl Pts',(22.6343955017318,-49.5904229013513,-25.));
#28808=CARTESIAN_POINT('Ctrl Pts',(22.6551918733353,-49.6797461904936,-25.));
#28809=CARTESIAN_POINT('Ctrl Pts',(22.6763394154917,-49.7705778056766,-25.));
#28810=CARTESIAN_POINT('Ctrl Pts',(22.6928891491029,-49.8623282425449,-25.));
#28811=CARTESIAN_POINT('Ctrl Pts',(22.7047658933192,-49.9546151098704,-25.));
#28812=CARTESIAN_POINT('Ctrl Pts',(22.706867096187,-49.9709422637395,-25.));
#28813=CARTESIAN_POINT('Ctrl Pts',(22.7088219209409,-49.9872862726765,-25.));
#28814=CARTESIAN_POINT('Ctrl Pts',(22.7106298000774,-50.0036450953763,-25.));
#28815=CARTESIAN_POINT('Origin',(20.,-50.,-42.2084234471774));
#28816=CARTESIAN_POINT('Ctrl Pts',(23.0767447721987,-49.9980895972329,-39.7084234471774));
#28817=CARTESIAN_POINT('Ctrl Pts',(23.0776699202316,-49.8748204878272,-39.7020198504181));
#28818=CARTESIAN_POINT('Ctrl Pts',(23.0151644566962,-48.7389614167051,-39.642966745928));
#28819=CARTESIAN_POINT('Ctrl Pts',(21.6024148578293,-46.7464740991412,-39.5312641337071));
#28820=CARTESIAN_POINT('Ctrl Pts',(18.1518492862868,-46.8799264325519,-39.3733156105146));
#28821=CARTESIAN_POINT('Ctrl Pts',(16.3769778256201,-49.8417650264767,-39.2153670873222));
#28822=CARTESIAN_POINT('Ctrl Pts',(17.8869742727072,-52.9473163426722,-39.0574185641297));
#28823=CARTESIAN_POINT('Ctrl Pts',(21.3127949729971,-53.3805020684052,-38.8994700409372));
#28824=CARTESIAN_POINT('Ctrl Pts',(22.9593111902465,-51.4421740844442,-38.7831383352865));
#28825=CARTESIAN_POINT('Ctrl Pts',(23.0761866233546,-50.2155563599539,-38.7194561373666));
#28826=CARTESIAN_POINT('Ctrl Pts',(23.0742548311415,-50.0026845243509,-38.7084234471775));
#28827=CARTESIAN_POINT('Ctrl Pts',(23.0703065393339,-50.0033432771247,-39.7915765528225));
#28828=CARTESIAN_POINT('Ctrl Pts',(23.0652969395396,-49.3102241888876,-39.7557520197534));
#28829=CARTESIAN_POINT('Ctrl Pts',(22.4928180780877,-47.5885986835485,-39.6672779789534));
#28830=CARTESIAN_POINT('Ctrl Pts',(19.6484750771286,-46.3913839963408,-39.5261544304226));
#28831=CARTESIAN_POINT('Ctrl Pts',(16.7861445447059,-48.3201950030769,-39.3682059072301));
#28832=CARTESIAN_POINT('Ctrl Pts',(16.8365146481096,-51.7735627154933,-39.2102573840377));
#28833=CARTESIAN_POINT('Ctrl Pts',(19.7557254203512,-53.6181280557829,-39.0523088608451));
#28834=CARTESIAN_POINT('Ctrl Pts',(22.5305077858237,-52.349751264392,-38.9127485837735));
#28835=CARTESIAN_POINT('Ctrl Pts',(23.0660296945049,-50.6610395723575,-38.8258378144326));
#28836=CARTESIAN_POINT('Ctrl Pts',(23.0703817199364,-49.9978503929169,-38.7915765528226));
#28837=CARTESIAN_POINT('Ctrl Pts',(18.086534003335,-48.364012796625,-40.));
#28838=CARTESIAN_POINT('Ctrl Pts',(17.5453386170133,-48.9970000028465,-39.9473504922692));
#28839=CARTESIAN_POINT('Ctrl Pts',(17.1495688120533,-50.8315710151824,-39.8420514768075));
#28840=CARTESIAN_POINT('Ctrl Pts',(19.1409886760425,-52.8453306902491,-39.684102953615));
#28841=CARTESIAN_POINT('Ctrl Pts',(21.9115816382771,-52.2727934305225,-39.5261544304226));
#28842=CARTESIAN_POINT('Ctrl Pts',(22.9488012054458,-49.6427660783584,-39.3682059072301));
#28843=CARTESIAN_POINT('Ctrl Pts',(21.3125360027934,-47.3350410101149,-39.2102573840377));
#28844=CARTESIAN_POINT('Ctrl Pts',(18.4861820654716,-47.4443516492433,-39.0523088608452));
#28845=CARTESIAN_POINT('Ctrl Pts',(17.0323870753209,-49.8703899313991,-38.8943603376527));
#28846=CARTESIAN_POINT('Ctrl Pts',(18.2692232736426,-52.4141431243459,-38.7364118144602));
#28847=CARTESIAN_POINT('Ctrl Pts',(21.0753087179177,-52.7689650096666,-38.5784632912678));
#28848=CARTESIAN_POINT('Ctrl Pts',(22.9064411229281,-50.6133013449025,-38.4205147680753));
#28849=CARTESIAN_POINT('Ctrl Pts',(22.1023934291463,-47.9015504828899,-38.2625662448829));
#28850=CARTESIAN_POINT('Ctrl Pts',(19.3921687147818,-47.0924127949112,-38.1046177216903));
#28851=CARTESIAN_POINT('Ctrl Pts',(17.233046562173,-48.9194895571954,-37.9466691984979));
#28852=CARTESIAN_POINT('Ctrl Pts',(17.5826367266969,-51.7262355095391,-37.7887206753054));
#28853=CARTESIAN_POINT('Ctrl Pts',(20.1239767567563,-52.9678546022029,-37.630772152113));
#28854=CARTESIAN_POINT('Ctrl Pts',(22.5529107785992,-51.518611006092,-37.4728236289205));
#28855=CARTESIAN_POINT('Ctrl Pts',(22.6671982676034,-48.692488587455,-37.314875105728));
#28856=CARTESIAN_POINT('Ctrl Pts',(20.3632181930562,-47.0518472062269,-37.1569265825356));
#28857=CARTESIAN_POINT('Ctrl Pts',(17.7299192364194,-48.0842061957224,-36.9989780593431));
#28858=CARTESIAN_POINT('Ctrl Pts',(17.154833463334,-50.853557213245,-36.8410295361506));
#28859=CARTESIAN_POINT('Ctrl Pts',(19.1593736589235,-52.8490138392078,-36.6830810129582));
#28860=CARTESIAN_POINT('Ctrl Pts',(21.9260841906145,-52.2613562790991,-36.5251324897657));
#28861=CARTESIAN_POINT('Ctrl Pts',(22.9464727663089,-49.6233957501942,-36.3671839665733));
#28862=CARTESIAN_POINT('Ctrl Pts',(21.2953840974929,-47.3268908439923,-36.2092354433807));
#28863=CARTESIAN_POINT('Ctrl Pts',(18.4698100649153,-47.4540127089428,-36.0512869201883));
#28864=CARTESIAN_POINT('Ctrl Pts',(17.0316127078011,-49.8895038188253,-35.8933383969958));
#28865=CARTESIAN_POINT('Ctrl Pts',(18.2847618291327,-52.4251784551708,-35.7353898738034));
#28866=CARTESIAN_POINT('Ctrl Pts',(21.0930652333649,-52.7620175448917,-35.5774413506109));
#28867=CARTESIAN_POINT('Ctrl Pts',(22.9103196345885,-50.5946193295201,-35.4194928274184));
#28868=CARTESIAN_POINT('Ctrl Pts',(22.0888757364977,-47.8880978526551,-35.2615443042259));
#28869=CARTESIAN_POINT('Ctrl Pts',(19.3735117384099,-47.0963738221607,-35.1035957810335));
#28870=CARTESIAN_POINT('Ctrl Pts',(17.2261655933258,-48.9372793373283,-34.945647257841));
#28871=CARTESIAN_POINT('Ctrl Pts',(17.5937707424136,-51.7417213561457,-34.7876987346485));
#28872=CARTESIAN_POINT('Ctrl Pts',(20.1430307772,-52.9669975934097,-34.6297502114561));
#28873=CARTESIAN_POINT('Ctrl Pts',(22.5626091563838,-51.5021873498801,-34.4718016882636));
#28874=CARTESIAN_POINT('Ctrl Pts',(22.6587477517086,-48.6753895231782,-34.3138531650711));
#28875=CARTESIAN_POINT('Ctrl Pts',(20.344280622717,-47.0495757296036,-34.1559046418787));
#28876=CARTESIAN_POINT('Ctrl Pts',(17.7176647239296,-48.0988218888997,-33.9979561186862));
#28877=CARTESIAN_POINT('Ctrl Pts',(17.1603728058656,-50.8718084198119,-33.8400075954937));
#28878=CARTESIAN_POINT('Ctrl Pts',(19.1776845013661,-52.8543527713352,-33.6820590723013));
#28879=CARTESIAN_POINT('Ctrl Pts',(21.9405646498826,-52.2489422763042,-33.5241105491088));
#28880=CARTESIAN_POINT('Ctrl Pts',(22.9439938499564,-49.6044842178357,-33.3661620259164));
#28881=CARTESIAN_POINT('Ctrl Pts',(21.2781933638003,-47.3186282899868,-33.2082135027238));
#28882=CARTESIAN_POINT('Ctrl Pts',(18.4534938291803,-47.4638905413727,-33.0502649795314));
#28883=CARTESIAN_POINT('Ctrl Pts',(17.0309644047835,-49.9085661066135,-32.8923164563389));
#28884=CARTESIAN_POINT('Ctrl Pts',(18.3003692554337,-52.4361420021517,-32.7343679331465));
#28885=CARTESIAN_POINT('Ctrl Pts',(21.1107776102498,-52.7549420362487,-32.576419409954));
#28886=CARTESIAN_POINT('Ctrl Pts',(22.9140776886262,-50.5759199138536,-32.4184708867615));
#28887=CARTESIAN_POINT('Ctrl Pts',(22.0752721543919,-47.8747287213798,-32.260522363569));
#28888=CARTESIAN_POINT('Ctrl Pts',(19.3548804743199,-47.1004563600269,-32.1025738403766));
#28889=CARTESIAN_POINT('Ctrl Pts',(17.2193990477586,-48.9551120314041,-31.9446253171841));
#28890=CARTESIAN_POINT('Ctrl Pts',(17.6050039364394,-51.7571358450762,-31.7866767939917));
#28891=CARTESIAN_POINT('Ctrl Pts',(20.162078915438,-52.9660180288887,-31.6287282707991));
#28892=CARTESIAN_POINT('Ctrl Pts',(22.5722018712164,-51.4857018732685,-31.4707797476068));
#28893=CARTESIAN_POINT('Ctrl Pts',(22.6501876203464,-48.6583450147357,-31.3128312244142));
#28894=CARTESIAN_POINT('Ctrl Pts',(20.3253288559214,-47.0474259267501,-31.1548827012218));
#28895=CARTESIAN_POINT('Ctrl Pts',(17.7055043122623,-48.1135159524991,-30.9969341780293));
#28896=CARTESIAN_POINT('Ctrl Pts',(17.1660292247431,-50.8900236892983,-30.8389856548368));
#28897=CARTESIAN_POINT('Ctrl Pts',(19.1960292478244,-52.8595740158577,-30.6810371316444));
#28898=CARTESIAN_POINT('Ctrl Pts',(21.9549651002382,-52.2364355522512,-30.5230886084519));
#28899=CARTESIAN_POINT('Ctrl Pts',(22.9413935538417,-49.5855889915311,-30.3651400852594));
#28900=CARTESIAN_POINT('Ctrl Pts',(21.2609499306183,-47.310476288449,-30.207191562067));
#28901=CARTESIAN_POINT('Ctrl Pts',(18.4372413553613,-47.4738729364634,-30.0492430388745));
#28902=CARTESIAN_POINT('Ctrl Pts',(17.0304385140436,-49.9276321643062,-29.8912945156821));
#28903=CARTESIAN_POINT('Ctrl Pts',(18.3160467569104,-52.4470051078016,-29.7333459924895));
#28904=CARTESIAN_POINT('Ctrl Pts',(21.128444190168,-52.7477529423549,-29.5753974692971));
#28905=CARTESIAN_POINT('Ctrl Pts',(22.9177155962706,-50.5571967531925,-29.4174489461046));
#28906=CARTESIAN_POINT('Ctrl Pts',(22.0615830095597,-47.8614472143047,-29.2595004229122));
#28907=CARTESIAN_POINT('Ctrl Pts',(19.3362758082611,-47.1046584450221,-29.1015518997197));
#28908=CARTESIAN_POINT('Ctrl Pts',(17.2127471454189,-48.9729878058884,-28.9436033765272));
#28909=CARTESIAN_POINT('Ctrl Pts',(17.6163358752312,-51.7724778878259,-28.7856548533347));
#28910=CARTESIAN_POINT('Ctrl Pts',(20.181120371364,-52.9649161766797,-28.6277063301423));
#28911=CARTESIAN_POINT('Ctrl Pts',(22.5816885347909,-51.4691551413309,-28.4697578069498));
#28912=CARTESIAN_POINT('Ctrl Pts',(22.6415182232601,-48.6413558229776,-28.3118092837573));
#28913=CARTESIAN_POINT('Ctrl Pts',(20.3063636747943,-47.045397856035,-28.1538607605649));
#28914=CARTESIAN_POINT('Ctrl Pts',(17.6934385041046,-48.1282877980411,-27.9959122373724));
#28915=CARTESIAN_POINT('Ctrl Pts',(17.1718024827192,-50.9082022577011,-27.8379637141799));
#28916=CARTESIAN_POINT('Ctrl Pts',(19.2144071506939,-52.8646773725511,-27.6800151909875));
#28917=CARTESIAN_POINT('Ctrl Pts',(21.969284930193,-52.2238365980696,-27.522066667795));
#28918=CARTESIAN_POINT('Ctrl Pts',(22.9386720207179,-49.5667108964077,-27.3641181446025));
#28919=CARTESIAN_POINT('Ctrl Pts',(21.2436544380323,-47.3024350851045,-27.2061696214101));
#28920=CARTESIAN_POINT('Ctrl Pts',(18.4210534546561,-47.4839596618936,-27.0482210982176));
#28921=CARTESIAN_POINT('Ctrl Pts',(17.0300347762909,-49.9467008492878,-26.8902725750251));
#28922=CARTESIAN_POINT('Ctrl Pts',(18.3317942465966,-52.4577680338926,-26.7323240518326));
#28923=CARTESIAN_POINT('Ctrl Pts',(21.146063130971,-52.7404491468214,-26.5743755286402));
#28924=CARTESIAN_POINT('Ctrl Pts',(22.9212354249696,-50.5384534322301,-26.4164270054477));
#28925=CARTESIAN_POINT('Ctrl Pts',(22.0478044516093,-47.8482482790349,-26.2584784822553));
#28926=CARTESIAN_POINT('Ctrl Pts',(19.3177072968886,-47.1089910531324,-26.1005299590628));
#28927=CARTESIAN_POINT('Ctrl Pts',(17.2061926609974,-48.9908837262921,-25.9425814358703));
#28928=CARTESIAN_POINT('Ctrl Pts',(17.6278009322015,-51.7877910457717,-25.7846329126779));
#28929=CARTESIAN_POINT('Ctrl Pts',(20.2000849941159,-52.9636040941318,-25.6266843894854));
#28930=CARTESIAN_POINT('Ctrl Pts',(22.5912068609734,-51.4527230224798,-25.4687358662929));
#28931=CARTESIAN_POINT('Ctrl Pts',(22.63246493662,-48.6240737732433,-25.3107873431004));
#28932=CARTESIAN_POINT('Ctrl Pts',(20.2879336158885,-47.044187324869,-25.152838819908));
#28933=CARTESIAN_POINT('Ctrl Pts',(17.6803736923545,-48.1417371056711,-24.9948902967155));
#28934=CARTESIAN_POINT('Ctrl Pts',(17.1799177684998,-50.9293032433429,-24.836941773523));
#28935=CARTESIAN_POINT('Ctrl Pts',(18.5452496035378,-52.2169963426693,-24.7316427580614));
#28936=CARTESIAN_POINT('Ctrl Pts',(19.3498000020249,-52.4320868020351,-24.6789932503306));
#28937=CARTESIAN_POINT('Ctrl Pts',(17.9456684496579,-48.2435746787731,-40.1070022498898));
#28938=CARTESIAN_POINT('Ctrl Pts',(17.3646313374449,-48.9231611417519,-40.054352742159));
#28939=CARTESIAN_POINT('Ctrl Pts',(16.9397257481012,-50.8927896162339,-39.9490537266974));
#28940=CARTESIAN_POINT('Ctrl Pts',(19.0777499741398,-53.0547982657246,-39.7911052035049));
#28941=CARTESIAN_POINT('Ctrl Pts',(22.0523084692446,-52.4401119538419,-39.6331566803124));
#28942=CARTESIAN_POINT('Ctrl Pts',(23.1658860740626,-49.6164672289135,-39.4752081571199));
#28943=CARTESIAN_POINT('Ctrl Pts',(21.4091622878053,-47.1388520397903,-39.3172596339275));
#28944=CARTESIAN_POINT('Ctrl Pts',(18.3747378057433,-47.2562099103462,-39.159311110735));
#28945=CARTESIAN_POINT('Ctrl Pts',(16.8139173254206,-49.8608482964249,-39.0013625875425));
#28946=CARTESIAN_POINT('Ctrl Pts',(18.1418069399974,-52.5918675304547,-38.8434140643501));
#28947=CARTESIAN_POINT('Ctrl Pts',(21.1544708029442,-52.9728106959128,-38.6854655411576));
#28948=CARTESIAN_POINT('Ctrl Pts',(23.1204075266815,-50.6584513677779,-38.5275170179651));
#28949=CARTESIAN_POINT('Ctrl Pts',(22.2571674439236,-47.7470668110575,-38.3695684947727));
#28950=CARTESIAN_POINT('Ctrl Pts',(19.3474213868002,-46.878362018873,-38.2116199715802));
#28951=CARTESIAN_POINT('Ctrl Pts',(17.0293489638371,-48.8399445315482,-38.0536714483877));
#28952=CARTESIAN_POINT('Ctrl Pts',(17.4046752596388,-51.8533175278514,-37.8957229251952));
#28953=CARTESIAN_POINT('Ctrl Pts',(20.133103678538,-53.1863421439208,-37.7377744020028));
#28954=CARTESIAN_POINT('Ctrl Pts',(22.7408509828893,-51.6304081221977,-37.5798258788103));
#28955=CARTESIAN_POINT('Ctrl Pts',(22.8635520890914,-48.5962322027645,-37.4218773556178));
#28956=CARTESIAN_POINT('Ctrl Pts',(20.3899575926377,-46.8348100723855,-37.2639288324254));
#28957=CARTESIAN_POINT('Ctrl Pts',(17.5628004142346,-47.9431692734875,-37.1059803092329));
#28958=CARTESIAN_POINT('Ctrl Pts',(16.9453779725182,-50.9163943943856,-36.9480317860404));
#28959=CARTESIAN_POINT('Ctrl Pts',(19.0974884228245,-53.0587525607701,-36.790083262848));
#28960=CARTESIAN_POINT('Ctrl Pts',(22.0678786705856,-52.4278328221218,-36.6321347396554));
#28961=CARTESIAN_POINT('Ctrl Pts',(23.1633862198763,-49.5956708957895,-36.4741862164631));
#28962=CARTESIAN_POINT('Ctrl Pts',(21.3907476934156,-47.1301018746788,-36.3162376932706));
#28963=CARTESIAN_POINT('Ctrl Pts',(18.3571605311308,-47.266582198009,-36.1582891700781));
#28964=CARTESIAN_POINT('Ctrl Pts',(16.8130859505072,-49.881369310155,-36.0003406468856));
#28965=CARTESIAN_POINT('Ctrl Pts',(18.1584894129788,-52.6037152603445,-35.8423921236932));
#28966=CARTESIAN_POINT('Ctrl Pts',(21.1735345176749,-52.9653517726256,-35.6844436005007));
#28967=CARTESIAN_POINT('Ctrl Pts',(23.1245715666416,-50.6383940196509,-35.5264950773083));
#28968=CARTESIAN_POINT('Ctrl Pts',(22.2426546056792,-47.7326238249923,-35.3685465541157));
#28969=CARTESIAN_POINT('Ctrl Pts',(19.3273909210059,-46.8826146490553,-35.2105980309233));
#28970=CARTESIAN_POINT('Ctrl Pts',(17.0219614317752,-48.8590439598447,-35.0526495077308));
#28971=CARTESIAN_POINT('Ctrl Pts',(17.4166289394056,-51.8699434116262,-34.8947009845384));
#28972=CARTESIAN_POINT('Ctrl Pts',(20.1535604179975,-53.1854220438481,-34.7367524613459));
#28973=CARTESIAN_POINT('Ctrl Pts',(22.7512633359202,-51.6127753891431,-34.5788039381534));
#28974=CARTESIAN_POINT('Ctrl Pts',(22.8544794630559,-48.5778743394492,-34.420855414961));
#28975=CARTESIAN_POINT('Ctrl Pts',(20.3696258761073,-46.8323713741795,-34.2629068917684));
#28976=CARTESIAN_POINT('Ctrl Pts',(17.5496437489551,-47.9588609448717,-34.104958368576));
#28977=CARTESIAN_POINT('Ctrl Pts',(16.9513251104087,-50.9359892184104,-33.9470098453835));
#28978=CARTESIAN_POINT('Ctrl Pts',(19.1171472729993,-53.0644845344418,-33.7890613221911));
#28979=CARTESIAN_POINT('Ctrl Pts',(22.0834251524095,-52.4145049251787,-33.6311127989986));
#28980=CARTESIAN_POINT('Ctrl Pts',(23.1607248106417,-49.575367134104,-33.4731642758061));
#28981=CARTESIAN_POINT('Ctrl Pts',(21.3722914121648,-47.1212310479123,-33.3152157526137));
#28982=CARTESIAN_POINT('Ctrl Pts',(18.3396431266347,-47.2771872167786,-33.1572672294212));
#28983=CARTESIAN_POINT('Ctrl Pts',(16.8123899207133,-49.9018349255842,-32.9993187062287));
#28984=CARTESIAN_POINT('Ctrl Pts',(18.1752458269029,-52.6154859218069,-32.8413701830363));
#28985=CARTESIAN_POINT('Ctrl Pts',(21.1925508444502,-52.9577553791357,-32.6834216598438));
#28986=CARTESIAN_POINT('Ctrl Pts',(23.1286062811288,-50.6183179902657,-32.5254731366514));
#28987=CARTESIAN_POINT('Ctrl Pts',(22.2280495549668,-47.7182704849133,-32.3675246134588));
#28988=CARTESIAN_POINT('Ctrl Pts',(19.3073880603804,-46.8869977352239,-32.2095760902664));
#28989=CARTESIAN_POINT('Ctrl Pts',(17.0146967466071,-48.8781894613227,-32.0516275670739));
#28990=CARTESIAN_POINT('Ctrl Pts',(17.428689098791,-51.8864926845151,-31.8936790438815));
#28991=CARTESIAN_POINT('Ctrl Pts',(20.1740108422151,-53.184370365739,-31.735730520689));
#28992=CARTESIAN_POINT('Ctrl Pts',(22.7615622473033,-51.5950762845941,-31.5777819974966));
#28993=CARTESIAN_POINT('Ctrl Pts',(22.8452891518807,-48.55957504826,-31.419833474304));
#28994=CARTESIAN_POINT('Ctrl Pts',(20.3492789180058,-46.830063307124,-31.2618849511116));
#28995=CARTESIAN_POINT('Ctrl Pts',(17.5365881120131,-47.9746367561522,-31.1039364279191));
#28996=CARTESIAN_POINT('Ctrl Pts',(16.9573979435723,-50.9555454597386,-30.9459879047267));
#28997=CARTESIAN_POINT('Ctrl Pts',(19.1368425231359,-53.0700901565815,-30.7880393815342));
#28998=CARTESIAN_POINT('Ctrl Pts',(22.0988857352243,-52.4010774810233,-30.6300908583417));
#28999=CARTESIAN_POINT('Ctrl Pts',(23.1579330859087,-49.5550808788918,-30.4721423351492));
#29000=CARTESIAN_POINT('Ctrl Pts',(21.3537785517932,-47.1124789122659,-30.3141938119568));
#29001=CARTESIAN_POINT('Ctrl Pts',(18.3221941780797,-47.2879044959038,-30.1562452887643));
#29002=CARTESIAN_POINT('Ctrl Pts',(16.811825314945,-49.922304588451,-29.9982967655719));
#29003=CARTESIAN_POINT('Ctrl Pts',(18.1920774747975,-52.6271487476477,-29.8403482423793));
#29004=CARTESIAN_POINT('Ctrl Pts',(21.2115180027775,-52.9500370384753,-29.6823997191869));
#29005=CARTESIAN_POINT('Ctrl Pts',(23.1325120042847,-50.5982164678267,-29.5244511959944));
#29006=CARTESIAN_POINT('Ctrl Pts',(22.2133526425706,-47.7040112197537,-29.366502672802));
#29007=CARTESIAN_POINT('Ctrl Pts',(19.2874137558802,-46.8915091693428,-29.2085541496095));
#29008=CARTESIAN_POINT('Ctrl Pts',(17.0075551444725,-48.8973812147032,-29.050605626417));
#29009=CARTESIAN_POINT('Ctrl Pts',(17.4408552723353,-51.9029641778798,-28.8926571032246));
#29010=CARTESIAN_POINT('Ctrl Pts',(20.194454092182,-53.183187397366,-28.7347085800321));
#29011=CARTESIAN_POINT('Ctrl Pts',(22.7717473001459,-51.5773114152244,-28.5767600568396));
#29012=CARTESIAN_POINT('Ctrl Pts',(22.8359815310565,-48.5413351460594,-28.4188115336471));
#29013=CARTESIAN_POINT('Ctrl Pts',(20.3289175580364,-46.8278859338841,-28.2608630104547));
#29014=CARTESIAN_POINT('Ctrl Pts',(17.5236340431025,-47.9904960755269,-28.1029144872622));
#29015=CARTESIAN_POINT('Ctrl Pts',(16.9635962172961,-50.9750622981224,-27.9449659640698));
#29016=CARTESIAN_POINT('Ctrl Pts',(19.1565733705927,-53.0755692122251,-27.7870174408773));
#29017=CARTESIAN_POINT('Ctrl Pts',(22.1142597625249,-52.3875510169411,-27.6290689176848));
#29018=CARTESIAN_POINT('Ctrl Pts',(23.1550111989396,-49.534813016024,-27.4711203944923));
#29019=CARTESIAN_POINT('Ctrl Pts',(21.335209799508,-47.1038457315552,-27.3131718712999));
#29020=CARTESIAN_POINT('Ctrl Pts',(18.3048145563825,-47.29873378596,-27.1552233481074));
#29021=CARTESIAN_POINT('Ctrl Pts',(16.8113918548235,-49.9427770720226,-26.997274824915));
#29022=CARTESIAN_POINT('Ctrl Pts',(18.208984263294,-52.63870401891,-26.8393263017224));
#29023=CARTESIAN_POINT('Ctrl Pts',(21.2304340148929,-52.9421955520691,-26.68137777853));
#29024=CARTESIAN_POINT('Ctrl Pts',(23.1362909557585,-50.5780933009252,-26.5234292553375));
#29025=CARTESIAN_POINT('Ctrl Pts',(22.1985597346407,-47.6898406051712,-26.3654807321451));
#29026=CARTESIAN_POINT('Ctrl Pts',(19.2674782677023,-46.8961607354285,-26.2075322089526));
#29027=CARTESIAN_POINT('Ctrl Pts',(17.0005181319692,-48.9165945971056,-26.0495836857601));
#29028=CARTESIAN_POINT('Ctrl Pts',(17.4531643639531,-51.9194046599987,-25.8916351625677));
#29029=CARTESIAN_POINT('Ctrl Pts',(20.2148148526698,-53.1817787219156,-25.7336866393752));
#29030=CARTESIAN_POINT('Ctrl Pts',(22.7819663465347,-51.5596695965279,-25.5757381161827));
#29031=CARTESIAN_POINT('Ctrl Pts',(22.8262617594946,-48.522780826262,-25.4177895929903));
#29032=CARTESIAN_POINT('Ctrl Pts',(20.3091307149198,-46.8265862858259,-25.2598410697978));
#29033=CARTESIAN_POINT('Ctrl Pts',(17.5096074259459,-48.0049354943838,-25.1018925466053));
#29034=CARTESIAN_POINT('Ctrl Pts',(16.9723089342444,-50.9977166962789,-24.9439440234128));
#29035=CARTESIAN_POINT('Ctrl Pts',(18.438153778257,-52.3802071955689,-24.8386450079512));
#29036=CARTESIAN_POINT('Ctrl Pts',(19.301933573839,-52.6111321859386,-24.7859955002204));
#29037=CARTESIAN_POINT('Ctrl Pts',(17.8048028959809,-48.1231365609212,-40.2140044997796));
#29038=CARTESIAN_POINT('Ctrl Pts',(17.1839240578764,-48.8493222806572,-40.1613549920488));
#29039=CARTESIAN_POINT('Ctrl Pts',(16.7298826841491,-50.9540082172854,-40.0560559765871));
#29040=CARTESIAN_POINT('Ctrl Pts',(19.014511272237,-53.2642658412,-39.8981074533947));
#29041=CARTESIAN_POINT('Ctrl Pts',(22.1930353002121,-52.6074304771614,-39.7401589302022));
#29042=CARTESIAN_POINT('Ctrl Pts',(23.3829709426793,-49.5901683794686,-39.5822104070097));
#29043=CARTESIAN_POINT('Ctrl Pts',(21.5057885728173,-46.9426630694658,-39.4242618838173));
#29044=CARTESIAN_POINT('Ctrl Pts',(18.2632935460151,-47.068068171449,-39.2663133606248));
#29045=CARTESIAN_POINT('Ctrl Pts',(16.5954475755204,-49.8513066614508,-39.1083648374323));
#29046=CARTESIAN_POINT('Ctrl Pts',(18.0143906063523,-52.7695919365634,-38.9504163142399));
#29047=CARTESIAN_POINT('Ctrl Pts',(21.2336328879706,-53.176656382159,-38.7924677910474));
#29048=CARTESIAN_POINT('Ctrl Pts',(23.334373930435,-50.7036013906531,-38.6345192678549));
#29049=CARTESIAN_POINT('Ctrl Pts',(22.4119414587009,-47.5925831392253,-38.4765707446625));
#29050=CARTESIAN_POINT('Ctrl Pts',(19.3026740588186,-46.6643112428346,-38.31862222147));
#29051=CARTESIAN_POINT('Ctrl Pts',(16.8256513655012,-48.7603995059013,-38.1606736982775));
#29052=CARTESIAN_POINT('Ctrl Pts',(17.2267137925807,-51.9803995461637,-38.002725175085));
#29053=CARTESIAN_POINT('Ctrl Pts',(20.1422306003197,-53.4048296856387,-37.8447766518926));
#29054=CARTESIAN_POINT('Ctrl Pts',(22.9287911871795,-51.7422052383032,-37.6868281287001));
#29055=CARTESIAN_POINT('Ctrl Pts',(23.0599059105793,-48.499975818074,-37.5288796055077));
#29056=CARTESIAN_POINT('Ctrl Pts',(20.4166969922192,-46.6177729385439,-37.3709310823152));
#29057=CARTESIAN_POINT('Ctrl Pts',(17.3956815920498,-47.8021323512527,-37.2129825591227));
#29058=CARTESIAN_POINT('Ctrl Pts',(16.7359224817024,-50.9792315755262,-37.0550340359303));
#29059=CARTESIAN_POINT('Ctrl Pts',(19.0356031867254,-53.2684912823324,-36.8970855127378));
#29060=CARTESIAN_POINT('Ctrl Pts',(22.2096731505566,-52.5943093651446,-36.7391369895453));
#29061=CARTESIAN_POINT('Ctrl Pts',(23.3802996734437,-49.5679460413847,-36.5811884663528));
#29062=CARTESIAN_POINT('Ctrl Pts',(21.4861112893383,-46.9333129053653,-36.4232399431604));
#29063=CARTESIAN_POINT('Ctrl Pts',(18.2445109973463,-47.0791516870751,-36.2652914199679));
#29064=CARTESIAN_POINT('Ctrl Pts',(16.5945591932132,-49.8732348014845,-36.1073428967754));
#29065=CARTESIAN_POINT('Ctrl Pts',(18.0322169968249,-52.7822520655183,-35.949394373583));
#29066=CARTESIAN_POINT('Ctrl Pts',(21.2540038019849,-53.1686860003594,-35.7914458503905));
#29067=CARTESIAN_POINT('Ctrl Pts',(23.3388234986948,-50.6821687097818,-35.633497327198));
#29068=CARTESIAN_POINT('Ctrl Pts',(22.3964334748606,-47.5771497973294,-35.4755488040056));
#29069=CARTESIAN_POINT('Ctrl Pts',(19.2812701036018,-46.6688554759499,-35.3176002808131));
#29070=CARTESIAN_POINT('Ctrl Pts',(16.8177572702246,-48.780808582361,-35.1596517576206));
#29071=CARTESIAN_POINT('Ctrl Pts',(17.2394871363976,-51.9981654671068,-35.0017032344282));
#29072=CARTESIAN_POINT('Ctrl Pts',(20.1640900587951,-53.4038464942864,-34.8437547112357));
#29073=CARTESIAN_POINT('Ctrl Pts',(22.9399175154567,-51.723363428406,-34.6858061880432));
#29074=CARTESIAN_POINT('Ctrl Pts',(23.0502111744031,-48.4803591557203,-34.5278576648508));
#29075=CARTESIAN_POINT('Ctrl Pts',(20.3949711294977,-46.6151670187554,-34.3699091416583));
#29076=CARTESIAN_POINT('Ctrl Pts',(17.3816227739805,-47.8189000008437,-34.2119606184658));
#29077=CARTESIAN_POINT('Ctrl Pts',(16.7422774149517,-51.000170017009,-34.0540120952733));
#29078=CARTESIAN_POINT('Ctrl Pts',(19.0566100446325,-53.2746162975484,-33.8960635720809));
#29079=CARTESIAN_POINT('Ctrl Pts',(22.2262856549365,-52.5800675740533,-33.7381150488884));
#29080=CARTESIAN_POINT('Ctrl Pts',(23.377455771327,-49.5462500503724,-33.5801665256959));
#29081=CARTESIAN_POINT('Ctrl Pts',(21.4663894605293,-46.9238338058378,-33.4222180025035));
#29082=CARTESIAN_POINT('Ctrl Pts',(18.2257924240891,-47.0904838921846,-33.264269479311));
#29083=CARTESIAN_POINT('Ctrl Pts',(16.5938154366431,-49.8951037445551,-33.1063209561186));
#29084=CARTESIAN_POINT('Ctrl Pts',(18.0501223983721,-52.7948298414622,-32.9483724329261));
#29085=CARTESIAN_POINT('Ctrl Pts',(21.2743240786507,-53.1605687220227,-32.7904239097336));
#29086=CARTESIAN_POINT('Ctrl Pts',(23.3431348736315,-50.6607160666778,-32.6324753865412));
#29087=CARTESIAN_POINT('Ctrl Pts',(22.3808269555417,-47.5618122484469,-32.4745268633486));
#29088=CARTESIAN_POINT('Ctrl Pts',(19.2598956464409,-46.6735391104208,-32.3165783401562));
#29089=CARTESIAN_POINT('Ctrl Pts',(16.8099944454557,-48.8012668912414,-32.1586298169637));
#29090=CARTESIAN_POINT('Ctrl Pts',(17.2523742611426,-52.015849523954,-32.0006812937713));
#29091=CARTESIAN_POINT('Ctrl Pts',(20.1859427689921,-53.4027227025893,-31.8427327705787));
#29092=CARTESIAN_POINT('Ctrl Pts',(22.9509226233902,-51.7044506959199,-31.6847842473864));
#29093=CARTESIAN_POINT('Ctrl Pts',(23.040390683415,-48.4608050817844,-31.5268357241939));
#29094=CARTESIAN_POINT('Ctrl Pts',(20.3732289800902,-46.6127006874977,-31.3688872010014));
#29095=CARTESIAN_POINT('Ctrl Pts',(17.3676719117639,-47.8357575598052,-31.2109386778089));
#29096=CARTESIAN_POINT('Ctrl Pts',(16.7487666624015,-51.0210672301788,-31.0529901546165));
#29097=CARTESIAN_POINT('Ctrl Pts',(19.0776557984475,-53.2806062973054,-30.895041631424));
#29098=CARTESIAN_POINT('Ctrl Pts',(22.2428063702104,-52.5657194097955,-30.7370931082315));
#29099=CARTESIAN_POINT('Ctrl Pts',(23.3744726179757,-49.5245727662524,-30.579144585039));
#29100=CARTESIAN_POINT('Ctrl Pts',(21.4466071729682,-46.9144815360828,-30.4211960618466));
#29101=CARTESIAN_POINT('Ctrl Pts',(18.2071470007981,-47.1019360553443,-30.2632475386541));
#29102=CARTESIAN_POINT('Ctrl Pts',(16.5932121158465,-49.9169770125958,-30.1052990154617));
#29103=CARTESIAN_POINT('Ctrl Pts',(18.0681081926846,-52.8072923874939,-29.9473504922691));
#29104=CARTESIAN_POINT('Ctrl Pts',(21.2945918153871,-53.1523211345956,-29.7894019690767));
#29105=CARTESIAN_POINT('Ctrl Pts',(23.3473084122988,-50.639236182461,-29.6314534458842));
#29106=CARTESIAN_POINT('Ctrl Pts',(22.3651222755816,-47.5465752252027,-29.4735049226918));
#29107=CARTESIAN_POINT('Ctrl Pts',(19.2385517034993,-46.6783598936636,-29.3155563994993));
#29108=CARTESIAN_POINT('Ctrl Pts',(16.8023631435262,-48.821774623518,-29.1576078763068));
#29109=CARTESIAN_POINT('Ctrl Pts',(17.2653746694394,-52.0334504679336,-28.9996593531144));
#29110=CARTESIAN_POINT('Ctrl Pts',(20.2077878130001,-53.4014586180524,-28.8417108299219));
#29111=CARTESIAN_POINT('Ctrl Pts',(22.9618060655009,-51.6854676891177,-28.6837623067294));
#29112=CARTESIAN_POINT('Ctrl Pts',(23.030444838853,-48.4413144691413,-28.5258137835369));
#29113=CARTESIAN_POINT('Ctrl Pts',(20.3514714412784,-46.6103740117332,-28.3678652603445));
#29114=CARTESIAN_POINT('Ctrl Pts',(17.3538295821005,-47.8527043530126,-28.209916737152));
#29115=CARTESIAN_POINT('Ctrl Pts',(16.755389951873,-51.0419223385436,-28.0519682139596));
#29116=CARTESIAN_POINT('Ctrl Pts',(19.0987395904915,-53.2864610518992,-27.8940196907671));
#29117=CARTESIAN_POINT('Ctrl Pts',(22.259234594857,-52.5512654358125,-27.7360711675746));
#29118=CARTESIAN_POINT('Ctrl Pts',(23.3713503771613,-49.5029151356404,-27.5781226443821));
#29119=CARTESIAN_POINT('Ctrl Pts',(21.4267651609838,-46.9052563780058,-27.4201741211897));
#29120=CARTESIAN_POINT('Ctrl Pts',(18.1885756581089,-47.1135079100266,-27.2622255979972));
#29121=CARTESIAN_POINT('Ctrl Pts',(16.5927489333562,-49.9388532947573,-27.1042770748048));
#29122=CARTESIAN_POINT('Ctrl Pts',(18.0861742799915,-52.8196400039275,-26.9463285516122));
#29123=CARTESIAN_POINT('Ctrl Pts',(21.3148048988148,-53.1439419573167,-26.7883800284198));
#29124=CARTESIAN_POINT('Ctrl Pts',(23.3513464865473,-50.6177331696203,-26.6304315052273));
#29125=CARTESIAN_POINT('Ctrl Pts',(22.3493150176721,-47.5314329313073,-26.4724829820349));
#29126=CARTESIAN_POINT('Ctrl Pts',(19.2172492385159,-46.6833304177247,-26.3145344588424));
#29127=CARTESIAN_POINT('Ctrl Pts',(16.794843602941,-48.8423054679189,-26.1565859356499));
#29128=CARTESIAN_POINT('Ctrl Pts',(17.2785277957047,-52.0510182742257,-25.9986374124575));
#29129=CARTESIAN_POINT('Ctrl Pts',(20.2295447112238,-53.3999533496994,-25.840688889265));
#29130=CARTESIAN_POINT('Ctrl Pts',(22.9727258320959,-51.6666161705761,-25.6827403660725));
#29131=CARTESIAN_POINT('Ctrl Pts',(23.0200585823692,-48.4214878792807,-25.52479184288));
#29132=CARTESIAN_POINT('Ctrl Pts',(20.3303278139511,-46.6089852467828,-25.3668433196876));
#29133=CARTESIAN_POINT('Ctrl Pts',(17.3388411595373,-47.8681338830967,-25.2088947964951));
#29134=CARTESIAN_POINT('Ctrl Pts',(16.764700099989,-51.0661301492147,-25.0509462733027));
#29135=CARTESIAN_POINT('Ctrl Pts',(18.3310579529763,-52.5434180484685,-24.945647257841));
#29136=CARTESIAN_POINT('Ctrl Pts',(19.2540671456531,-52.7901775698422,-24.8929977501102));
#29137=CARTESIAN_POINT('Ctrl Pts',(17.6639373423039,-48.0026984430693,-40.3210067496694));
#29138=CARTESIAN_POINT('Ctrl Pts',(17.003216778308,-48.7754834195626,-40.2683572419386));
#29139=CARTESIAN_POINT('Ctrl Pts',(16.520039620197,-51.0152268183369,-40.163058226477));
#29140=CARTESIAN_POINT('Ctrl Pts',(18.9512725703343,-53.4737334166756,-40.0051097032844));
#29141=CARTESIAN_POINT('Ctrl Pts',(22.3337621311796,-52.7747490004808,-39.8471611800921));
#29142=CARTESIAN_POINT('Ctrl Pts',(23.600055811296,-49.5638695300238,-39.6892126568995));
#29143=CARTESIAN_POINT('Ctrl Pts',(21.6024148578293,-46.7464740991412,-39.5312641337071));
#29144=CARTESIAN_POINT('Ctrl Pts',(18.1518492862868,-46.8799264325519,-39.3733156105146));
#29145=CARTESIAN_POINT('Ctrl Pts',(16.3769778256201,-49.8417650264767,-39.2153670873222));
#29146=CARTESIAN_POINT('Ctrl Pts',(17.8869742727072,-52.9473163426722,-39.0574185641297));
#29147=CARTESIAN_POINT('Ctrl Pts',(21.3127949729971,-53.3805020684052,-38.8994700409372));
#29148=CARTESIAN_POINT('Ctrl Pts',(23.5483403341885,-50.7487514135285,-38.7415215177447));
#29149=CARTESIAN_POINT('Ctrl Pts',(22.5667154734781,-47.438099467393,-38.5835729945523));
#29150=CARTESIAN_POINT('Ctrl Pts',(19.257926730837,-46.4502604667964,-38.4256244713598));
#29151=CARTESIAN_POINT('Ctrl Pts',(16.6219537671653,-48.6808544802542,-38.2676759481673));
#29152=CARTESIAN_POINT('Ctrl Pts',(17.0487523255225,-52.107481564476,-38.1097274249749));
#29153=CARTESIAN_POINT('Ctrl Pts',(20.1513575221015,-53.6233172273567,-37.9517789017824));
#29154=CARTESIAN_POINT('Ctrl Pts',(23.1167313914696,-51.8540023544087,-37.7938303785899));
#29155=CARTESIAN_POINT('Ctrl Pts',(23.2562597320672,-48.4037194333835,-37.6358818553975));
#29156=CARTESIAN_POINT('Ctrl Pts',(20.4434363918007,-46.4007358047025,-37.477933332205));
#29157=CARTESIAN_POINT('Ctrl Pts',(17.228562769865,-47.6610954290179,-37.3199848090125));
#29158=CARTESIAN_POINT('Ctrl Pts',(16.5264669908866,-51.0420687566668,-37.1620362858201));
#29159=CARTESIAN_POINT('Ctrl Pts',(18.9737179506262,-53.4782300038948,-37.0040877626276));
#29160=CARTESIAN_POINT('Ctrl Pts',(22.3514676305278,-52.7607859081673,-36.8461392394351));
#29161=CARTESIAN_POINT('Ctrl Pts',(23.5972131270111,-49.5402211869799,-36.6881907162427));
#29162=CARTESIAN_POINT('Ctrl Pts',(21.581474885261,-46.7365239360518,-36.5302421930502));
#29163=CARTESIAN_POINT('Ctrl Pts',(18.1318614635619,-46.8917211761413,-36.3722936698578));
#29164=CARTESIAN_POINT('Ctrl Pts',(16.3760324359193,-49.8651002928142,-36.2143451466652));
#29165=CARTESIAN_POINT('Ctrl Pts',(17.905944580671,-52.960788870692,-36.0563966234728));
#29166=CARTESIAN_POINT('Ctrl Pts',(21.3344730862948,-53.3720202280932,-35.8984481002803));
#29167=CARTESIAN_POINT('Ctrl Pts',(23.5530754307479,-50.7259433999127,-35.7404995770879));
#29168=CARTESIAN_POINT('Ctrl Pts',(22.550212344042,-47.4216757696665,-35.5825510538954));
#29169=CARTESIAN_POINT('Ctrl Pts',(19.2351492861978,-46.4550963028444,-35.4246025307029));
#29170=CARTESIAN_POINT('Ctrl Pts',(16.613553108674,-48.7025732048773,-35.2666540075104));
#29171=CARTESIAN_POINT('Ctrl Pts',(17.0623453333896,-52.1263875225874,-35.108705484318));
#29172=CARTESIAN_POINT('Ctrl Pts',(20.1746196995926,-53.6222709447248,-34.9507569611255));
#29173=CARTESIAN_POINT('Ctrl Pts',(23.1285716949932,-51.833951467669,-34.792808437933));
#29174=CARTESIAN_POINT('Ctrl Pts',(23.2459428857504,-48.3828439719913,-34.6348599147406));
#29175=CARTESIAN_POINT('Ctrl Pts',(20.420316382888,-46.3979626633313,-34.4769113915481));
#29176=CARTESIAN_POINT('Ctrl Pts',(17.213601799006,-47.6789390568155,-34.3189628683557));
#29177=CARTESIAN_POINT('Ctrl Pts',(16.5332297194947,-51.0643508156075,-34.1610143451632));
#29178=CARTESIAN_POINT('Ctrl Pts',(18.9960728162657,-53.4847480606549,-34.0030658219707));
#29179=CARTESIAN_POINT('Ctrl Pts',(22.3691461574634,-52.7456302229279,-33.8451172987783));
#29180=CARTESIAN_POINT('Ctrl Pts',(23.5941867320123,-49.5171329666407,-33.6871687755858));
#29181=CARTESIAN_POINT('Ctrl Pts',(21.5604875088938,-46.7264365637634,-33.5292202523933));
#29182=CARTESIAN_POINT('Ctrl Pts',(18.1119417215434,-46.9037805675905,-33.3712717292008));
#29183=CARTESIAN_POINT('Ctrl Pts',(16.3752409525729,-49.8883725635259,-33.2133232060083));
#29184=CARTESIAN_POINT('Ctrl Pts',(17.9249989698413,-52.9741737611174,-33.0553746828159));
#29185=CARTESIAN_POINT('Ctrl Pts',(21.3560973128511,-53.3633820649098,-32.8974261596234));
#29186=CARTESIAN_POINT('Ctrl Pts',(23.5576634661342,-50.7031141430899,-32.7394776364309));
#29187=CARTESIAN_POINT('Ctrl Pts',(22.5336043561166,-47.4053540119805,-32.5815291132385));
#29188=CARTESIAN_POINT('Ctrl Pts',(19.2124032325014,-46.4600804856177,-32.4235805900461));
#29189=CARTESIAN_POINT('Ctrl Pts',(16.6052921443043,-48.7243443211601,-32.2656320668535));
#29190=CARTESIAN_POINT('Ctrl Pts',(17.0760594234942,-52.145206363393,-32.1076835436611));
#29191=CARTESIAN_POINT('Ctrl Pts',(20.1978746957691,-53.6210750394396,-31.9497350204685));
#29192=CARTESIAN_POINT('Ctrl Pts',(23.1402829994771,-51.8138251072455,-31.7917864972762));
#29193=CARTESIAN_POINT('Ctrl Pts',(23.2354922149493,-48.3620351153088,-31.6338379740836));
#29194=CARTESIAN_POINT('Ctrl Pts',(20.3971790421746,-46.3953380678715,-31.4758894508912));
#29195=CARTESIAN_POINT('Ctrl Pts',(17.1987557115146,-47.6968783634582,-31.3179409276987));
#29196=CARTESIAN_POINT('Ctrl Pts',(16.5401353812306,-51.0865890006191,-31.1599924045063));
#29197=CARTESIAN_POINT('Ctrl Pts',(19.018469073759,-53.4911224380292,-31.0020438813138));
#29198=CARTESIAN_POINT('Ctrl Pts',(22.3867270051965,-52.7303613385677,-30.8440953581213));
#29199=CARTESIAN_POINT('Ctrl Pts',(23.5910121500427,-49.494064653613,-30.6861468349289));
#29200=CARTESIAN_POINT('Ctrl Pts',(21.5394357941431,-46.7164841598999,-30.5281983117364));
#29201=CARTESIAN_POINT('Ctrl Pts',(18.0920998235166,-46.9159676147846,-30.3702497885439));
#29202=CARTESIAN_POINT('Ctrl Pts',(16.3745989167479,-49.9116494367408,-30.2123012653515));
#29203=CARTESIAN_POINT('Ctrl Pts',(17.9441389105717,-52.98743602734,-30.054352742159));
#29204=CARTESIAN_POINT('Ctrl Pts',(21.3776656279966,-53.354605230716,-29.8964042189665));
#29205=CARTESIAN_POINT('Ctrl Pts',(23.5621048203129,-50.6802558970953,-29.738455695774));
#29206=CARTESIAN_POINT('Ctrl Pts',(22.5168919085926,-47.3891392306516,-29.5805071725816));
#29207=CARTESIAN_POINT('Ctrl Pts',(19.1896896511183,-46.4652106179844,-29.4225586493891));
#29208=CARTESIAN_POINT('Ctrl Pts',(16.5971711425799,-48.7461680323328,-29.2646101261967));
#29209=CARTESIAN_POINT('Ctrl Pts',(17.0898940665435,-52.1639367579875,-29.1066616030041));
#29210=CARTESIAN_POINT('Ctrl Pts',(20.2211215338182,-53.6197298387387,-28.9487130798117));
#29211=CARTESIAN_POINT('Ctrl Pts',(23.1518648308559,-51.7936239630112,-28.7907645566192));
#29212=CARTESIAN_POINT('Ctrl Pts',(23.2249081466494,-48.341293792223,-28.6328160334268));
#29213=CARTESIAN_POINT('Ctrl Pts',(20.3740253245205,-46.3928620895824,-28.4748675102343));
#29214=CARTESIAN_POINT('Ctrl Pts',(17.1840251210985,-47.7149126304983,-28.3169189870418));
#29215=CARTESIAN_POINT('Ctrl Pts',(16.5471836864498,-51.1087823789649,-28.1589704638494));
#29216=CARTESIAN_POINT('Ctrl Pts',(19.0409058103903,-53.4973528915733,-28.0010219406569));
#29217=CARTESIAN_POINT('Ctrl Pts',(22.4042094271889,-52.714979854684,-27.8430734174644));
#29218=CARTESIAN_POINT('Ctrl Pts',(23.587689555383,-49.4710172552568,-27.685124894272));
#29219=CARTESIAN_POINT('Ctrl Pts',(21.5183205224596,-46.7066670244563,-27.5271763710795));
#29220=CARTESIAN_POINT('Ctrl Pts',(18.0723367598354,-46.9282820340933,-27.369227847887));
#29221=CARTESIAN_POINT('Ctrl Pts',(16.3741060118888,-49.934929517492,-27.2112793246946));
#29222=CARTESIAN_POINT('Ctrl Pts',(17.963364296689,-53.000575988945,-27.053330801502));
#29223=CARTESIAN_POINT('Ctrl Pts',(21.3991757827366,-53.3456883625643,-26.8953822783096));
#29224=CARTESIAN_POINT('Ctrl Pts',(23.5664020173362,-50.6573730383154,-26.7374337551172));
#29225=CARTESIAN_POINT('Ctrl Pts',(22.5000703007035,-47.3730252574435,-26.5794852319247));
#29226=CARTESIAN_POINT('Ctrl Pts',(19.1670202093295,-46.4705001000209,-26.4215367087323));
#29227=CARTESIAN_POINT('Ctrl Pts',(16.5891690739128,-48.7680163387323,-26.2635881855397));
#29228=CARTESIAN_POINT('Ctrl Pts',(17.1038912274563,-52.1826318884526,-26.1056396623473));
#29229=CARTESIAN_POINT('Ctrl Pts',(20.2442745697777,-53.6181279774832,-25.9476911391548));
#29230=CARTESIAN_POINT('Ctrl Pts',(23.1634853176571,-51.7735627446242,-25.7897426159623));
#29231=CARTESIAN_POINT('Ctrl Pts',(23.2138554052439,-48.3201949322993,-25.6317940927699));
#29232=CARTESIAN_POINT('Ctrl Pts',(20.3515249129824,-46.3913842077397,-25.4738455695774));
#29233=CARTESIAN_POINT('Ctrl Pts',(17.1680748931287,-47.7313322718094,-25.315897046385));
#29234=CARTESIAN_POINT('Ctrl Pts',(16.5570912657335,-51.1345436021507,-25.1579485231925));
#29235=CARTESIAN_POINT('Ctrl Pts',(18.2239621276955,-52.7066289013681,-25.0526495077308));
#29236=CARTESIAN_POINT('Ctrl Pts',(19.2062007174672,-52.9692229537457,-25.));
#29237=CARTESIAN_POINT('Ctrl Pts',(22.5181182812424,-50.0021988905331,-38.387416697508));
#29238=CARTESIAN_POINT('Ctrl Pts',(22.5197006098244,-50.176561944423,-38.3984493876971));
#29239=CARTESIAN_POINT('Ctrl Pts',(22.5031153273103,-50.3506259111307,-38.4094820778862));
#29240=CARTESIAN_POINT('Ctrl Pts',(22.4672444397961,-50.5206201453611,-38.4205147680753));
#29241=CARTESIAN_POINT('Ctrl Pts',(22.2960636545913,-51.3318558998239,-38.4731642758061));
#29242=CARTESIAN_POINT('Ctrl Pts',(21.6856861862545,-52.0504104547452,-38.525813783537));
#29243=CARTESIAN_POINT('Ctrl Pts',(20.9128165447069,-52.3505507513191,-38.5784632912678));
#29244=CARTESIAN_POINT('Ctrl Pts',(20.1399469031593,-52.650691047893,-38.6311127989986));
#29245=CARTESIAN_POINT('Ctrl Pts',(19.2045850884009,-52.5324170861195,-38.6837623067294));
#29246=CARTESIAN_POINT('Ctrl Pts',(18.5307648146348,-52.0493212397415,-38.7364118144603));
#29247=CARTESIAN_POINT('Ctrl Pts',(17.8569445408687,-51.5662253933636,-38.7890613221911));
#29248=CARTESIAN_POINT('Ctrl Pts',(17.4446658080948,-50.7183076623813,-38.8417108299219));
#29249=CARTESIAN_POINT('Ctrl Pts',(17.4808256067329,-49.8900090831976,-38.8943603376527));
#29250=CARTESIAN_POINT('Ctrl Pts',(17.5169854053711,-49.0617105040138,-38.9470098453835));
#29251=CARTESIAN_POINT('Ctrl Pts',(18.0015837354214,-48.2530310766285,-38.9996593531144));
#29252=CARTESIAN_POINT('Ctrl Pts',(18.7149418900001,-47.8304729230812,-39.0523088608452));
#29253=CARTESIAN_POINT('Ctrl Pts',(19.4283000445789,-47.4079147695338,-39.104958368576));
#29254=CARTESIAN_POINT('Ctrl Pts',(20.3704180236861,-47.3714778898244,-39.1576078763068));
#29255=CARTESIAN_POINT('Ctrl Pts',(21.1141878803485,-47.7378802946769,-39.2102573840377));
#29256=CARTESIAN_POINT('Ctrl Pts',(21.8579577370108,-48.1042826995294,-39.2629068917685));
#29257=CARTESIAN_POINT('Ctrl Pts',(22.4033794712283,-48.8735243889439,-39.3155563994993));
#29258=CARTESIAN_POINT('Ctrl Pts',(22.5032204104756,-49.6964831256785,-39.3682059072301));
#29259=CARTESIAN_POINT('Ctrl Pts',(22.5153637550683,-49.7965770510867,-39.3746095039894));
#29260=CARTESIAN_POINT('Ctrl Pts',(22.5209155764383,-49.8974656183845,-39.3810131007487));
#29261=CARTESIAN_POINT('Ctrl Pts',(22.5201577888434,-49.9984351914864,-39.387416697508));
#29262=CARTESIAN_POINT('Ctrl Pts',(20.7937992825328,-52.9692229537457,-40.));
#29263=CARTESIAN_POINT('Ctrl Pts',(21.7760378723045,-52.7066289013681,-39.9473504922692));
#29264=CARTESIAN_POINT('Ctrl Pts',(23.4429086391268,-51.1345429997358,-39.8420514768075));
#29265=CARTESIAN_POINT('Ctrl Pts',(22.831925189682,-47.7313325290799,-39.6841029536151));
#29266=CARTESIAN_POINT('Ctrl Pts',(19.6484750771286,-46.3913839963408,-39.5261544304226));
#29267=CARTESIAN_POINT('Ctrl Pts',(16.7861445447059,-48.3201950030769,-39.3682059072301));
#29268=CARTESIAN_POINT('Ctrl Pts',(16.8365146481096,-51.7735627154933,-39.2102573840377));
#29269=CARTESIAN_POINT('Ctrl Pts',(19.7557254203512,-53.6181280557829,-39.0523088608451));
#29270=CARTESIAN_POINT('Ctrl Pts',(22.8961088159911,-52.1826319013229,-38.8943603376528));
#29271=CARTESIAN_POINT('Ctrl Pts',(23.4108309690293,-48.7680163312232,-38.7364118144603));
#29272=CARTESIAN_POINT('Ctrl Pts',(20.8329798036235,-46.4705000476597,-38.5784632912678));
#29273=CARTESIAN_POINT('Ctrl Pts',(17.4999296646635,-47.373025224819,-38.4205147680753));
#29274=CARTESIAN_POINT('Ctrl Pts',(16.4335979353407,-50.6573730457065,-38.2625662448828));
#29275=CARTESIAN_POINT('Ctrl Pts',(18.600824198122,-53.3456884082951,-38.1046177216904));
#29276=CARTESIAN_POINT('Ctrl Pts',(22.0366357308683,-53.0005760288509,-37.9466691984979));
#29277=CARTESIAN_POINT('Ctrl Pts',(23.6258940367278,-49.9349295168378,-37.7887206753055));
#29278=CARTESIAN_POINT('Ctrl Pts',(21.9276632661251,-46.9282819927009,-37.630772152113));
#29279=CARTESIAN_POINT('Ctrl Pts',(18.4816794571067,-46.7066669802649,-37.4728236289205));
#29280=CARTESIAN_POINT('Ctrl Pts',(16.4123103964255,-49.471017248116,-37.314875105728));
#29281=CARTESIAN_POINT('Ctrl Pts',(17.5957905404958,-52.7149798911831,-37.1569265825356));
#29282=CARTESIAN_POINT('Ctrl Pts',(20.9590942025022,-53.497352938559,-36.9989780593431));
#29283=CARTESIAN_POINT('Ctrl Pts',(23.4528163599439,-51.1087823938688,-36.8410295361506));
#29284=CARTESIAN_POINT('Ctrl Pts',(22.815974916742,-47.7149125997905,-36.6830810129582));
#29285=CARTESIAN_POINT('Ctrl Pts',(19.625974670453,-46.3928620411136,-36.5251324897657));
#29286=CARTESIAN_POINT('Ctrl Pts',(16.775091810017,-48.3412937699339,-36.3671839665732));
#29287=CARTESIAN_POINT('Ctrl Pts',(16.8481351267915,-51.7936239871129,-36.2092354433808));
#29288=CARTESIAN_POINT('Ctrl Pts',(19.7788784632106,-53.6197298873777,-36.0512869201883));
#29289=CARTESIAN_POINT('Ctrl Pts',(22.9101059725603,-52.163936787065,-35.8933383969958));
#29290=CARTESIAN_POINT('Ctrl Pts',(23.4028289031449,-48.7461680154847,-35.7353898738033));
#29291=CARTESIAN_POINT('Ctrl Pts',(20.81031035977,-46.4652105704865,-35.5774413506109));
#29292=CARTESIAN_POINT('Ctrl Pts',(17.4831080575873,-47.3891391955688,-35.4194928274184));
#29293=CARTESIAN_POINT('Ctrl Pts',(16.4378951318222,-50.6802559062359,-35.261544304226));
#29294=CARTESIAN_POINT('Ctrl Pts',(18.6223343534913,-53.3546052757928,-35.1035957810335));
#29295=CARTESIAN_POINT('Ctrl Pts',(22.0558611170534,-52.9874360674829,-34.945647257841));
#29296=CARTESIAN_POINT('Ctrl Pts',(23.6254011319675,-49.9116494355537,-34.7876987346486));
#29297=CARTESIAN_POINT('Ctrl Pts',(21.9079002021205,-46.9159675733437,-34.6297502114561));
#29298=CARTESIAN_POINT('Ctrl Pts',(18.4605641851711,-46.7164841157783,-34.4718016882636));
#29299=CARTESIAN_POINT('Ctrl Pts',(16.4089878017039,-49.4940646468145,-34.3138531650711));
#29300=CARTESIAN_POINT('Ctrl Pts',(17.6132729627324,-52.7303613752562,-34.1559046418787));
#29301=CARTESIAN_POINT('Ctrl Pts',(20.98153093943,-53.4911224849404,-33.9979561186862));
#29302=CARTESIAN_POINT('Ctrl Pts',(23.4598646652605,-51.08658901522,-33.8400075954937));
#29303=CARTESIAN_POINT('Ctrl Pts',(22.8012443261265,-47.6968783325106,-33.6820590723013));
#29304=CARTESIAN_POINT('Ctrl Pts',(19.6028209524885,-46.3953380194348,-33.5241105491088));
#29305=CARTESIAN_POINT('Ctrl Pts',(16.7645077415746,-48.362035093299,-33.3661620259164));
#29306=CARTESIAN_POINT('Ctrl Pts',(16.8597169583261,-51.8138251316183,-33.2082135027239));
#29307=CARTESIAN_POINT('Ctrl Pts',(19.8021253015719,-53.621075088097,-33.0502649795314));
#29308=CARTESIAN_POINT('Ctrl Pts',(22.9239406157955,-52.1452063922187,-32.8923164563389));
#29309=CARTESIAN_POINT('Ctrl Pts',(23.3947079013113,-48.7243443040189,-32.7343679331465));
#29310=CARTESIAN_POINT('Ctrl Pts',(20.7875967780819,-46.4600804380509,-32.576419409954));
#29311=CARTESIAN_POINT('Ctrl Pts',(17.4663956098388,-47.4053539771154,-32.4184708867615));
#29312=CARTESIAN_POINT('Ctrl Pts',(16.4423364860605,-50.7031141525378,-32.2605223635691));
#29313=CARTESIAN_POINT('Ctrl Pts',(18.6439026689266,-53.3633821101044,-32.1025738403766));
#29314=CARTESIAN_POINT('Ctrl Pts',(22.0750010580409,-52.9741738010823,-31.9446253171841));
#29315=CARTESIAN_POINT('Ctrl Pts',(23.624759096134,-49.888372562026,-31.7866767939916));
#29316=CARTESIAN_POINT('Ctrl Pts',(21.888058303827,-46.9037805259858,-31.6287282707992));
#29317=CARTESIAN_POINT('Ctrl Pts',(18.4395124701376,-46.7264365197756,-31.4707797476067));
#29318=CARTESIAN_POINT('Ctrl Pts',(16.4058132196916,-49.5171329601522,-31.3128312244143));
#29319=CARTESIAN_POINT('Ctrl Pts',(17.6308538107017,-52.7456302598216,-31.1548827012217));
#29320=CARTESIAN_POINT('Ctrl Pts',(21.0039271972243,-53.4847481074805,-30.9969341780293));
#29321=CARTESIAN_POINT('Ctrl Pts',(23.4667703270891,-51.0643508299095,-30.8389856548368));
#29322=CARTESIAN_POINT('Ctrl Pts',(22.7863982384356,-47.6789390256271,-30.6810371316444));
#29323=CARTESIAN_POINT('Ctrl Pts',(19.5796836114642,-46.3979626149297,-30.5230886084519));
#29324=CARTESIAN_POINT('Ctrl Pts',(16.7540570706331,-48.3828439502611,-30.3651400852594));
#29325=CARTESIAN_POINT('Ctrl Pts',(16.8714282629673,-51.8339514923121,-30.207191562067));
#29326=CARTESIAN_POINT('Ctrl Pts',(19.8253802980609,-53.6222709933982,-30.0492430388745));
#29327=CARTESIAN_POINT('Ctrl Pts',(22.9376547060844,-52.1263875511603,-29.891294515682));
#29328=CARTESIAN_POINT('Ctrl Pts',(23.3864469368306,-48.7025731874435,-29.7333459924896));
#29329=CARTESIAN_POINT('Ctrl Pts',(20.7648507240798,-46.4550962552107,-29.5753974692971));
#29330=CARTESIAN_POINT('Ctrl Pts',(17.4497876216902,-47.4216757350208,-29.4174489461046));
#29331=CARTESIAN_POINT('Ctrl Pts',(16.4469245215085,-50.7259434096673,-29.2595004229122));
#29332=CARTESIAN_POINT('Ctrl Pts',(18.6655268957734,-53.3720202734039,-29.1015518997197));
#29333=CARTESIAN_POINT('Ctrl Pts',(22.0940554474673,-52.960788910477,-28.9436033765272));
#29334=CARTESIAN_POINT('Ctrl Pts',(23.6239676127769,-49.8651002910015,-28.7856548533348));
#29335=CARTESIAN_POINT('Ctrl Pts',(21.8681385615409,-46.8917211343748,-28.6277063301423));
#29336=CARTESIAN_POINT('Ctrl Pts',(18.4185250934885,-46.7365238921992,-28.4697578069498));
#29337=CARTESIAN_POINT('Ctrl Pts',(16.4027868246521,-49.5402211808024,-28.3118092837573));
#29338=CARTESIAN_POINT('Ctrl Pts',(17.648532337875,-52.7607859452632,-28.1538607605649));
#29339=CARTESIAN_POINT('Ctrl Pts',(21.0262820631638,-53.4782300506355,-27.9959122373724));
#29340=CARTESIAN_POINT('Ctrl Pts',(23.4735330557886,-51.042068770664,-27.8379637141799));
#29341=CARTESIAN_POINT('Ctrl Pts',(22.7714372673746,-47.6610953975998,-27.6800151909874));
#29342=CARTESIAN_POINT('Ctrl Pts',(19.556563602243,-46.4007357563187,-27.522066667795));
#29343=CARTESIAN_POINT('Ctrl Pts',(16.7437402241732,-48.4037194119704,-27.3641181446025));
#29344=CARTESIAN_POINT('Ctrl Pts',(16.883268566659,-51.8540023792524,-27.2061696214101));
#29345=CARTESIAN_POINT('Ctrl Pts',(19.8486424758461,-53.6233172761733,-27.0482210982176));
#29346=CARTESIAN_POINT('Ctrl Pts',(22.9512477141718,-52.1074815925537,-26.8902725750252));
#29347=CARTESIAN_POINT('Ctrl Pts',(23.3780462781492,-48.6808544629774,-26.7323240518326));
#29348=CARTESIAN_POINT('Ctrl Pts',(20.7420732792926,-46.4502604182672,-26.5743755286402));
#29349=CARTESIAN_POINT('Ctrl Pts',(17.4332844917096,-47.4380994344961,-26.4164270054477));
#29350=CARTESIAN_POINT('Ctrl Pts',(16.4516596187905,-50.7487514207967,-26.2584784822553));
#29351=CARTESIAN_POINT('Ctrl Pts',(18.6872050080179,-53.3805021188932,-26.1005299590628));
#29352=CARTESIAN_POINT('Ctrl Pts',(22.1130257584277,-52.9473163731849,-25.9425814358703));
#29353=CARTESIAN_POINT('Ctrl Pts',(23.6230222174753,-49.8417650404807,-25.7846329126778));
#29354=CARTESIAN_POINT('Ctrl Pts',(21.8481507499307,-46.8799263624337,-25.6266843894854));
#29355=CARTESIAN_POINT('Ctrl Pts',(18.3975850974581,-46.7464741037567,-25.4687358662929));
#29356=CARTESIAN_POINT('Ctrl Pts',(16.3999441875489,-49.5638694433452,-25.3107873431005));
#29357=CARTESIAN_POINT('Ctrl Pts',(17.6662377409256,-52.7747491690934,-25.152838819908));
#29358=CARTESIAN_POINT('Ctrl Pts',(21.0487276436386,-53.4737332515659,-24.9948902967155));
#29359=CARTESIAN_POINT('Ctrl Pts',(23.4799599601655,-51.0152272608972,-24.836941773523));
#29360=CARTESIAN_POINT('Ctrl Pts',(22.996783221692,-48.7754834195627,-24.7316427580614));
#29361=CARTESIAN_POINT('Ctrl Pts',(22.3360626576962,-48.0026984430694,-24.6789932503306));
#29362=CARTESIAN_POINT('Ctrl Pts',(20.7459328543469,-52.7901775698422,-40.1070022498898));
#29363=CARTESIAN_POINT('Ctrl Pts',(21.6689420470237,-52.5434180484685,-40.054352742159));
#29364=CARTESIAN_POINT('Ctrl Pts',(23.2352998106083,-51.0661295831258,-39.9490537266973));
#29365=CARTESIAN_POINT('Ctrl Pts',(22.6611589182799,-47.8681341248537,-39.7911052035049));
#29366=CARTESIAN_POINT('Ctrl Pts',(19.6696721767562,-46.6089850481313,-39.6331566803124));
#29367=CARTESIAN_POINT('Ctrl Pts',(16.9799413705986,-48.4214879457904,-39.4752081571199));
#29368=CARTESIAN_POINT('Ctrl Pts',(17.0272741357351,-51.6666161432018,-39.3172596339275));
#29369=CARTESIAN_POINT('Ctrl Pts',(19.7704552795004,-53.3999534232776,-39.159311110735));
#29370=CARTESIAN_POINT('Ctrl Pts',(22.7214722451228,-52.0510182863199,-39.0013625875425));
#29371=CARTESIAN_POINT('Ctrl Pts',(23.2051564374117,-48.8423054608625,-38.84341406435));
#29372=CARTESIAN_POINT('Ctrl Pts',(20.7827507736561,-46.683330368521,-38.6854655411576));
#29373=CARTESIAN_POINT('Ctrl Pts',(17.6506849497833,-47.5314329006501,-38.5275170179651));
#29374=CARTESIAN_POINT('Ctrl Pts',(16.6486534689832,-50.6177331765657,-38.3695684947727));
#29375=CARTESIAN_POINT('Ctrl Pts',(18.6851950831981,-53.1439420002899,-38.2116199715802));
#29376=CARTESIAN_POINT('Ctrl Pts',(21.9138257459041,-52.8196400414271,-38.0536714483878));
#29377=CARTESIAN_POINT('Ctrl Pts',(23.4072511123288,-49.9388532941425,-37.8957229251952));
#29378=CARTESIAN_POINT('Ctrl Pts',(21.8114243662861,-47.1135078711303,-37.7377744020028));
#29379=CARTESIAN_POINT('Ctrl Pts',(18.5732348198147,-46.905256336479,-37.5798258788103));
#29380=CARTESIAN_POINT('Ctrl Pts',(16.6286495775531,-49.5029151289302,-37.4218773556178));
#29381=CARTESIAN_POINT('Ctrl Pts',(17.7407653747764,-52.5512654701108,-37.2639288324254));
#29382=CARTESIAN_POINT('Ctrl Pts',(20.9012604216236,-53.2864610960517,-37.1059803092329));
#29383=CARTESIAN_POINT('Ctrl Pts',(23.2446100917232,-51.0419223525488,-36.9480317860405));
#29384=CARTESIAN_POINT('Ctrl Pts',(22.6461704534581,-47.8527043241565,-36.790083262848));
#29385=CARTESIAN_POINT('Ctrl Pts',(19.6485285539981,-46.6103739661872,-36.6321347396555));
#29386=CARTESIAN_POINT('Ctrl Pts',(16.9695551204265,-48.4413144481962,-36.474186216463));
#29387=CARTESIAN_POINT('Ctrl Pts',(17.0381938947004,-51.6854677117661,-36.3162376932706));
#29388=CARTESIAN_POINT('Ctrl Pts',(19.7922121842078,-53.4014586637584,-36.1582891700781));
#29389=CARTESIAN_POINT('Ctrl Pts',(22.7346253673064,-52.0334504952578,-36.0003406468857));
#29390=CARTESIAN_POINT('Ctrl Pts',(23.1976368994413,-48.8217746076858,-35.8423921236931));
#29391=CARTESIAN_POINT('Ctrl Pts',(20.7614483067326,-46.67835984903,-35.6844436005007));
#29392=CARTESIAN_POINT('Ctrl Pts',(17.6348776926376,-47.5465751922353,-35.5264950773082));
#29393=CARTESIAN_POINT('Ctrl Pts',(16.6526915427226,-50.6392361910505,-35.3685465541158));
#29394=CARTESIAN_POINT('Ctrl Pts',(18.7054081672171,-53.1523211769542,-35.2105980309233));
#29395=CARTESIAN_POINT('Ctrl Pts',(21.9318918332747,-52.8072924252161,-35.0526495077308));
#29396=CARTESIAN_POINT('Ctrl Pts',(23.4067879299314,-49.9169770114804,-34.8947009845384));
#29397=CARTESIAN_POINT('Ctrl Pts',(21.7928530232929,-47.1019360164021,-34.7367524613459));
#29398=CARTESIAN_POINT('Ctrl Pts',(18.5533928075934,-46.9144814946219,-34.5788039381534));
#29399=CARTESIAN_POINT('Ctrl Pts',(16.6255273366806,-49.5245727598638,-34.420855414961));
#29400=CARTESIAN_POINT('Ctrl Pts',(17.7571935996524,-52.5657194442717,-34.2629068917685));
#29401=CARTESIAN_POINT('Ctrl Pts',(20.9223442139462,-53.2806063413878,-34.104958368576));
#29402=CARTESIAN_POINT('Ctrl Pts',(23.2512333812862,-51.0210672438993,-33.9470098453835));
#29403=CARTESIAN_POINT('Ctrl Pts',(22.6323281236075,-47.8357575307237,-33.7890613221911));
#29404=CARTESIAN_POINT('Ctrl Pts',(19.6267710148948,-46.6127006419817,-33.6311127989986));
#29405=CARTESIAN_POINT('Ctrl Pts',(16.9596092757305,-48.4608050611018,-33.4731642758062));
#29406=CARTESIAN_POINT('Ctrl Pts',(17.0490773369575,-51.7044507188229,-33.3152157526136));
#29407=CARTESIAN_POINT('Ctrl Pts',(19.8140572285093,-53.4027227483126,-33.1572672294212));
#29408=CARTESIAN_POINT('Ctrl Pts',(22.7476257757779,-52.0158495510415,-32.9993187062287));
#29409=CARTESIAN_POINT('Ctrl Pts',(23.1900055974093,-48.8012668751339,-32.8413701830363));
#29410=CARTESIAN_POINT('Ctrl Pts',(20.7401043635042,-46.6735390657223,-32.6834216598438));
#29411=CARTESIAN_POINT('Ctrl Pts',(17.6191730124666,-47.5618122156842,-32.5254731366514));
#29412=CARTESIAN_POINT('Ctrl Pts',(16.6568650814459,-50.6607160755559,-32.3675246134588));
#29413=CARTESIAN_POINT('Ctrl Pts',(18.7256759042258,-53.1605687644921,-32.2095760902664));
#29414=CARTESIAN_POINT('Ctrl Pts',(21.9498776278288,-52.7948298790171,-32.0516275670739));
#29415=CARTESIAN_POINT('Ctrl Pts',(23.4061846091267,-49.8951037431457,-31.8936790438815));
#29416=CARTESIAN_POINT('Ctrl Pts',(21.7742075997515,-47.0904838530887,-31.735730520689));
#29417=CARTESIAN_POINT('Ctrl Pts',(18.5336105197666,-46.9238337645025,-31.5777819974966));
#29418=CARTESIAN_POINT('Ctrl Pts',(16.6225441832892,-49.5462500442751,-31.419833474304));
#29419=CARTESIAN_POINT('Ctrl Pts',(17.7737143151483,-52.5800676087223,-31.2618849511116));
#29420=CARTESIAN_POINT('Ctrl Pts',(20.943389968044,-53.2746163415502,-31.1039364279191));
#29421=CARTESIAN_POINT('Ctrl Pts',(23.2577226288231,-51.0001700304486,-30.9459879047267));
#29422=CARTESIAN_POINT('Ctrl Pts',(22.6183772612034,-47.8188999715357,-30.7880393815342));
#29423=CARTESIAN_POINT('Ctrl Pts',(19.6050288651951,-46.6151669732725,-30.6300908583417));
#29424=CARTESIAN_POINT('Ctrl Pts',(16.9497887846104,-48.4803591353003,-30.4721423351492));
#29425=CARTESIAN_POINT('Ctrl Pts',(17.0600824450388,-51.7233634515632,-30.3141938119568));
#29426=CARTESIAN_POINT('Ctrl Pts',(19.8359099389999,-53.4038465400247,-30.1562452887643));
#29427=CARTESIAN_POINT('Ctrl Pts',(22.7605129006961,-51.9981654939569,-29.9982967655718));
#29428=CARTESIAN_POINT('Ctrl Pts',(23.1822427725361,-48.7808085659784,-29.8403482423793));
#29429=CARTESIAN_POINT('Ctrl Pts',(20.718729906056,-46.6688554311885,-29.6823997191869));
#29430=CARTESIAN_POINT('Ctrl Pts',(17.603566492938,-47.5771497647728,-29.5244511959944));
#29431=CARTESIAN_POINT('Ctrl Pts',(16.6611764564406,-50.6821687189482,-29.366502672802));
#29432=CARTESIAN_POINT('Ctrl Pts',(18.7459961811647,-53.1686860429378,-29.2085541496095));
#29433=CARTESIAN_POINT('Ctrl Pts',(21.9677830296167,-52.7822521029042,-29.050605626417));
#29434=CARTESIAN_POINT('Ctrl Pts',(23.4054408525466,-49.8732347997812,-28.8926571032246));
#29435=CARTESIAN_POINT('Ctrl Pts',(21.7554890262427,-47.0791516478272,-28.7347085800321));
#29436=CARTESIAN_POINT('Ctrl Pts',(18.5138886906926,-46.933312864157,-28.5767600568396));
#29437=CARTESIAN_POINT('Ctrl Pts',(16.6197002811342,-49.5679460355797,-28.4188115336471));
#29438=CARTESIAN_POINT('Ctrl Pts',(17.7903268197514,-52.5943094000035,-28.2608630104547));
#29439=CARTESIAN_POINT('Ctrl Pts',(20.9643968262331,-53.2684913262547,-28.1029144872623));
#29440=CARTESIAN_POINT('Ctrl Pts',(23.2640775621583,-50.9792315886794,-27.9449659640697));
#29441=CARTESIAN_POINT('Ctrl Pts',(22.6043184429442,-47.8021323217292,-27.7870174408773));
#29442=CARTESIAN_POINT('Ctrl Pts',(19.5833030021837,-46.6177728930778,-27.6290689176848));
#29443=CARTESIAN_POINT('Ctrl Pts',(16.9400940482998,-48.4999757979521,-27.4711203944923));
#29444=CARTESIAN_POINT('Ctrl Pts',(17.071208773474,-51.7422052616489,-27.3131718712999));
#29445=CARTESIAN_POINT('Ctrl Pts',(19.8577693977516,-53.4048297315116,-27.1552233481074));
#29446=CARTESIAN_POINT('Ctrl Pts',(22.7732862447201,-51.9803995725483,-26.997274824915));
#29447=CARTESIAN_POINT('Ctrl Pts',(23.1743486770808,-48.7603994896662,-26.8393263017224));
#29448=CARTESIAN_POINT('Ctrl Pts',(20.6973259507001,-46.6643111972318,-26.68137777853));
#29449=CARTESIAN_POINT('Ctrl Pts',(17.5880585085861,-47.5925831083121,-26.5234292553375));
#29450=CARTESIAN_POINT('Ctrl Pts',(16.6656260253793,-50.7036013974831,-26.3654807321451));
#29451=CARTESIAN_POINT('Ctrl Pts',(18.7663670941892,-53.1766564296025,-26.2075322089526));
#29452=CARTESIAN_POINT('Ctrl Pts',(21.9856094229051,-52.7695919652361,-26.0495836857601));
#29453=CARTESIAN_POINT('Ctrl Pts',(23.4045524649764,-49.8513066746105,-25.8916351625676));
#29454=CARTESIAN_POINT('Ctrl Pts',(21.7367064880185,-47.0680681055589,-25.7336866393752));
#29455=CARTESIAN_POINT('Ctrl Pts',(18.4942113851663,-46.942663073803,-25.5757381161827));
#29456=CARTESIAN_POINT('Ctrl Pts',(16.6170290562352,-49.5901682980168,-25.4177895929903));
#29457=CARTESIAN_POINT('Ctrl Pts',(17.8069645796052,-52.6074306356065,-25.2598410697978));
#29458=CARTESIAN_POINT('Ctrl Pts',(20.9854889288333,-53.2642656860466,-25.1018925466053));
#29459=CARTESIAN_POINT('Ctrl Pts',(23.2701169215177,-50.9540086331591,-24.9439440234129));
#29460=CARTESIAN_POINT('Ctrl Pts',(22.8160759421236,-48.8493222806574,-24.8386450079512));
#29461=CARTESIAN_POINT('Ctrl Pts',(22.1951971040192,-48.1231365609213,-24.7859955002204));
#29462=CARTESIAN_POINT('Ctrl Pts',(20.698066426161,-52.6111321859386,-40.2140044997796));
#29463=CARTESIAN_POINT('Ctrl Pts',(21.561846221743,-52.3802071955689,-40.1613549920488));
#29464=CARTESIAN_POINT('Ctrl Pts',(23.0276909820899,-50.9977161665157,-40.0560559765871));
#29465=CARTESIAN_POINT('Ctrl Pts',(22.4903926468778,-48.0049357206273,-39.8981074533947));
#29466=CARTESIAN_POINT('Ctrl Pts',(19.6908692763838,-46.8265860999219,-39.7401589302022));
#29467=CARTESIAN_POINT('Ctrl Pts',(17.1737381964913,-48.5227808885037,-39.5822104070097));
#29468=CARTESIAN_POINT('Ctrl Pts',(17.2180336233606,-51.5596695709103,-39.4242618838173));
#29469=CARTESIAN_POINT('Ctrl Pts',(19.7851851386495,-53.1817787907722,-39.2663133606248));
#29470=CARTESIAN_POINT('Ctrl Pts',(22.5468356742545,-51.9194046713169,-39.1083648374324));
#29471=CARTESIAN_POINT('Ctrl Pts',(22.9994819057941,-48.9165945905019,-38.9504163142399));
#29472=CARTESIAN_POINT('Ctrl Pts',(20.7325217436886,-46.8961606893823,-38.7924677910474));
#29473=CARTESIAN_POINT('Ctrl Pts',(17.8014402349031,-47.6898405764811,-38.634519267855));
#29474=CARTESIAN_POINT('Ctrl Pts',(16.8637090026257,-50.5780933074249,-38.4765707446625));
#29475=CARTESIAN_POINT('Ctrl Pts',(18.7695659682742,-52.9421955922846,-38.31862222147));
#29476=CARTESIAN_POINT('Ctrl Pts',(21.7910157609398,-52.6387040540034,-38.1606736982776));
#29477=CARTESIAN_POINT('Ctrl Pts',(23.1886081879298,-49.9427770714472,-38.002725175085));
#29478=CARTESIAN_POINT('Ctrl Pts',(21.6951854664471,-47.2987337495597,-37.8447766518926));
#29479=CARTESIAN_POINT('Ctrl Pts',(18.6647901825227,-47.1038456926932,-37.6868281287001));
#29480=CARTESIAN_POINT('Ctrl Pts',(16.8449887586807,-49.5348130097445,-37.5288796055077));
#29481=CARTESIAN_POINT('Ctrl Pts',(17.8857402090571,-52.3875510490384,-37.3709310823152));
#29482=CARTESIAN_POINT('Ctrl Pts',(20.8434266407449,-53.0755692535444,-37.2129825591227));
#29483=CARTESIAN_POINT('Ctrl Pts',(23.0364038235026,-50.9750623112288,-37.0550340359302));
#29484=CARTESIAN_POINT('Ctrl Pts',(22.4763659901743,-47.9904960485225,-36.8970855127378));
#29485=CARTESIAN_POINT('Ctrl Pts',(19.6710824375433,-46.8278858912607,-36.7391369895453));
#29486=CARTESIAN_POINT('Ctrl Pts',(17.164018430836,-48.5413351264584,-36.5811884663529));
#29487=CARTESIAN_POINT('Ctrl Pts',(17.2282526626093,-51.5773114364193,-36.4232399431604));
#29488=CARTESIAN_POINT('Ctrl Pts',(19.8055459052051,-53.1831874401391,-36.2652914199679));
#29489=CARTESIAN_POINT('Ctrl Pts',(22.5591447620525,-51.9029642034506,-36.1073428967754));
#29490=CARTESIAN_POINT('Ctrl Pts',(22.9924448957378,-48.897381199887,-35.949394373583));
#29491=CARTESIAN_POINT('Ctrl Pts',(20.7125862536951,-46.8915091275734,-35.7914458503905));
#29492=CARTESIAN_POINT('Ctrl Pts',(17.786647327688,-47.7040111889018,-35.633497327198));
#29493=CARTESIAN_POINT('Ctrl Pts',(16.8674879536229,-50.5982164758651,-35.4755488040056));
#29494=CARTESIAN_POINT('Ctrl Pts',(18.788481980943,-52.9500370781157,-35.3176002808131));
#29495=CARTESIAN_POINT('Ctrl Pts',(21.8079225494959,-52.6271487829494,-35.1596517576206));
#29496=CARTESIAN_POINT('Ctrl Pts',(23.1881747278953,-49.9223045874071,-35.0017032344282));
#29497=CARTESIAN_POINT('Ctrl Pts',(21.6778058444655,-47.2879044594606,-34.8437547112357));
#29498=CARTESIAN_POINT('Ctrl Pts',(18.6462214300157,-47.1124788734655,-34.6858061880432));
#29499=CARTESIAN_POINT('Ctrl Pts',(16.8420668716573,-49.5550808729132,-34.5278576648508));
#29500=CARTESIAN_POINT('Ctrl Pts',(17.9011142365724,-52.4010775132872,-34.3699091416583));
#29501=CARTESIAN_POINT('Ctrl Pts',(20.8631574884625,-53.0700901978351,-34.2119606184659));
#29502=CARTESIAN_POINT('Ctrl Pts',(23.0426020973119,-50.9555454725786,-34.0540120952733));
#29503=CARTESIAN_POINT('Ctrl Pts',(22.4634119210885,-47.9746367289368,-33.8960635720809));
#29504=CARTESIAN_POINT('Ctrl Pts',(19.650721077301,-46.8300632645287,-33.7381150488884));
#29505=CARTESIAN_POINT('Ctrl Pts',(17.1547108098864,-48.5595750289046,-33.580166525696));
#29506=CARTESIAN_POINT('Ctrl Pts',(17.2384377155889,-51.5950763060275,-33.4222180025035));
#29507=CARTESIAN_POINT('Ctrl Pts',(19.8259891554466,-53.1843704085283,-33.264269479311));
#29508=CARTESIAN_POINT('Ctrl Pts',(22.5713109357603,-51.8864927098645,-33.1063209561185));
#29509=CARTESIAN_POINT('Ctrl Pts',(22.9853032935072,-48.8781894462487,-32.9483724329261));
#29510=CARTESIAN_POINT('Ctrl Pts',(20.6926119489265,-46.8869976933937,-32.7904239097336));
#29511=CARTESIAN_POINT('Ctrl Pts',(17.7719504150944,-47.718270454253,-32.6324753865412));
#29512=CARTESIAN_POINT('Ctrl Pts',(16.8713936768312,-50.6183179985742,-32.4745268633487));
#29513=CARTESIAN_POINT('Ctrl Pts',(18.8074491395251,-52.9577554188798,-32.3165783401562));
#29514=CARTESIAN_POINT('Ctrl Pts',(21.8247541976167,-52.615485956952,-32.1586298169637));
#29515=CARTESIAN_POINT('Ctrl Pts',(23.1876101221194,-49.9018349242652,-32.0006812937713));
#29516=CARTESIAN_POINT('Ctrl Pts',(21.6603568956761,-47.2771871801915,-31.8427327705788));
#29517=CARTESIAN_POINT('Ctrl Pts',(18.6277085693955,-47.1212310092294,-31.6847842473863));
#29518=CARTESIAN_POINT('Ctrl Pts',(16.8392751468868,-49.575367128398,-31.5268357241939));
#29519=CARTESIAN_POINT('Ctrl Pts',(17.9165748195948,-52.414504957623,-31.3688872010014));
#29520=CARTESIAN_POINT('Ctrl Pts',(20.8828527388637,-53.0644845756201,-31.2109386778089));
#29521=CARTESIAN_POINT('Ctrl Pts',(23.0486749305571,-50.9359892309876,-31.0529901546165));
#29522=CARTESIAN_POINT('Ctrl Pts',(22.4503562839711,-47.9588609174444,-30.895041631424));
#29523=CARTESIAN_POINT('Ctrl Pts',(19.6303741189261,-46.8323713316152,-30.7370931082315));
#29524=CARTESIAN_POINT('Ctrl Pts',(17.1455204985878,-48.5778743203397,-30.579144585039));
#29525=CARTESIAN_POINT('Ctrl Pts',(17.2487366271103,-51.6127754108142,-30.4211960618466));
#29526=CARTESIAN_POINT('Ctrl Pts',(19.8464395799389,-53.1854220866514,-30.2632475386541));
#29527=CARTESIAN_POINT('Ctrl Pts',(22.5833710953078,-51.8699434367532,-30.1052990154617));
#29528=CARTESIAN_POINT('Ctrl Pts',(22.9780386082415,-48.8590439445134,-29.9473504922691));
#29529=CARTESIAN_POINT('Ctrl Pts',(20.6726090880323,-46.8826146071662,-29.7894019690767));
#29530=CARTESIAN_POINT('Ctrl Pts',(17.7573453641857,-47.7326237945248,-29.6314534458842));
#29531=CARTESIAN_POINT('Ctrl Pts',(16.8754283913727,-50.6383940282292,-29.4735049226918));
#29532=CARTESIAN_POINT('Ctrl Pts',(18.8264654665559,-52.9653518124717,-29.3155563994993));
#29533=CARTESIAN_POINT('Ctrl Pts',(21.8415106117661,-52.6037152953314,-29.1576078763068));
#29534=CARTESIAN_POINT('Ctrl Pts',(23.1869140923162,-49.8813693085608,-28.9996593531144));
#29535=CARTESIAN_POINT('Ctrl Pts',(21.6428394909445,-47.2665821612795,-28.8417108299219));
#29536=CARTESIAN_POINT('Ctrl Pts',(18.6092522878967,-47.1301018361149,-28.6837623067294));
#29537=CARTESIAN_POINT('Ctrl Pts',(16.8366137376164,-49.5956708903569,-28.525813783537));
#29538=CARTESIAN_POINT('Ctrl Pts',(17.9321213016278,-52.4278328547439,-28.3678652603445));
#29539=CARTESIAN_POINT('Ctrl Pts',(20.9025115893025,-53.0587526018739,-28.209916737152));
#29540=CARTESIAN_POINT('Ctrl Pts',(23.0546220685279,-50.9163944066948,-28.0519682139595));
#29541=CARTESIAN_POINT('Ctrl Pts',(22.4371996185138,-47.9431692458585,-27.8940196907671));
#29542=CARTESIAN_POINT('Ctrl Pts',(19.6100424021244,-46.8348100298369,-27.7360711675746));
#29543=CARTESIAN_POINT('Ctrl Pts',(17.1364478724265,-48.5962321839338,-27.5781226443822));
#29544=CARTESIAN_POINT('Ctrl Pts',(17.259148980289,-51.6304081440452,-27.4201741211897));
#29545=CARTESIAN_POINT('Ctrl Pts',(19.8668963196571,-53.1863421868501,-27.2622255979972));
#29546=CARTESIAN_POINT('Ctrl Pts',(22.5953247752684,-51.8533175525428,-27.1042770748048));
#29547=CARTESIAN_POINT('Ctrl Pts',(22.9706510760124,-48.8399445163551,-26.9463285516123));
#29548=CARTESIAN_POINT('Ctrl Pts',(20.6525786221077,-46.8783619761964,-26.7883800284198));
#29549=CARTESIAN_POINT('Ctrl Pts',(17.7428325254625,-47.747066782128,-26.6304315052274));
#29550=CARTESIAN_POINT('Ctrl Pts',(16.8795924319682,-50.6584513741695,-26.4724829820349));
#29551=CARTESIAN_POINT('Ctrl Pts',(18.8455291803604,-52.9728107403119,-26.3145344588424));
#29552=CARTESIAN_POINT('Ctrl Pts',(21.8581930873826,-52.5918675572875,-26.1565859356499));
#29553=CARTESIAN_POINT('Ctrl Pts',(23.1860827124775,-49.8608483087402,-25.9986374124575));
#29554=CARTESIAN_POINT('Ctrl Pts',(21.6252622261063,-47.2562098486842,-25.840688889265));
#29555=CARTESIAN_POINT('Ctrl Pts',(18.5908376728745,-47.1388520438493,-25.6827403660725));
#29556=CARTESIAN_POINT('Ctrl Pts',(16.8341139249216,-49.6164671526884,-25.5247918428801));
#29557=CARTESIAN_POINT('Ctrl Pts',(17.9476914182848,-52.4401121021197,-25.3668433196876));
#29558=CARTESIAN_POINT('Ctrl Pts',(20.9222502140279,-53.0547981205273,-25.2088947964951));
#29559=CARTESIAN_POINT('Ctrl Pts',(23.0602738828699,-50.892790005421,-25.0509462733027));
#29560=CARTESIAN_POINT('Ctrl Pts',(22.6353686625552,-48.923161141752,-24.945647257841));
#29561=CARTESIAN_POINT('Ctrl Pts',(22.0543315503421,-48.2435746787732,-24.8929977501102));
#29562=CARTESIAN_POINT('Ctrl Pts',(20.6501999979751,-52.4320868020351,-40.3210067496694));
#29563=CARTESIAN_POINT('Ctrl Pts',(21.4547503964622,-52.2169963426693,-40.2683572419386));
#29564=CARTESIAN_POINT('Ctrl Pts',(22.8200821535714,-50.9293027499057,-40.1630582264769));
#29565=CARTESIAN_POINT('Ctrl Pts',(22.3196263754757,-48.141737316401,-40.0051097032845));
#29566=CARTESIAN_POINT('Ctrl Pts',(19.7120663760114,-47.0441871517124,-39.847161180092));
#29567=CARTESIAN_POINT('Ctrl Pts',(17.367535022384,-48.6240738312172,-39.6892126568995));
#29568=CARTESIAN_POINT('Ctrl Pts',(17.4087931109861,-51.4527229986188,-39.5312641337071));
#29569=CARTESIAN_POINT('Ctrl Pts',(19.7999149977987,-52.9636041582669,-39.3733156105146));
#29570=CARTESIAN_POINT('Ctrl Pts',(22.3721991033862,-51.7877910563139,-39.2153670873222));
#29571=CARTESIAN_POINT('Ctrl Pts',(22.7938073741765,-48.9908837201412,-39.0574185641296));
#29572=CARTESIAN_POINT('Ctrl Pts',(20.6822927137212,-47.1089910102435,-38.8994700409372));
#29573=CARTESIAN_POINT('Ctrl Pts',(17.9521955200229,-47.8482482523122,-38.7415215177447));
#29574=CARTESIAN_POINT('Ctrl Pts',(17.0787645362682,-50.5384534382841,-38.5835729945523));
#29575=CARTESIAN_POINT('Ctrl Pts',(18.8539368533503,-52.7404491842795,-38.4256244713598));
#29576=CARTESIAN_POINT('Ctrl Pts',(21.6682057759756,-52.4577680665795,-38.2676759481674));
#29577=CARTESIAN_POINT('Ctrl Pts',(22.9699652635309,-49.946700848752,-38.1097274249748));
#29578=CARTESIAN_POINT('Ctrl Pts',(21.5789465666081,-47.4839596279891,-37.9517789017824));
#29579=CARTESIAN_POINT('Ctrl Pts',(18.7563455452306,-47.3024350489073,-37.7938303785899));
#29580=CARTESIAN_POINT('Ctrl Pts',(17.0613279398084,-49.5667108905587,-37.6358818553975));
#29581=CARTESIAN_POINT('Ctrl Pts',(18.0307150433377,-52.223836627966,-37.477933332205));
#29582=CARTESIAN_POINT('Ctrl Pts',(20.7855928598664,-52.8646774110371,-37.3199848090125));
#29583=CARTESIAN_POINT('Ctrl Pts',(22.8281975552819,-50.9082022699088,-37.1620362858201));
#29584=CARTESIAN_POINT('Ctrl Pts',(22.3065615268905,-48.1282877728884,-37.0040877626276));
#29585=CARTESIAN_POINT('Ctrl Pts',(19.6936363210884,-47.0453978163343,-36.8461392394351));
#29586=CARTESIAN_POINT('Ctrl Pts',(17.3584817412455,-48.6413558047206,-36.6881907162427));
#29587=CARTESIAN_POINT('Ctrl Pts',(17.4183114305182,-51.4691551610726,-36.5302421930502));
#29588=CARTESIAN_POINT('Ctrl Pts',(19.8188796262023,-52.9649162165198,-36.3722936698577));
#29589=CARTESIAN_POINT('Ctrl Pts',(22.3836641567986,-51.7724779116434,-36.2143451466652));
#29590=CARTESIAN_POINT('Ctrl Pts',(22.7872528920342,-48.9729877920881,-36.0563966234728));
#29591=CARTESIAN_POINT('Ctrl Pts',(20.6637242006576,-47.1046584061167,-35.8984481002803));
#29592=CARTESIAN_POINT('Ctrl Pts',(17.9384169627383,-47.8614471855684,-35.7404995770878));
#29593=CARTESIAN_POINT('Ctrl Pts',(17.0822843645233,-50.5571967606797,-35.5825510538954));
#29594=CARTESIAN_POINT('Ctrl Pts',(18.8715557946688,-52.7477529792771,-35.4246025307029));
#29595=CARTESIAN_POINT('Ctrl Pts',(21.6839532657172,-52.4470051406827,-35.2666540075104));
#29596=CARTESIAN_POINT('Ctrl Pts',(22.9695615258592,-49.9276321633338,-35.108705484318));
#29597=CARTESIAN_POINT('Ctrl Pts',(21.562758665638,-47.4738729025192,-34.9507569611255));
#29598=CARTESIAN_POINT('Ctrl Pts',(18.739050052438,-47.3104762523091,-34.792808437933));
#29599=CARTESIAN_POINT('Ctrl Pts',(17.058606406634,-49.5855889859624,-34.6348599147405));
#29600=CARTESIAN_POINT('Ctrl Pts',(18.0450348734924,-52.2364355823028,-34.4769113915481));
#29601=CARTESIAN_POINT('Ctrl Pts',(20.8039707629787,-52.8595740542826,-34.3189628683556));
#29602=CARTESIAN_POINT('Ctrl Pts',(22.8339708133377,-50.8900237012579,-34.1610143451632));
#29603=CARTESIAN_POINT('Ctrl Pts',(22.2944957185695,-48.11351592715,-34.0030658219707));
#29604=CARTESIAN_POINT('Ctrl Pts',(19.6746711397071,-47.0474258870756,-33.8451172987782));
#29605=CARTESIAN_POINT('Ctrl Pts',(17.3498123440423,-48.6583449967074,-33.6871687755857));
#29606=CARTESIAN_POINT('Ctrl Pts',(17.4277980942202,-51.4857018932322,-33.5292202523933));
#29607=CARTESIAN_POINT('Ctrl Pts',(19.837921082384,-52.9660180687438,-33.3712717292008));
#29608=CARTESIAN_POINT('Ctrl Pts',(22.3949960957427,-51.7571358686874,-33.2133232060084));
#29609=CARTESIAN_POINT('Ctrl Pts',(22.7806009896051,-48.9551120173637,-33.0553746828159));
#29610=CARTESIAN_POINT('Ctrl Pts',(20.6451195343488,-47.100456321065,-32.8974261596234));
#29611=CARTESIAN_POINT('Ctrl Pts',(17.9247278177222,-47.8747286928219,-32.7394776364309));
#29612=CARTESIAN_POINT('Ctrl Pts',(17.0859222722165,-50.5759199215923,-32.5815291132385));
#29613=CARTESIAN_POINT('Ctrl Pts',(18.8892223748244,-52.7549420732675,-32.423580590046));
#29614=CARTESIAN_POINT('Ctrl Pts',(21.6996307674046,-52.4361420348868,-32.2656320668536));
#29615=CARTESIAN_POINT('Ctrl Pts',(22.9690356351122,-49.9085661053849,-32.107683543661));
#29616=CARTESIAN_POINT('Ctrl Pts',(21.5465061916006,-47.4638905072944,-31.9497350204686));
#29617=CARTESIAN_POINT('Ctrl Pts',(18.7218066190244,-47.3186282539564,-31.7917864972761));
#29618=CARTESIAN_POINT('Ctrl Pts',(17.0560061104844,-49.6044842125209,-31.6338379740837));
#29619=CARTESIAN_POINT('Ctrl Pts',(18.0594353240415,-52.2489423065238,-31.4758894508912));
#29620=CARTESIAN_POINT('Ctrl Pts',(20.8223155096835,-52.8543528096899,-31.3179409276987));
#29621=CARTESIAN_POINT('Ctrl Pts',(22.8396272322911,-50.8718084315267,-31.1599924045063));
#29622=CARTESIAN_POINT('Ctrl Pts',(22.2823353067388,-48.0988218633531,-31.0020438813138));
#29623=CARTESIAN_POINT('Ctrl Pts',(19.655719372657,-47.049575689958,-30.8440953581213));
#29624=CARTESIAN_POINT('Ctrl Pts',(17.3412522125651,-48.6753895053789,-30.6861468349288));
#29625=CARTESIAN_POINT('Ctrl Pts',(17.4373908091818,-51.5021873700654,-30.5281983117364));
#29626=CARTESIAN_POINT('Ctrl Pts',(19.8569692208779,-52.9669976332779,-30.3702497885439));
#29627=CARTESIAN_POINT('Ctrl Pts',(22.4062292899195,-51.7417213795498,-30.2123012653515));
#29628=CARTESIAN_POINT('Ctrl Pts',(22.773834443947,-48.9372793230483,-30.054352742159));
#29629=CARTESIAN_POINT('Ctrl Pts',(20.6264882700084,-47.096373783144,-29.8964042189665));
#29630=CARTESIAN_POINT('Ctrl Pts',(17.9111242354336,-47.8880978242769,-29.738455695774));
#29631=CARTESIAN_POINT('Ctrl Pts',(17.0896803263047,-50.5946193375101,-29.5805071725816));
#29632=CARTESIAN_POINT('Ctrl Pts',(18.9069347519471,-52.7620175820056,-29.4225586493891));
#29633=CARTESIAN_POINT('Ctrl Pts',(21.7152381939154,-52.4251784877586,-29.2646101261966));
#29634=CARTESIAN_POINT('Ctrl Pts',(22.9683873320859,-49.8895038173406,-29.1066616030042));
#29635=CARTESIAN_POINT('Ctrl Pts',(21.5301899556464,-47.4540126747319,-28.9487130798117));
#29636=CARTESIAN_POINT('Ctrl Pts',(18.7046158851008,-47.3268908080728,-28.7907645566192));
#29637=CARTESIAN_POINT('Ctrl Pts',(17.0535271940985,-49.6233957451342,-28.6328160334268));
#29638=CARTESIAN_POINT('Ctrl Pts',(18.0739157835043,-52.2613563094843,-28.4748675102343));
#29639=CARTESIAN_POINT('Ctrl Pts',(20.8406263523719,-52.8490138774931,-28.3169189870418));
#29640=CARTESIAN_POINT('Ctrl Pts',(22.8451665748976,-50.8535572247102,-28.1589704638494));
#29641=CARTESIAN_POINT('Ctrl Pts',(22.2700807940834,-48.0842061699878,-28.0010219406569));
#29642=CARTESIAN_POINT('Ctrl Pts',(19.636781802065,-47.0518471665959,-27.8430734174644));
#29643=CARTESIAN_POINT('Ctrl Pts',(17.3328016965531,-48.6924885699155,-27.685124894272));
#29644=CARTESIAN_POINT('Ctrl Pts',(17.447089187104,-51.5186110264415,-27.5271763710795));
#29645=CARTESIAN_POINT('Ctrl Pts',(19.8760232415626,-52.9678546421884,-27.369227847887));
#29646=CARTESIAN_POINT('Ctrl Pts',(22.4173633058167,-51.7262355325375,-27.2112793246946));
#29647=CARTESIAN_POINT('Ctrl Pts',(22.7669534749441,-48.9194895430439,-27.0533308015021));
#29648=CARTESIAN_POINT('Ctrl Pts',(20.6078312935152,-47.0924127551611,-26.8953822783097));
#29649=CARTESIAN_POINT('Ctrl Pts',(17.897606542339,-47.901550455944,-26.7374337551171));
#29650=CARTESIAN_POINT('Ctrl Pts',(17.093558838557,-50.6133013508559,-26.5794852319247));
#29651=CARTESIAN_POINT('Ctrl Pts',(18.9246912665317,-52.7689650510212,-26.4215367087322));
#29652=CARTESIAN_POINT('Ctrl Pts',(21.73077675186,-52.4141431493388,-26.2635881855398));
#29653=CARTESIAN_POINT('Ctrl Pts',(22.9676129599786,-49.8703899428698,-26.1056396623473));
#29654=CARTESIAN_POINT('Ctrl Pts',(21.5138179641941,-47.4443515918095,-25.9476911391548));
#29655=CARTESIAN_POINT('Ctrl Pts',(18.6874639605827,-47.3350410138954,-25.7897426159623));
#29656=CARTESIAN_POINT('Ctrl Pts',(17.051198793608,-49.6427660073601,-25.6317940927699));
#29657=CARTESIAN_POINT('Ctrl Pts',(18.0884182569644,-52.2727935686328,-25.4738455695774));
#29658=CARTESIAN_POINT('Ctrl Pts',(20.8590114992225,-52.8453305550081,-25.3158970463849));
#29659=CARTESIAN_POINT('Ctrl Pts',(22.8504308442221,-50.8315713776829,-25.1579485231925));
#29660=CARTESIAN_POINT('Ctrl Pts',(22.4546613829867,-48.9970000028466,-25.0526495077308));
#29661=CARTESIAN_POINT('Ctrl Pts',(21.9134659966651,-48.3640127966251,-25.));
#29662=CARTESIAN_POINT('Ctrl Pts',(22.514945820706,-49.9982392595312,-39.112583302492));
#29663=CARTESIAN_POINT('Ctrl Pts',(22.5168590395215,-49.7066908675705,-39.0941950563712));
#29664=CARTESIAN_POINT('Ctrl Pts',(22.4699890228872,-49.4157373171367,-39.0758068102504));
#29665=CARTESIAN_POINT('Ctrl Pts',(22.3716202189689,-49.1433861578537,-39.0574185641297));
#29666=CARTESIAN_POINT('Ctrl Pts',(22.0899691540247,-48.3635861501753,-39.0047690563988));
#29667=CARTESIAN_POINT('Ctrl Pts',(21.386130933873,-47.7362885802094,-38.952119548668));
#29668=CARTESIAN_POINT('Ctrl Pts',(20.5791956248474,-47.5458493355713,-38.8994700409372));
#29669=CARTESIAN_POINT('Ctrl Pts',(19.7722603158218,-47.3554100909331,-38.8468205332064));
#29670=CARTESIAN_POINT('Ctrl Pts',(18.8622279179223,-47.6018291716227,-38.7941710254756));
#29671=CARTESIAN_POINT('Ctrl Pts',(18.2616398883468,-48.1734062429628,-38.7415215177447));
#29672=CARTESIAN_POINT('Ctrl Pts',(17.6610518587713,-48.7449833143029,-38.6888720100139));
#29673=CARTESIAN_POINT('Ctrl Pts',(17.3699081975197,-49.6417183762935,-38.6362225022831));
#29674=CARTESIAN_POINT('Ctrl Pts',(17.520198419741,-50.457085198288,-38.5835729945523));
#29675=CARTESIAN_POINT('Ctrl Pts',(17.6704886419622,-51.2724520202826,-38.5309234868215));
#29676=CARTESIAN_POINT('Ctrl Pts',(18.2622127476563,-52.006450602281,-38.4782739790906));
#29677=CARTESIAN_POINT('Ctrl Pts',(19.0271196209408,-52.3263363736636,-38.4256244713598));
#29678=CARTESIAN_POINT('Ctrl Pts',(19.7920264942254,-52.6462221450461,-38.372974963629));
#29679=CARTESIAN_POINT('Ctrl Pts',(20.7301161351005,-52.5519951058128,-38.3203254558982));
#29680=CARTESIAN_POINT('Ctrl Pts',(21.4161208701306,-52.0863703832249,-38.2676759481673));
#29681=CARTESIAN_POINT('Ctrl Pts',(22.0897219089449,-51.6291646515194,-38.2159783996089));
#29682=CARTESIAN_POINT('Ctrl Pts',(22.5202715562231,-50.8138703486238,-38.1642808510504));
#29683=CARTESIAN_POINT('Ctrl Pts',(22.5215368448905,-49.9997267149633,-38.112583302492));
#29684=CARTESIAN_POINT('Origin',(20.,-50.,-32.));
#29685=CARTESIAN_POINT('',(20.,-52.5175,-24.3199761284063));
#29686=CARTESIAN_POINT('Ctrl Pts',(17.4825,-50.,-25.));
#29687=CARTESIAN_POINT('Ctrl Pts',(17.4825,-50.3222180082023,-25.));
#29688=CARTESIAN_POINT('Ctrl Pts',(17.5480817994189,-50.6620957154614,-24.965994767533));
#29689=CARTESIAN_POINT('Ctrl Pts',(17.8069078640769,-51.2808669639972,-24.8434341672334));
#29690=CARTESIAN_POINT('Ctrl Pts',(17.9998598225217,-51.560142465796,-24.75619390213));
#29691=CARTESIAN_POINT('Ctrl Pts',(18.4404784589042,-52.0007611021785,-24.5883213994305));
#29692=CARTESIAN_POINT('Ctrl Pts',(18.719545764891,-52.1932581515168,-24.4956547875015));
#29693=CARTESIAN_POINT('Ctrl Pts',(19.3374025937983,-52.4517149721102,-24.3600905047278));
#29694=CARTESIAN_POINT('Ctrl Pts',(19.6768725637946,-52.5175,-24.3199761284063));
#29695=CARTESIAN_POINT('Ctrl Pts',(20.,-52.5175,-24.3199761284063));
#29696=CARTESIAN_POINT('Ctrl Pts',(20.,-52.5175,-24.3199761284063));
#29697=CARTESIAN_POINT('Ctrl Pts',(20.3231274362054,-52.5175,-24.3199761284063));
#29698=CARTESIAN_POINT('Ctrl Pts',(20.6625974062016,-52.4517149721102,-24.3600905047278));
#29699=CARTESIAN_POINT('Ctrl Pts',(21.2804542351089,-52.1932581515168,-24.4956547875015));
#29700=CARTESIAN_POINT('Ctrl Pts',(21.5595215410957,-52.0007611021785,-24.5883213994305));
#29701=CARTESIAN_POINT('Ctrl Pts',(22.0001401774783,-51.560142465796,-24.75619390213));
#29702=CARTESIAN_POINT('Ctrl Pts',(22.1930921359231,-51.2808669639972,-24.8434341672334));
#29703=CARTESIAN_POINT('Ctrl Pts',(22.4519182005811,-50.6620957154615,-24.965994767533));
#29704=CARTESIAN_POINT('Ctrl Pts',(22.5175,-50.3222180082023,-25.));
#29705=CARTESIAN_POINT('Ctrl Pts',(22.5175,-50.,-25.));
#29706=CARTESIAN_POINT('Origin',(20.,-50.,-32.));
#29707=CARTESIAN_POINT('Origin',(-20.,-50.,-24.));
#29708=CARTESIAN_POINT('Origin',(-20.,50.,-24.));
#29709=CARTESIAN_POINT('Origin',(20.,50.,-32.));
#29710=CARTESIAN_POINT('Origin',(20.,66.,25.));
#29711=CARTESIAN_POINT('Ctrl Pts',(19.2300979593296,64.5225674811446,25.));
#29712=CARTESIAN_POINT('Ctrl Pts',(19.281839231255,64.4874948330505,25.));
#29713=CARTESIAN_POINT('Ctrl Pts',(19.3355569853841,64.4556772697649,25.));
#29714=CARTESIAN_POINT('Ctrl Pts',(19.3909199227331,64.4270507505591,25.));
#29715=CARTESIAN_POINT('Ctrl Pts',(19.426030142418,64.4088963059748,25.));
#29716=CARTESIAN_POINT('Ctrl Pts',(19.4618029278252,64.3920259076849,25.));
#29717=CARTESIAN_POINT('Ctrl Pts',(19.4981613804728,64.3764304346951,25.));
#29718=CARTESIAN_POINT('Ctrl Pts',(19.5229472314038,64.365798874753,25.));
#29719=CARTESIAN_POINT('Ctrl Pts',(19.5480053751662,64.3557599229072,25.));
#29720=CARTESIAN_POINT('Ctrl Pts',(19.5733126916688,64.3463122740479,25.));
#29721=CARTESIAN_POINT('Ctrl Pts',(19.5868015745102,64.3412766461662,25.));
#29722=CARTESIAN_POINT('Ctrl Pts',(19.6003611975298,64.336409177933,25.));
#29723=CARTESIAN_POINT('Ctrl Pts',(19.6139743572948,64.33171419315,25.));
#29724=CARTESIAN_POINT('Ctrl Pts',(19.6763387771318,64.3102055935898,25.));
#29725=CARTESIAN_POINT('Ctrl Pts',(19.7398944948615,64.2922866657573,25.));
#29726=CARTESIAN_POINT('Ctrl Pts',(19.8042916188756,64.2779108681233,25.));
#29727=CARTESIAN_POINT('Ctrl Pts',(19.850744007574,64.267540992919,25.));
#29728=CARTESIAN_POINT('Ctrl Pts',(19.897635109279,64.2590155593061,25.));
#29729=CARTESIAN_POINT('Ctrl Pts',(19.9448427078687,64.2523311286925,25.));
#29730=CARTESIAN_POINT('Ctrl Pts',(19.9577423603646,64.2505045830807,25.));
#29731=CARTESIAN_POINT('Ctrl Pts',(19.9706656780993,64.2488155711042,25.));
#29732=CARTESIAN_POINT('Ctrl Pts',(19.9836102341249,64.247264183342,25.));
#29733=CARTESIAN_POINT('Ctrl Pts',(19.9969403079863,64.2456665917817,25.));
#29734=CARTESIAN_POINT('Ctrl Pts',(20.0102849815179,64.2442159339093,25.));
#29735=CARTESIAN_POINT('Ctrl Pts',(20.0236360018045,64.2429122860894,25.));
#29736=CARTESIAN_POINT('Ctrl Pts',(20.0911671831916,64.2363182673923,25.));
#29737=CARTESIAN_POINT('Ctrl Pts',(20.1589020463386,64.2334766424509,25.));
#29738=CARTESIAN_POINT('Ctrl Pts',(20.2264859165014,64.2343394624463,25.));
#29739=CARTESIAN_POINT('Ctrl Pts',(20.295048342074,64.2352147753216,25.));
#29740=CARTESIAN_POINT('Ctrl Pts',(20.3634563804349,64.239902250275,25.));
#29741=CARTESIAN_POINT('Ctrl Pts',(20.4313612181172,64.2484001199632,25.));
#29742=CARTESIAN_POINT('Ctrl Pts',(20.4734290714963,64.2536646511553,25.));
#29743=CARTESIAN_POINT('Ctrl Pts',(20.5153041663473,64.2603925631682,25.));
#29744=CARTESIAN_POINT('Ctrl Pts',(20.5569049437151,64.2685933800542,25.));
#29745=CARTESIAN_POINT('Ctrl Pts',(20.5909685471161,64.2753083837547,25.));
#29746=CARTESIAN_POINT('Ctrl Pts',(20.6248482693332,64.2830110591366,25.));
#29747=CARTESIAN_POINT('Ctrl Pts',(20.6584989914886,64.2917106170954,25.));
#29748=CARTESIAN_POINT('Ctrl Pts',(20.6722821250041,64.2952739037411,25.));
#29749=CARTESIAN_POINT('Ctrl Pts',(20.6860293036811,64.2990053184497,25.));
#29750=CARTESIAN_POINT('Ctrl Pts',(20.6997141699917,64.3028986531347,25.));
#29751=CARTESIAN_POINT('Ctrl Pts',(20.767509458307,64.3221863642084,25.));
#29752=CARTESIAN_POINT('Ctrl Pts',(20.8338951499891,64.3454732746142,25.));
#29753=CARTESIAN_POINT('Ctrl Pts',(20.8985085156353,64.3727406748912,25.));
#29754=CARTESIAN_POINT('Ctrl Pts',(20.9056752429655,64.3757650959352,25.));
#29755=CARTESIAN_POINT('Ctrl Pts',(20.912820174029,64.3788385395555,25.));
#29756=CARTESIAN_POINT('Ctrl Pts',(20.9199428180022,64.381961019588,25.));
#29757=CARTESIAN_POINT('Ctrl Pts',(20.9816953861963,64.4090325904643,25.));
#29758=CARTESIAN_POINT('Ctrl Pts',(21.0417735205151,64.4397857609011,25.));
#29759=CARTESIAN_POINT('Ctrl Pts',(21.1000352843316,64.4739103291622,25.));
#29760=CARTESIAN_POINT('Ctrl Pts',(21.1627111717192,64.5106202990872,25.));
#29761=CARTESIAN_POINT('Ctrl Pts',(21.2232860382956,64.5512318872835,25.));
#29762=CARTESIAN_POINT('Ctrl Pts',(21.2815632966598,64.5954199888185,25.));
#29763=CARTESIAN_POINT('Ctrl Pts',(21.2920884895073,64.6034006025823,25.));
#29764=CARTESIAN_POINT('Ctrl Pts',(21.3025386647321,64.6114980246855,25.));
#29765=CARTESIAN_POINT('Ctrl Pts',(21.3129125592066,64.6197105288189,25.));
#29766=CARTESIAN_POINT('Ctrl Pts',(21.3220886651644,64.6269748024524,25.));
#29767=CARTESIAN_POINT('Ctrl Pts',(21.3311980890197,64.6343235975034,25.));
#29768=CARTESIAN_POINT('Ctrl Pts',(21.3402381792021,64.641753616724,25.));
#29769=CARTESIAN_POINT('Ctrl Pts',(21.3951413928709,64.6868783803714,25.));
#29770=CARTESIAN_POINT('Ctrl Pts',(21.4475124849223,64.7350138905591,25.));
#29771=CARTESIAN_POINT('Ctrl Pts',(21.4972014371838,64.7858101432121,25.));
#29772=CARTESIAN_POINT('Ctrl Pts',(21.54793815392,64.8376775093934,25.));
#29773=CARTESIAN_POINT('Ctrl Pts',(21.5958791893217,64.8923195535381,25.));
#29774=CARTESIAN_POINT('Ctrl Pts',(21.6408446258094,64.9494149499861,25.));
#29775=CARTESIAN_POINT('Ctrl Pts',(21.686082829692,65.00685669607,25.));
#29776=CARTESIAN_POINT('Ctrl Pts',(21.7283100119046,65.0667823784968,25.));
#29777=CARTESIAN_POINT('Ctrl Pts',(21.7673110082825,65.1289063303553,25.));
#29778=CARTESIAN_POINT('Ctrl Pts',(21.7769380340976,65.1442410382814,25.));
#29779=CARTESIAN_POINT('Ctrl Pts',(21.7863683037242,65.1597098543281,25.));
#29780=CARTESIAN_POINT('Ctrl Pts',(21.7955981964646,65.1753087874189,25.));
#29781=CARTESIAN_POINT('Ctrl Pts',(21.8028478722767,65.1875610650027,25.));
#29782=CARTESIAN_POINT('Ctrl Pts',(21.8099746659192,65.199895168117,25.));
#29783=CARTESIAN_POINT('Ctrl Pts',(21.8169663572284,65.212290083603,25.));
#29784=CARTESIAN_POINT('Ctrl Pts',(21.8539815854589,65.2779109191527,25.));
#29785=CARTESIAN_POINT('Ctrl Pts',(21.8872827332467,65.3453487040639,25.));
#29786=CARTESIAN_POINT('Ctrl Pts',(21.9166890670406,65.4142571139814,25.));
#29787=CARTESIAN_POINT('Ctrl Pts',(21.9461274772774,65.4832406892256,25.));
#29788=CARTESIAN_POINT('Ctrl Pts',(21.9716633369393,65.5536989287888,25.));
#29789=CARTESIAN_POINT('Ctrl Pts',(21.9930795831037,65.625322085145,25.));
#29790=CARTESIAN_POINT('Ctrl Pts',(22.014008595814,65.6953157683622,25.));
#29791=CARTESIAN_POINT('Ctrl Pts',(22.0310038676764,65.7664228433862,25.));
#29792=CARTESIAN_POINT('Ctrl Pts',(22.0438192119979,65.8383774372798,25.));
#29793=CARTESIAN_POINT('Ctrl Pts',(22.0465680662148,65.8538114891385,25.));
#29794=CARTESIAN_POINT('Ctrl Pts',(22.0491244257846,65.8692845939399,25.));
#29795=CARTESIAN_POINT('Ctrl Pts',(22.0514855533718,65.8847942120883,25.));
#29796=CARTESIAN_POINT('Ctrl Pts',(22.0534987458236,65.8980183370176,25.));
#29797=CARTESIAN_POINT('Ctrl Pts',(22.0553700032061,65.9112690075299,25.));
#29798=CARTESIAN_POINT('Ctrl Pts',(22.0571001530702,65.9245445252814,25.));
#29799=CARTESIAN_POINT('Ctrl Pts',(21.8174278887594,66.9586205879594,25.));
#29800=CARTESIAN_POINT('Ctrl Pts',(21.7765814107043,67.0211003513439,25.));
#29801=CARTESIAN_POINT('Ctrl Pts',(21.7321382448712,67.0810293930508,25.));
#29802=CARTESIAN_POINT('Ctrl Pts',(21.6844272397568,67.1382579399872,25.));
#29803=CARTESIAN_POINT('Ctrl Pts',(21.637967675109,67.1939854051645,25.));
#29804=CARTESIAN_POINT('Ctrl Pts',(21.5884084550957,67.2471523904015,25.));
#29805=CARTESIAN_POINT('Ctrl Pts',(21.5360271611327,67.2975829314462,25.));
#29806=CARTESIAN_POINT('Ctrl Pts',(21.5243354888859,67.3088391894062,25.));
#29807=CARTESIAN_POINT('Ctrl Pts',(21.5125015557441,67.3199604168664,25.));
#29808=CARTESIAN_POINT('Ctrl Pts',(21.5005334335621,67.3309397166112,25.));
#29809=CARTESIAN_POINT('Ctrl Pts',(21.4456122493378,67.3813232383342,25.));
#29810=CARTESIAN_POINT('Ctrl Pts',(21.3879773343812,67.4286222799669,25.));
#29811=CARTESIAN_POINT('Ctrl Pts',(21.3279448353606,67.4726643541928,25.));
#29812=CARTESIAN_POINT('Ctrl Pts',(21.2858003429978,67.5035831213795,25.));
#29813=CARTESIAN_POINT('Ctrl Pts',(21.2424735350058,67.5328958196392,25.));
#29814=CARTESIAN_POINT('Ctrl Pts',(21.1980684694414,67.5605283676983,25.));
#29815=CARTESIAN_POINT('Ctrl Pts',(21.1811930594238,67.5710296601162,25.));
#29816=CARTESIAN_POINT('Ctrl Pts',(21.1641618931168,67.5812881669686,25.));
#29817=CARTESIAN_POINT('Ctrl Pts',(21.1469806065534,67.5912993349929,25.));
#29818=CARTESIAN_POINT('Ctrl Pts',(21.1305958626812,67.6008463746361,25.));
#29819=CARTESIAN_POINT('Ctrl Pts',(21.1140692794188,67.6101712136826,25.));
#29820=CARTESIAN_POINT('Ctrl Pts',(21.0974353366829,67.6192539953179,25.));
#29821=CARTESIAN_POINT('Ctrl Pts',(21.0337183685953,67.6540459455365,25.));
#29822=CARTESIAN_POINT('Ctrl Pts',(20.9683624441582,67.6853307441412,25.));
#29823=CARTESIAN_POINT('Ctrl Pts',(20.9016592645668,67.712946755633,25.));
#29824=CARTESIAN_POINT('Ctrl Pts',(20.8363884218304,67.7399697604452,25.));
#29825=CARTESIAN_POINT('Ctrl Pts',(20.7698266382456,67.7634800022219,25.));
#29826=CARTESIAN_POINT('Ctrl Pts',(20.7022386209724,67.7832777771816,25.));
#29827=CARTESIAN_POINT('Ctrl Pts',(20.6361329278297,67.8026413521051,25.));
#29828=CARTESIAN_POINT('Ctrl Pts',(20.5690447597529,67.8184536274702,25.));
#29829=CARTESIAN_POINT('Ctrl Pts',(20.5012257200427,67.8304791677269,25.));
#29830=CARTESIAN_POINT('Ctrl Pts',(20.479165553528,67.8343908335604,25.));
#29831=CARTESIAN_POINT('Ctrl Pts',(20.4570281345296,67.8379014394019,25.));
#29832=CARTESIAN_POINT('Ctrl Pts',(20.4348224165778,67.8410017088834,25.));
#29833=CARTESIAN_POINT('Ctrl Pts',(20.4223379067786,67.8427447439344,25.));
#29834=CARTESIAN_POINT('Ctrl Pts',(20.4098305231907,67.844358118475,25.));
#29835=CARTESIAN_POINT('Ctrl Pts',(20.3973195611165,67.8458383045697,25.));
#29836=CARTESIAN_POINT('Ctrl Pts',(20.3294889065971,67.85386342614,25.));
#29837=CARTESIAN_POINT('Ctrl Pts',(20.2614347205481,67.857995328394,25.));
#29838=CARTESIAN_POINT('Ctrl Pts',(20.1934027269559,67.8580559708634,25.));
#29839=CARTESIAN_POINT('Ctrl Pts',(20.1836058007518,67.8580647036635,25.));
#29840=CARTESIAN_POINT('Ctrl Pts',(20.1738093409654,67.8579889211747,25.));
#29841=CARTESIAN_POINT('Ctrl Pts',(20.1640140908158,67.8578280017397,25.));
#29842=CARTESIAN_POINT('Ctrl Pts',(20.0946498528238,67.8566884643292,25.));
#29843=CARTESIAN_POINT('Ctrl Pts',(20.0253448166408,67.8512836465463,25.));
#29844=CARTESIAN_POINT('Ctrl Pts',(19.9564239887308,67.8417867762202,25.));
#29845=CARTESIAN_POINT('Ctrl Pts',(19.8921287237172,67.8329272802895,25.));
#29846=CARTESIAN_POINT('Ctrl Pts',(19.8281673125328,67.8205056461074,25.));
#29847=CARTESIAN_POINT('Ctrl Pts',(19.7648241284675,67.8046280687348,25.));
#29848=CARTESIAN_POINT('Ctrl Pts',(19.7509594847671,67.8011527626487,25.));
#29849=CARTESIAN_POINT('Ctrl Pts',(19.7371245581731,67.7975117747354,25.));
#29850=CARTESIAN_POINT('Ctrl Pts',(19.7233225085399,67.7937060404833,25.));
#29851=CARTESIAN_POINT('Ctrl Pts',(19.7122620885151,67.790656274655,25.));
#29852=CARTESIAN_POINT('Ctrl Pts',(19.7012233271795,67.7875007728397,25.));
#29853=CARTESIAN_POINT('Ctrl Pts',(19.6902209057537,67.7842441420852,25.));
#29854=CARTESIAN_POINT('Ctrl Pts',(19.624658693414,67.7648382396226,25.));
#29855=CARTESIAN_POINT('Ctrl Pts',(19.560262855601,67.7418123378998,25.));
#29856=CARTESIAN_POINT('Ctrl Pts',(19.4973358510903,67.7153484561744,25.));
#29857=CARTESIAN_POINT('Ctrl Pts',(19.4347002019695,67.6890071036341,25.));
#29858=CARTESIAN_POINT('Ctrl Pts',(19.3735189237464,67.6592588311679,25.));
#29859=CARTESIAN_POINT('Ctrl Pts',(19.3141200864186,67.6262415908821,25.));
#29860=CARTESIAN_POINT('Ctrl Pts',(19.2559939626492,67.5939317969245,25.));
#29861=CARTESIAN_POINT('Ctrl Pts',(19.199574042523,67.5584909174538,25.));
#29862=CARTESIAN_POINT('Ctrl Pts',(19.1452076937093,67.5200188262395,25.));
#29863=CARTESIAN_POINT('Ctrl Pts',(19.1337111877064,67.5118833778005,25.));
#29864=CARTESIAN_POINT('Ctrl Pts',(19.1223066761945,67.5036122974171,25.));
#29865=CARTESIAN_POINT('Ctrl Pts',(19.1109977221854,67.4952064007952,25.));
#29866=CARTESIAN_POINT('Ctrl Pts',(19.100366622277,67.4873043501958,25.));
#29867=CARTESIAN_POINT('Ctrl Pts',(19.0898187360985,67.4792820489923,25.));
#29868=CARTESIAN_POINT('Ctrl Pts',(19.0793736026688,67.4711534357938,25.));
#29869=CARTESIAN_POINT('Ctrl Pts',(19.0278061913906,67.4310226377767,25.));
#29870=CARTESIAN_POINT('Ctrl Pts',(18.9786453544672,67.3882343524051,25.));
#29871=CARTESIAN_POINT('Ctrl Pts',(18.9321821714341,67.3429205912564,25.));
#29872=CARTESIAN_POINT('Ctrl Pts',(18.886602631737,67.2984686135769,25.));
#29873=CARTESIAN_POINT('Ctrl Pts',(18.8436185304839,67.2515856441284,25.));
#29874=CARTESIAN_POINT('Ctrl Pts',(18.8035471707609,67.2023705436618,25.));
#29875=CARTESIAN_POINT('Ctrl Pts',(18.7647769323282,67.154753462715,25.));
#29876=CARTESIAN_POINT('Ctrl Pts',(18.7287330112329,67.1049526682313,25.));
#29877=CARTESIAN_POINT('Ctrl Pts',(18.6957494603037,67.0530423374834,25.));
#29878=CARTESIAN_POINT('Ctrl Pts',(18.6902971461602,67.0444613502168,25.));
#29879=CARTESIAN_POINT('Ctrl Pts',(18.684928570876,67.0358226946663,25.));
#29880=CARTESIAN_POINT('Ctrl Pts',(18.6796453811788,67.0271266799546,25.));
#29881=CARTESIAN_POINT('Ctrl Pts',(18.6739897987629,67.0178177149714,25.));
#29882=CARTESIAN_POINT('Ctrl Pts',(18.6684320638271,67.0084430187688,25.));
#29883=CARTESIAN_POINT('Ctrl Pts',(18.6629725798064,66.9990042518226,25.));
#29884=CARTESIAN_POINT('Origin',(20.,66.,37.5459252805377));
#29885=CARTESIAN_POINT('Ctrl Pts',(17.9434278899737,66.0014963127332,35.7959252805377));
#29886=CARTESIAN_POINT('Ctrl Pts',(17.9426109499923,66.0996692927701,35.7905876687522));
#29887=CARTESIAN_POINT('Ctrl Pts',(17.9936360748142,66.8783591116969,35.7482056843029));
#29888=CARTESIAN_POINT('Ctrl Pts',(18.9885906510386,68.2081813101826,35.6687793271897));
#29889=CARTESIAN_POINT('Ctrl Pts',(21.3064560191417,68.0471889261963,35.5576462091981));
#29890=CARTESIAN_POINT('Ctrl Pts',(22.4285781845706,66.0128601788243,35.4465130912066));
#29891=CARTESIAN_POINT('Ctrl Pts',(21.3279816597525,63.9665950349013,35.335379973215));
#29892=CARTESIAN_POINT('Ctrl Pts',(19.0119582073911,63.7814655261371,35.2242468552234));
#29893=CARTESIAN_POINT('Ctrl Pts',(17.9980259373779,65.1068137265861,35.144428624331));
#29894=CARTESIAN_POINT('Ctrl Pts',(17.9427193490685,65.892962776772,35.1016547661024));
#29895=CARTESIAN_POINT('Ctrl Pts',(17.9436249754829,65.9983937900349,35.0959252805377));
#29896=CARTESIAN_POINT('Ctrl Pts',(17.9473272485919,65.9976786215907,35.8540747194623));
#29897=CARTESIAN_POINT('Ctrl Pts',(17.9508754702579,66.467827503345,35.8286277343138));
#29898=CARTESIAN_POINT('Ctrl Pts',(18.3433678783681,67.6294026063953,35.7661363765015));
#29899=CARTESIAN_POINT('Ctrl Pts',(20.2718170903172,68.4128312567252,35.6666006460253));
#29900=CARTESIAN_POINT('Ctrl Pts',(22.1745315590613,67.0812974610511,35.5554675280338));
#29901=CARTESIAN_POINT('Ctrl Pts',(22.0878552063855,64.7590834656903,35.4443344100422));
#29902=CARTESIAN_POINT('Ctrl Pts',(20.0898773670193,63.5731233891133,35.3332012920506));
#29903=CARTESIAN_POINT('Ctrl Pts',(18.2789899846852,64.474160336193,35.2364480618574));
#29904=CARTESIAN_POINT('Ctrl Pts',(17.95008404285,65.581879078884,35.1767392043279));
#29905=CARTESIAN_POINT('Ctrl Pts',(17.9479090025127,66.0011644690241,35.1540747194623));
#29906=CARTESIAN_POINT('Ctrl Pts',(21.2690708798523,67.0793586530486,36.));
#29907=CARTESIAN_POINT('Ctrl Pts',(21.627967898288,66.6573805147569,35.9629556273362));
#29908=CARTESIAN_POINT('Ctrl Pts',(21.8852403009264,65.4342572368484,35.8888668820084));
#29909=CARTESIAN_POINT('Ctrl Pts',(20.5452623374803,64.1066463862456,35.7777337640169));
#29910=CARTESIAN_POINT('Ctrl Pts',(18.7059924808176,64.516301386891,35.6666006460253));
#29911=CARTESIAN_POINT('Ctrl Pts',(18.0511940983536,66.2817529495446,35.5554675280338));
#29912=CARTESIAN_POINT('Ctrl Pts',(19.1799450174622,67.7904027559382,35.4443344100422));
#29913=CARTESIAN_POINT('Ctrl Pts',(21.0592800719747,67.6598694493458,35.3332012920506));
#29914=CARTESIAN_POINT('Ctrl Pts',(21.9691014748727,66.0104270874417,35.2220681740591));
#29915=CARTESIAN_POINT('Ctrl Pts',(21.0767331525235,64.3513066446749,35.1109350560675));
#29916=CARTESIAN_POINT('Ctrl Pts',(19.1988915310931,64.2012028551135,34.999801938076));
#29917=CARTESIAN_POINT('Ctrl Pts',(18.0542582879001,65.6973951096712,34.8886688200844));
#29918=CARTESIAN_POINT('Ctrl Pts',(18.6904432516101,67.4705602726572,34.7775357020928));
#29919=CARTESIAN_POINT('Ctrl Pts',(20.5251866927185,67.8978022666667,34.6664025841013));
#29920=CARTESIAN_POINT('Ctrl Pts',(21.8792583017954,66.5881052056475,34.5552694661097));
#29921=CARTESIAN_POINT('Ctrl Pts',(21.5133588964881,64.7401489682993,34.4441363481182));
#29922=CARTESIAN_POINT('Ctrl Pts',(19.7623737885107,64.0452590579031,34.3330032301266));
#29923=CARTESIAN_POINT('Ctrl Pts',(18.2288735799674,65.1394244562081,34.2218701121351));
#29924=CARTESIAN_POINT('Ctrl Pts',(18.3163779629365,67.0212227346053,34.1107369941435));
#29925=CARTESIAN_POINT('Ctrl Pts',(19.9447995104512,67.9683576357047,33.9996038761519));
#29926=CARTESIAN_POINT('Ctrl Pts',(21.6237427139031,67.1139742228354,33.8884707581604));
#29927=CARTESIAN_POINT('Ctrl Pts',(21.8165726780916,65.2400377215117,33.7773376401688));
#29928=CARTESIAN_POINT('Ctrl Pts',(20.3468038264876,64.0616486263943,33.6662045221773));
#29929=CARTESIAN_POINT('Ctrl Pts',(18.559626463418,64.6573149925867,33.5550714041857));
#29930=CARTESIAN_POINT('Ctrl Pts',(18.0907356532766,66.4818595294338,33.4439382861942));
#29931=CARTESIAN_POINT('Ctrl Pts',(19.3692787213201,67.865387256979,33.3328051682026));
#29932=CARTESIAN_POINT('Ctrl Pts',(21.2250827284832,67.541639147092,33.221672050211));
#29933=CARTESIAN_POINT('Ctrl Pts',(21.9596428037902,65.8069222109183,33.1105389322195));
#29934=CARTESIAN_POINT('Ctrl Pts',(20.9006606542602,64.248917667052,32.9994058142279));
#29935=CARTESIAN_POINT('Ctrl Pts',(19.0173584243029,64.2935725960923,32.8882726962364));
#29936=CARTESIAN_POINT('Ctrl Pts',(18.0334084408143,65.9000170495854,32.7771395782448));
#29937=CARTESIAN_POINT('Ctrl Pts',(18.8493604565844,67.5979698345543,32.6660064602532));
#29938=CARTESIAN_POINT('Ctrl Pts',(20.7184230712183,67.8333977314765,32.5548733422617));
#29939=CARTESIAN_POINT('Ctrl Pts',(21.9299566142173,66.3908278627113,32.4437402242701));
#29940=CARTESIAN_POINT('Ctrl Pts',(21.3751179015322,64.5905569511623,32.3326071062786));
#29941=CARTESIAN_POINT('Ctrl Pts',(19.5617171612518,64.0802637930451,32.221473988287));
#29942=CARTESIAN_POINT('Ctrl Pts',(18.1494501256381,65.3269887716151,32.1103408702955));
#29943=CARTESIAN_POINT('Ctrl Pts',(18.4308791719737,67.1896801158661,31.9992077523038));
#29944=CARTESIAN_POINT('Ctrl Pts',(20.1484293601129,67.9635293927237,31.8880746343123));
#29945=CARTESIAN_POINT('Ctrl Pts',(21.7301311557542,66.9402792855966,31.7769415163207));
#29946=CARTESIAN_POINT('Ctrl Pts',(21.7283488203504,65.0564485672595,31.6658083983292));
#29947=CARTESIAN_POINT('Ctrl Pts',(20.1447136174153,64.0361932579889,31.5546752803376));
#29948=CARTESIAN_POINT('Ctrl Pts',(18.4286308159493,64.8132911736871,31.4435421623461));
#29949=CARTESIAN_POINT('Ctrl Pts',(18.1507269402148,66.6765117156309,31.3324090443545));
#29950=CARTESIAN_POINT('Ctrl Pts',(19.5653505554741,67.9205621081879,31.221275926363));
#29951=CARTESIAN_POINT('Ctrl Pts',(21.3777824499989,67.4068384667431,31.1101428083714));
#29952=CARTESIAN_POINT('Ctrl Pts',(21.929213617296,65.6055208879127,30.9990096903798));
#29953=CARTESIAN_POINT('Ctrl Pts',(20.7149525489356,64.1652461190112,30.8878765723883));
#29954=CARTESIAN_POINT('Ctrl Pts',(18.8463387675313,64.4042103171995,30.7767434543967));
#29955=CARTESIAN_POINT('Ctrl Pts',(18.033601153746,66.103704042757,30.6656103364052));
#29956=CARTESIAN_POINT('Ctrl Pts',(19.0205891607567,67.7082837466316,30.5544772184136));
#29957=CARTESIAN_POINT('Ctrl Pts',(20.9039725170779,67.7493749281961,30.4433441004221));
#29958=CARTESIAN_POINT('Ctrl Pts',(21.9600046457578,66.1893693207493,30.3322109824305));
#29959=CARTESIAN_POINT('Ctrl Pts',(21.2221633776091,64.4560454574488,30.2210778644389));
#29960=CARTESIAN_POINT('Ctrl Pts',(19.3657500823907,64.1358095609499,30.1099447464474));
#29961=CARTESIAN_POINT('Ctrl Pts',(18.0898272756019,65.5217541280903,29.9988116284558));
#29962=CARTESIAN_POINT('Ctrl Pts',(18.5621697298479,67.3454081407765,29.8876785104642));
#29963=CARTESIAN_POINT('Ctrl Pts',(20.3504710397852,67.9376916682758,29.7765453924727));
#29964=CARTESIAN_POINT('Ctrl Pts',(21.8180074597053,66.7565235141681,29.6654122744811));
#29965=CARTESIAN_POINT('Ctrl Pts',(21.6216318964268,64.8829552634185,29.5542791564896));
#29966=CARTESIAN_POINT('Ctrl Pts',(19.941074994729,64.0317503220406,29.443146038498));
#29967=CARTESIAN_POINT('Ctrl Pts',(18.3144485771209,64.9819649554836,29.3320129205065));
#29968=CARTESIAN_POINT('Ctrl Pts',(18.2305051643892,66.863925331137,29.2208798025149));
#29969=CARTESIAN_POINT('Ctrl Pts',(19.7660730718466,67.9551872399639,29.1097466845233));
#29970=CARTESIAN_POINT('Ctrl Pts',(21.5157401112242,67.2569848313562,28.9986135665318));
#29971=CARTESIAN_POINT('Ctrl Pts',(21.87814214186,65.4083404306503,28.8874804485402));
#29972=CARTESIAN_POINT('Ctrl Pts',(20.5215945613111,64.101206155307,28.7763473305487));
#29973=CARTESIAN_POINT('Ctrl Pts',(18.6876631084887,64.5319227424242,28.6652142125571));
#29974=CARTESIAN_POINT('Ctrl Pts',(18.0548340318536,66.3062814186326,28.5540810945655));
#29975=CARTESIAN_POINT('Ctrl Pts',(19.2022974102536,67.800319285389,28.442947976574));
#29976=CARTESIAN_POINT('Ctrl Pts',(21.0798495960555,67.6466340822816,28.3318148585824));
#29977=CARTESIAN_POINT('Ctrl Pts',(21.9690809290854,65.9858845561824,28.2206817405909));
#29978=CARTESIAN_POINT('Ctrl Pts',(21.0561318935384,64.3380540398472,28.1095486225993));
#29979=CARTESIAN_POINT('Ctrl Pts',(19.1765693800943,64.2113018797919,27.9984155046077));
#29980=CARTESIAN_POINT('Ctrl Pts',(18.0506429798704,65.721636641838,27.8872823866162));
#29981=CARTESIAN_POINT('Ctrl Pts',(18.7088448504754,67.4867405055191,27.7761492686246));
#29982=CARTESIAN_POINT('Ctrl Pts',(20.5487627331737,67.8911209410725,27.665016150633));
#29983=CARTESIAN_POINT('Ctrl Pts',(21.8864313636263,66.5646730574428,27.5538830326415));
#29984=CARTESIAN_POINT('Ctrl Pts',(21.4975637603834,64.7214141665632,27.4427499146499));
#29985=CARTESIAN_POINT('Ctrl Pts',(19.738066861079,64.0483673546206,27.3316167966584));
#29986=CARTESIAN_POINT('Ctrl Pts',(18.2183014781556,65.1615315561838,27.2204836786668));
#29987=CARTESIAN_POINT('Ctrl Pts',(18.3292167132778,67.0420950774451,27.1093505606753));
#29988=CARTESIAN_POINT('Ctrl Pts',(19.9692985660544,67.9688921711125,26.9982174426838));
#29989=CARTESIAN_POINT('Ctrl Pts',(21.6374795950145,67.093681647467,26.8870843246921));
#29990=CARTESIAN_POINT('Ctrl Pts',(21.8069748172614,65.2174906480645,26.7759512067006));
#29991=CARTESIAN_POINT('Ctrl Pts',(20.3226556263046,64.0574829771209,26.664818088709));
#29992=CARTESIAN_POINT('Ctrl Pts',(18.5430291841408,64.6753434014641,26.5536849707175));
#29993=CARTESIAN_POINT('Ctrl Pts',(18.0968800225525,66.5055815646723,26.4425518527259));
#29994=CARTESIAN_POINT('Ctrl Pts',(19.3925406836826,67.8730918158693,26.3314187347344));
#29995=CARTESIAN_POINT('Ctrl Pts',(21.2441729909822,67.5262742434723,26.2202856167428));
#29996=CARTESIAN_POINT('Ctrl Pts',(21.957087271561,65.7825513461355,26.1091524987512));
#29997=CARTESIAN_POINT('Ctrl Pts',(20.8788021098056,64.2378441486145,25.9980193807597));
#29998=CARTESIAN_POINT('Ctrl Pts',(18.9961949733702,64.3059350666609,25.8868862627681));
#29999=CARTESIAN_POINT('Ctrl Pts',(18.0323250495028,65.9244934665604,25.7757531447766));
#30000=CARTESIAN_POINT('Ctrl Pts',(18.8693180936086,67.6121732190418,25.664620026785));
#30001=CARTESIAN_POINT('Ctrl Pts',(20.7412167255774,67.8242990731299,25.5534869087934));
#30002=CARTESIAN_POINT('Ctrl Pts',(21.9346029937715,66.3668134624633,25.4423537908019));
#30003=CARTESIAN_POINT('Ctrl Pts',(21.3576070175663,64.573488384656,25.3312206728103));
#30004=CARTESIAN_POINT('Ctrl Pts',(19.5375919330654,64.0859968791816,25.2200875548188));
#30005=CARTESIAN_POINT('Ctrl Pts',(18.141756289785,65.3498097603869,25.1089544368272));
#30006=CARTESIAN_POINT('Ctrl Pts',(18.4447228010167,67.2096329020469,24.9978213188356));
#30007=CARTESIAN_POINT('Ctrl Pts',(20.1751283187016,67.960491249224,24.8866882008441));
#30008=CARTESIAN_POINT('Ctrl Pts',(21.2151340020224,67.2672324081111,24.8125994555164));
#30009=CARTESIAN_POINT('Ctrl Pts',(21.4735782273626,66.7772536316049,24.7755550828525));
#30010=CARTESIAN_POINT('Ctrl Pts',(21.3677806246587,67.1633123698099,36.0748149723825));
#30011=CARTESIAN_POINT('Ctrl Pts',(21.7545930524415,66.7085123024943,36.0377705997186));
#30012=CARTESIAN_POINT('Ctrl Pts',(22.0318763887585,65.3902531353729,35.9636818543909));
#30013=CARTESIAN_POINT('Ctrl Pts',(20.5876734486638,63.9593792359159,35.8525487363994));
#30014=CARTESIAN_POINT('Ctrl Pts',(18.6053431364634,64.4008976582304,35.7414156184077));
#30015=CARTESIAN_POINT('Ctrl Pts',(17.8996138073842,66.3036680073947,35.6302825004163));
#30016=CARTESIAN_POINT('Ctrl Pts',(19.1161602286543,67.9296622740197,35.5191493824247));
#30017=CARTESIAN_POINT('Ctrl Pts',(21.1416720543637,67.7889759416293,35.4080162644332));
#30018=CARTESIAN_POINT('Ctrl Pts',(22.1222603781053,66.0112381179025,35.2968831464416));
#30019=CARTESIAN_POINT('Ctrl Pts',(21.1604826549332,64.2230694414171,35.18575002845));
#30020=CARTESIAN_POINT('Ctrl Pts',(19.1365804231924,64.0612904121213,35.0746169104584));
#30021=CARTESIAN_POINT('Ctrl Pts',(17.9029163330024,65.6738581646702,34.9634837924669));
#30022=CARTESIAN_POINT('Ctrl Pts',(18.5885844709106,67.5849420865818,34.8523506744753));
#30023=CARTESIAN_POINT('Ctrl Pts',(20.5660362979194,68.0454154381686,34.7412175564838));
#30024=CARTESIAN_POINT('Ctrl Pts',(22.0254291030805,66.6338486827774,34.6300844384922));
#30025=CARTESIAN_POINT('Ctrl Pts',(21.6310696349854,64.6421563535386,34.5189513205007));
#30026=CARTESIAN_POINT('Ctrl Pts',(19.743890957435,63.8932171328852,34.4078182025091));
#30027=CARTESIAN_POINT('Ctrl Pts',(18.0911133967366,65.0724879330689,34.2966850845175));
#30028=CARTESIAN_POINT('Ctrl Pts',(18.1854239679567,67.1006545749571,34.185551966526));
#30029=CARTESIAN_POINT('Ctrl Pts',(19.9405059549666,68.1214586822994,34.0744188485344));
#30030=CARTESIAN_POINT('Ctrl Pts',(21.7500392285148,67.2006203771226,33.9632857305429));
#30031=CARTESIAN_POINT('Ctrl Pts',(21.9578677218307,65.1809270100747,33.8521526125513));
#30032=CARTESIAN_POINT('Ctrl Pts',(20.373778613912,63.910881500246,33.7410194945598));
#30033=CARTESIAN_POINT('Ctrl Pts',(18.4475926074063,64.5528794590469,33.6298863765682));
#30034=CARTESIAN_POINT('Ctrl Pts',(17.9422309484369,66.5193390996755,33.5187532585767));
#30035=CARTESIAN_POINT('Ctrl Pts',(19.3202205186216,68.0104791529674,33.4076201405851));
#30036=CARTESIAN_POINT('Ctrl Pts',(21.3203710259418,67.6615495549417,33.2964870225935));
#30037=CARTESIAN_POINT('Ctrl Pts',(22.1120660010638,65.7919044056951,33.185353904602));
#30038=CARTESIAN_POINT('Ctrl Pts',(20.970715041884,64.1127165352126,33.0742207866104));
#30039=CARTESIAN_POINT('Ctrl Pts',(18.9409274694105,64.1608447743097,32.9630876686188));
#30040=CARTESIAN_POINT('Ctrl Pts',(17.8804447616159,65.8922402644766,32.8519545506273));
#30041=CARTESIAN_POINT('Ctrl Pts',(18.7598624328743,67.7222617059394,32.7408214326357));
#30042=CARTESIAN_POINT('Ctrl Pts',(20.7743028169038,67.9760014465848,32.6296883146442));
#30043=CARTESIAN_POINT('Ctrl Pts',(22.0800707866417,66.4212268886475,32.5185551966526));
#30044=CARTESIAN_POINT('Ctrl Pts',(21.4820761016564,64.4809289028958,32.4074220786611));
#30045=CARTESIAN_POINT('Ctrl Pts',(19.5276270344884,63.9309445752673,32.2962889606694));
#30046=CARTESIAN_POINT('Ctrl Pts',(18.0055122977753,65.2746412095833,32.185155842678));
#30047=CARTESIAN_POINT('Ctrl Pts',(18.3088312084093,67.2822147587319,32.0740227246863));
#30048=CARTESIAN_POINT('Ctrl Pts',(20.159974360862,68.1162548932082,31.9628896066948));
#30049=CARTESIAN_POINT('Ctrl Pts',(21.8647026817244,67.0134152544393,31.8517564887032));
#30050=CARTESIAN_POINT('Ctrl Pts',(21.8627817142903,64.983058087172,31.7406233707117));
#30051=CARTESIAN_POINT('Ctrl Pts',(20.1559696035638,63.8834461849685,31.6294902527201));
#30052=CARTESIAN_POINT('Ctrl Pts',(18.306407972752,64.7209876410282,31.5183571347286));
#30053=CARTESIAN_POINT('Ctrl Pts',(18.0068884244102,66.7291315494549,31.407224016737));
#30054=CARTESIAN_POINT('Ctrl Pts',(19.5315430381553,68.0699455654823,31.2960908987455));
#30055=CARTESIAN_POINT('Ctrl Pts',(21.484947901667,67.5162639277168,31.1849577807539));
#30056=CARTESIAN_POINT('Ctrl Pts',(22.0792699985932,65.5748378637382,31.0738246627623));
#30057=CARTESIAN_POINT('Ctrl Pts',(20.7705623535372,64.0225369210851,30.9626915447707));
#30058=CARTESIAN_POINT('Ctrl Pts',(18.7566057134853,64.2800880204431,30.8515584267792));
#30059=CARTESIAN_POINT('Ctrl Pts',(17.8806524639738,66.1117702585676,30.7404253087876));
#30060=CARTESIAN_POINT('Ctrl Pts',(18.9444094961397,67.8411559568164,30.6292921907961));
#30061=CARTESIAN_POINT('Ctrl Pts',(20.9742845050759,67.8854432561946,30.5181590728045));
#30062=CARTESIAN_POINT('Ctrl Pts',(22.1124559875022,66.2040986771801,30.407025954813));
#30063=CARTESIAN_POINT('Ctrl Pts',(21.3172246047091,64.3359549555647,30.2958928368214));
#30064=CARTESIAN_POINT('Ctrl Pts',(19.316417418231,63.9908107547912,30.1847597188299));
#30065=CARTESIAN_POINT('Ctrl Pts',(17.9412519161361,65.4845556321509,30.0736266008383));
#30066=CARTESIAN_POINT('Ctrl Pts',(18.4503336919285,67.4500554826586,29.9624934828468));
#30067=CARTESIAN_POINT('Ctrl Pts',(20.3777310671394,68.0884074818096,29.8513603648552));
#30068=CARTESIAN_POINT('Ctrl Pts',(21.9594141023544,66.8153667546909,29.7402272468636));
#30069=CARTESIAN_POINT('Ctrl Pts',(21.7477642293072,64.7960702811563,29.6290941288721));
#30070=CARTESIAN_POINT('Ctrl Pts',(19.9364917422682,63.8786576725195,29.5179610108805));
#30071=CARTESIAN_POINT('Ctrl Pts',(18.1833445123661,64.9027810572131,29.4068278928889));
#30072=CARTESIAN_POINT('Ctrl Pts',(18.0928718876097,66.9311224044622,29.2956947748974));
#30073=CARTESIAN_POINT('Ctrl Pts',(19.747877975144,68.1072638785266,29.1845616569058));
#30074=CARTESIAN_POINT('Ctrl Pts',(21.6336360632527,67.3547545098655,29.0734285389143));
#30075=CARTESIAN_POINT('Ctrl Pts',(22.0242261269836,65.3623204911576,28.9622954209227));
#30076=CARTESIAN_POINT('Ctrl Pts',(20.5621647665351,63.9535158577631,28.8511623029311));
#30077=CARTESIAN_POINT('Ctrl Pts',(18.5855880851643,64.4177340601748,28.7400291849396));
#30078=CARTESIAN_POINT('Ctrl Pts',(17.9035368589611,66.3301043280951,28.628896066948));
#30079=CARTESIAN_POINT('Ctrl Pts',(19.1402512154229,67.9403501221627,28.5177629489565));
#30080=CARTESIAN_POINT('Ctrl Pts',(21.1638414989099,67.7747111129913,28.4066298309649));
#30081=CARTESIAN_POINT('Ctrl Pts',(22.1222382342439,65.9847866412596,28.2954967129734));
#30082=CARTESIAN_POINT('Ctrl Pts',(21.1382790071064,64.208786034243,28.1843635949818));
#30083=CARTESIAN_POINT('Ctrl Pts',(19.1125220304568,64.0721749501739,28.0732304769902));
#30084=CARTESIAN_POINT('Ctrl Pts',(17.8990198222922,65.6999852301763,27.9620973589987));
#30085=CARTESIAN_POINT('Ctrl Pts',(18.6084173666064,67.6023808359554,27.8509642410071));
#30086=CARTESIAN_POINT('Ctrl Pts',(20.5914461090282,68.0382144316372,27.7398311230155));
#30087=CARTESIAN_POINT('Ctrl Pts',(22.0331600936403,66.6085939560183,27.6286980050241));
#30088=CARTESIAN_POINT('Ctrl Pts',(21.6140459356233,64.6219643380822,27.5175648870324));
#30089=CARTESIAN_POINT('Ctrl Pts',(19.7176934101476,63.8965671963791,27.4064317690409));
#30090=CARTESIAN_POINT('Ctrl Pts',(18.079718985085,65.0963145478738,27.2952986510493));
#30091=CARTESIAN_POINT('Ctrl Pts',(18.199261330582,67.1231503918422,27.1841655330577));
#30092=CARTESIAN_POINT('Ctrl Pts',(19.9669105743685,68.1220347944658,27.0730324150662));
#30093=CARTESIAN_POINT('Ctrl Pts',(21.7648445795207,67.1787494226676,26.9618992970746));
#30094=CARTESIAN_POINT('Ctrl Pts',(21.9475233287081,65.1566262001724,26.8507661790831));
#30095=CARTESIAN_POINT('Ctrl Pts',(20.3477521398551,63.9063918421381,26.7396330610915));
#30096=CARTESIAN_POINT('Ctrl Pts',(18.4297043732834,64.5723101376224,26.6284999431));
#30097=CARTESIAN_POINT('Ctrl Pts',(17.9488532335904,66.5449062612042,26.5173668251084));
#30098=CARTESIAN_POINT('Ctrl Pts',(19.3452918222943,68.0187829810191,26.4062337071169));
#30099=CARTESIAN_POINT('Ctrl Pts',(21.3409461502948,67.6449895520258,26.2951005891253));
#30100=CARTESIAN_POINT('Ctrl Pts',(22.109311696695,65.7656379479381,26.1839674711337));
#30101=CARTESIAN_POINT('Ctrl Pts',(20.9471563155252,64.1007817061923,26.0728343531422));
#30102=CARTESIAN_POINT('Ctrl Pts',(18.9181179017211,64.1741688115918,25.9617012351506));
#30103=CARTESIAN_POINT('Ctrl Pts',(17.879277102923,65.9186204843926,25.850568117159));
#30104=CARTESIAN_POINT('Ctrl Pts',(18.781372397108,67.7375698454729,25.7394349991675));
#30105=CARTESIAN_POINT('Ctrl Pts',(20.7988693870556,67.9661950844702,25.6283018811759));
#30106=CARTESIAN_POINT('Ctrl Pts',(22.0850785667664,66.3953446216335,25.5171687631844));
#30107=CARTESIAN_POINT('Ctrl Pts',(21.4632032016557,64.4625327242989,25.4060356451928));
#30108=CARTESIAN_POINT('Ctrl Pts',(19.5016253192157,63.9371235872212,25.2949025272012));
#30109=CARTESIAN_POINT('Ctrl Pts',(17.9972200268106,65.299237240249,25.1837694092097));
#30110=CARTESIAN_POINT('Ctrl Pts',(18.3237516103194,67.3037194948181,25.0726362912181));
#30111=CARTESIAN_POINT('Ctrl Pts',(20.1887499941509,68.1129804395273,24.9615031732266));
#30112=CARTESIAN_POINT('Ctrl Pts',(21.3096484764694,67.3657991545403,24.8874144278989));
#30113=CARTESIAN_POINT('Ctrl Pts',(21.5881947811615,66.837709283723,24.850370055235));
#30114=CARTESIAN_POINT('Ctrl Pts',(21.4664903694652,67.2472660865711,36.149629944765));
#30115=CARTESIAN_POINT('Ctrl Pts',(21.8812182065951,66.7596440902318,36.1125855721011));
#30116=CARTESIAN_POINT('Ctrl Pts',(22.1785124765907,65.3462490338972,36.0384968267734));
#30117=CARTESIAN_POINT('Ctrl Pts',(20.6300845598474,63.8121120855864,35.9273637087819));
#30118=CARTESIAN_POINT('Ctrl Pts',(18.5046937921093,64.2854939295697,35.8162305907903));
#30119=CARTESIAN_POINT('Ctrl Pts',(17.7480335164148,66.325583065245,35.7050974727988));
#30120=CARTESIAN_POINT('Ctrl Pts',(19.0523754398465,68.0689217921011,35.5939643548072));
#30121=CARTESIAN_POINT('Ctrl Pts',(21.2240640367527,67.9180824339128,35.4828312368156));
#30122=CARTESIAN_POINT('Ctrl Pts',(22.275419281338,66.0120491483635,35.3716981188241));
#30123=CARTESIAN_POINT('Ctrl Pts',(21.2442321573429,64.0948322381591,35.2605650008325));
#30124=CARTESIAN_POINT('Ctrl Pts',(19.0742693152918,63.9213779691293,35.149431882841));
#30125=CARTESIAN_POINT('Ctrl Pts',(17.7515743781046,65.650321219669,35.0382987648494));
#30126=CARTESIAN_POINT('Ctrl Pts',(18.486725690211,67.6993239005066,34.9271656468578));
#30127=CARTESIAN_POINT('Ctrl Pts',(20.6068859031203,68.1930286096704,34.8160325288663));
#30128=CARTESIAN_POINT('Ctrl Pts',(22.1715999043656,66.6795921599075,34.7048994108747));
#30129=CARTESIAN_POINT('Ctrl Pts',(21.7487803734828,64.5441637387779,34.5937662928832));
#30130=CARTESIAN_POINT('Ctrl Pts',(19.7254081263593,63.7411752078672,34.4826331748916));
#30131=CARTESIAN_POINT('Ctrl Pts',(17.9533532135058,65.0055514099299,34.3715000569001));
#30132=CARTESIAN_POINT('Ctrl Pts',(18.0544699729771,67.1800864153088,34.2603669389085));
#30133=CARTESIAN_POINT('Ctrl Pts',(19.936212399482,68.274559728894,34.1492338209169));
#30134=CARTESIAN_POINT('Ctrl Pts',(21.8763357431267,67.2872665314098,34.0381007029254));
#30135=CARTESIAN_POINT('Ctrl Pts',(22.0991627655698,65.1218162986378,33.9269675849338));
#30136=CARTESIAN_POINT('Ctrl Pts',(20.4007534013364,63.7601143740976,33.8158344669422));
#30137=CARTESIAN_POINT('Ctrl Pts',(18.3355587513947,64.4484439255071,33.7047013489507));
#30138=CARTESIAN_POINT('Ctrl Pts',(17.7937262435972,66.556818669917,33.5935682309591));
#30139=CARTESIAN_POINT('Ctrl Pts',(19.2711623159232,68.1555710489559,33.4824351129676));
#30140=CARTESIAN_POINT('Ctrl Pts',(21.4156593234003,67.7814599627911,33.371301994976));
#30141=CARTESIAN_POINT('Ctrl Pts',(22.2644891983374,65.776886600472,33.2601688769844));
#30142=CARTESIAN_POINT('Ctrl Pts',(21.0407694295078,63.9765154033731,33.1490357589929));
#30143=CARTESIAN_POINT('Ctrl Pts',(18.8644965145181,64.0281169525272,33.0379026410013));
#30144=CARTESIAN_POINT('Ctrl Pts',(17.7274810824176,65.8844634793678,32.9267695230098));
#30145=CARTESIAN_POINT('Ctrl Pts',(18.6703644091643,67.8465535773246,32.8156364050182));
#30146=CARTESIAN_POINT('Ctrl Pts',(20.8301825625893,68.1186051616932,32.7045032870267));
#30147=CARTESIAN_POINT('Ctrl Pts',(22.2301849590661,66.4516259145837,32.5933701690351));
#30148=CARTESIAN_POINT('Ctrl Pts',(21.5890343017806,64.3713008546293,32.4822370510436));
#30149=CARTESIAN_POINT('Ctrl Pts',(19.493536907725,63.7816253574895,32.371103933052));
#30150=CARTESIAN_POINT('Ctrl Pts',(17.8615744699125,65.2222936475516,32.2599708150604));
#30151=CARTESIAN_POINT('Ctrl Pts',(18.1867832448448,67.3747494015975,32.1488376970689));
#30152=CARTESIAN_POINT('Ctrl Pts',(20.1715193616111,68.2689803936927,32.0377045790773));
#30153=CARTESIAN_POINT('Ctrl Pts',(21.9992742076947,67.086551223282,31.9265714610857));
#30154=CARTESIAN_POINT('Ctrl Pts',(21.9972146082301,64.9096676070843,31.8154383430942));
#30155=CARTESIAN_POINT('Ctrl Pts',(20.1672255897123,63.7306991119479,31.7043052251026));
#30156=CARTESIAN_POINT('Ctrl Pts',(18.1841851295548,64.6286841083692,31.5931721071111));
#30157=CARTESIAN_POINT('Ctrl Pts',(17.8630499086056,66.7817513832787,31.4820389891195));
#30158=CARTESIAN_POINT('Ctrl Pts',(19.4977355208365,68.2193290227768,31.3709058711279));
#30159=CARTESIAN_POINT('Ctrl Pts',(21.5921133533351,67.6256893886905,31.2597727531364));
#30160=CARTESIAN_POINT('Ctrl Pts',(22.2293263798905,65.5441548395638,31.1486396351448));
#30161=CARTESIAN_POINT('Ctrl Pts',(20.8261721581388,63.879827723159,31.0375065171533));
#30162=CARTESIAN_POINT('Ctrl Pts',(18.6668726594392,64.1559657236867,30.9263733991617));
#30163=CARTESIAN_POINT('Ctrl Pts',(17.7277037742016,66.1198364743782,30.8152402811701));
#30164=CARTESIAN_POINT('Ctrl Pts',(18.8682298315227,67.9740281670011,30.7041071631786));
#30165=CARTESIAN_POINT('Ctrl Pts',(21.0445964930739,68.021511584193,30.592974045187));
#30166=CARTESIAN_POINT('Ctrl Pts',(22.2649073292466,66.2188280336109,30.4818409271955));
#30167=CARTESIAN_POINT('Ctrl Pts',(21.412285831809,64.2158644536806,30.3707078092039));
#30168=CARTESIAN_POINT('Ctrl Pts',(19.2670847540712,63.8458119486327,30.2595746912124));
#30169=CARTESIAN_POINT('Ctrl Pts',(17.7926765566704,65.4473571362115,30.1484415732208));
#30170=CARTESIAN_POINT('Ctrl Pts',(18.338497654009,67.5547028245408,30.0373084552292));
#30171=CARTESIAN_POINT('Ctrl Pts',(20.4049910944936,68.2391232953435,29.9261753372377));
#30172=CARTESIAN_POINT('Ctrl Pts',(22.1008207450036,66.8742099952136,29.8150422192461));
#30173=CARTESIAN_POINT('Ctrl Pts',(21.8738965621875,64.7091852988942,29.7039091012546));
#30174=CARTESIAN_POINT('Ctrl Pts',(19.9319084898074,63.7255650229983,29.592775983263));
#30175=CARTESIAN_POINT('Ctrl Pts',(18.0522404476114,64.8235971589427,29.4816428652714));
#30176=CARTESIAN_POINT('Ctrl Pts',(17.9552386108303,66.9983194777874,29.3705097472799));
#30177=CARTESIAN_POINT('Ctrl Pts',(19.7296828784414,68.2593405170892,29.2593766292883));
#30178=CARTESIAN_POINT('Ctrl Pts',(21.7515320152811,67.4525241883749,29.1482435112968));
#30179=CARTESIAN_POINT('Ctrl Pts',(22.1703101121073,65.3163005516648,29.0371103933052));
#30180=CARTESIAN_POINT('Ctrl Pts',(20.6027349717591,63.8058255602192,28.9259772753137));
#30181=CARTESIAN_POINT('Ctrl Pts',(18.48351306184,64.3035453779253,28.8148441573221));
#30182=CARTESIAN_POINT('Ctrl Pts',(17.7522396860685,66.3539272375576,28.7037110393305));
#30183=CARTESIAN_POINT('Ctrl Pts',(19.0782050205922,68.0803809589363,28.592577921339));
#30184=CARTESIAN_POINT('Ctrl Pts',(21.2478334017644,67.902788143701,28.4814448033474));
#30185=CARTESIAN_POINT('Ctrl Pts',(22.2753955394023,65.9836887263368,28.3703116853558));
#30186=CARTESIAN_POINT('Ctrl Pts',(21.2204261206745,64.0795180286389,28.2591785673643));
#30187=CARTESIAN_POINT('Ctrl Pts',(19.0484746808193,63.9330480205558,28.1480454493727));
#30188=CARTESIAN_POINT('Ctrl Pts',(17.7473966647141,65.6783338185146,28.0369123313811));
#30189=CARTESIAN_POINT('Ctrl Pts',(18.5079898827373,67.7180211663916,27.9257792133896));
#30190=CARTESIAN_POINT('Ctrl Pts',(20.6341294848828,68.1853079222018,27.814646095398));
#30191=CARTESIAN_POINT('Ctrl Pts',(22.1798888236542,66.6525148545939,27.7035129774065));
#30192=CARTESIAN_POINT('Ctrl Pts',(21.7305281108632,64.5225145096011,27.5923798594149));
#30193=CARTESIAN_POINT('Ctrl Pts',(19.6973199592161,63.7447670381374,27.4812467414234));
#30194=CARTESIAN_POINT('Ctrl Pts',(17.9411364920144,65.0310975395638,27.3701136234318));
#30195=CARTESIAN_POINT('Ctrl Pts',(18.0693059478863,67.2042057062393,27.2589805054402));
#30196=CARTESIAN_POINT('Ctrl Pts',(19.9645225826826,68.2751774178192,27.1478473874487));
#30197=CARTESIAN_POINT('Ctrl Pts',(21.8922095640269,67.2638171978682,27.0367142694571));
#30198=CARTESIAN_POINT('Ctrl Pts',(22.0880718401547,65.0957617522804,26.9255811514656));
#30199=CARTESIAN_POINT('Ctrl Pts',(20.3728486534058,63.7553007071551,26.814448033474));
#30200=CARTESIAN_POINT('Ctrl Pts',(18.3163795624261,64.4692768737807,26.7033149154825));
#30201=CARTESIAN_POINT('Ctrl Pts',(17.8008264446283,66.5842309577361,26.5921817974909));
#30202=CARTESIAN_POINT('Ctrl Pts',(19.2980429609061,68.164474146169,26.4810486794993));
#30203=CARTESIAN_POINT('Ctrl Pts',(21.4377193096073,67.7637048605792,26.3699155615078));
#30204=CARTESIAN_POINT('Ctrl Pts',(22.2615361218289,65.7487245497409,26.2587824435162));
#30205=CARTESIAN_POINT('Ctrl Pts',(21.0155105212449,63.9637192637702,26.1476493255247));
#30206=CARTESIAN_POINT('Ctrl Pts',(18.8400408300719,64.0424025565226,26.0365162075331));
#30207=CARTESIAN_POINT('Ctrl Pts',(17.7262291563432,65.9127475022248,25.9253830895415));
#30208=CARTESIAN_POINT('Ctrl Pts',(18.6934267006075,67.8629664719039,25.81424997155));
#30209=CARTESIAN_POINT('Ctrl Pts',(20.8565220485339,68.1080910958107,25.7031168535584));
#30210=CARTESIAN_POINT('Ctrl Pts',(22.2355541397614,66.4238757808037,25.5919837355669));
#30211=CARTESIAN_POINT('Ctrl Pts',(21.5687993857451,64.3515770639418,25.4808506175753));
#30212=CARTESIAN_POINT('Ctrl Pts',(19.465658705366,63.7882502952606,25.3697174995837));
#30213=CARTESIAN_POINT('Ctrl Pts',(17.8526837638362,65.2486647201112,25.2585843815922));
#30214=CARTESIAN_POINT('Ctrl Pts',(18.2027804196222,67.3978060875893,25.1474512636006));
#30215=CARTESIAN_POINT('Ctrl Pts',(20.2023716696001,68.2654696298307,25.0363181456091));
#30216=CARTESIAN_POINT('Ctrl Pts',(21.4041629509165,67.4643659009696,24.9622294002814));
#30217=CARTESIAN_POINT('Ctrl Pts',(21.7028113349605,66.8981649358412,24.9251850276175));
#30218=CARTESIAN_POINT('Ctrl Pts',(21.5652001142716,67.3312198033323,36.2244449171475));
#30219=CARTESIAN_POINT('Ctrl Pts',(22.0078433607486,66.8107758779692,36.1874005444836));
#30220=CARTESIAN_POINT('Ctrl Pts',(22.3251485644228,65.3022449324216,36.1133117991559));
#30221=CARTESIAN_POINT('Ctrl Pts',(20.672495671031,63.6648449352568,36.0021786811644));
#30222=CARTESIAN_POINT('Ctrl Pts',(18.4040444477551,64.1700902009091,35.8910455631728));
#30223=CARTESIAN_POINT('Ctrl Pts',(17.5964532254454,66.3474981230952,35.7799124451812));
#30224=CARTESIAN_POINT('Ctrl Pts',(18.9885906510386,68.2081813101826,35.6687793271897));
#30225=CARTESIAN_POINT('Ctrl Pts',(21.3064560191417,68.0471889261963,35.5576462091981));
#30226=CARTESIAN_POINT('Ctrl Pts',(22.4285781845706,66.0128601788243,35.4465130912066));
#30227=CARTESIAN_POINT('Ctrl Pts',(21.3279816597525,63.9665950349013,35.335379973215));
#30228=CARTESIAN_POINT('Ctrl Pts',(19.0119582073911,63.7814655261371,35.2242468552234));
#30229=CARTESIAN_POINT('Ctrl Pts',(17.6002324232069,65.626784274668,35.1131137372319));
#30230=CARTESIAN_POINT('Ctrl Pts',(18.3848669095114,67.8137057144312,35.0019806192403));
#30231=CARTESIAN_POINT('Ctrl Pts',(20.6477355083213,68.3406417811724,34.8908475012488));
#30232=CARTESIAN_POINT('Ctrl Pts',(22.3177707056507,66.7253356370374,34.7797143832572));
#30233=CARTESIAN_POINT('Ctrl Pts',(21.8664911119801,64.4461711240172,34.6685812652656));
#30234=CARTESIAN_POINT('Ctrl Pts',(19.7069252952836,63.5891332828492,34.5574481472741));
#30235=CARTESIAN_POINT('Ctrl Pts',(17.8155930302749,64.9386148867908,34.4463150292825));
#30236=CARTESIAN_POINT('Ctrl Pts',(17.9235159779974,67.2595182556605,34.335181911291));
#30237=CARTESIAN_POINT('Ctrl Pts',(19.9319188439973,68.4276607754887,34.2240487932994));
#30238=CARTESIAN_POINT('Ctrl Pts',(22.0026322577385,67.3739126856969,34.1129156753079));
#30239=CARTESIAN_POINT('Ctrl Pts',(22.2404578093089,65.0627055872007,34.0017825573163));
#30240=CARTESIAN_POINT('Ctrl Pts',(20.4277281887608,63.6093472479493,33.8906494393247));
#30241=CARTESIAN_POINT('Ctrl Pts',(18.223524895383,64.3440083919673,33.7795163213331));
#30242=CARTESIAN_POINT('Ctrl Pts',(17.6452215387575,66.5942982401586,33.6683832033416));
#30243=CARTESIAN_POINT('Ctrl Pts',(19.2221041132247,68.3006629449443,33.55725008535));
#30244=CARTESIAN_POINT('Ctrl Pts',(21.5109476208589,67.9013703706408,33.4461169673585));
#30245=CARTESIAN_POINT('Ctrl Pts',(22.416912395611,65.7618687952487,33.3349838493669));
#30246=CARTESIAN_POINT('Ctrl Pts',(21.1108238171316,63.8403142715337,33.2238507313754));
#30247=CARTESIAN_POINT('Ctrl Pts',(18.7880655596257,63.8953891307446,33.1127176133838));
#30248=CARTESIAN_POINT('Ctrl Pts',(17.5745174032192,65.8766866942591,33.0015844953923));
#30249=CARTESIAN_POINT('Ctrl Pts',(18.5808663854542,67.9708454487097,32.8904513774007));
#30250=CARTESIAN_POINT('Ctrl Pts',(20.8860623082748,68.2612088768015,32.7793182594092));
#30251=CARTESIAN_POINT('Ctrl Pts',(22.3802991314904,66.4820249405198,32.6681851414175));
#30252=CARTESIAN_POINT('Ctrl Pts',(21.6959925019048,64.261672806363,32.5570520234261));
#30253=CARTESIAN_POINT('Ctrl Pts',(19.4594467809617,63.6323061397115,32.4459189054344));
#30254=CARTESIAN_POINT('Ctrl Pts',(17.7176366420497,65.1699460855199,32.3347857874429));
#30255=CARTESIAN_POINT('Ctrl Pts',(18.0647352812803,67.4672840444633,32.2236526694513));
#30256=CARTESIAN_POINT('Ctrl Pts',(20.1830643623602,68.4217058941771,32.1125195514598));
#30257=CARTESIAN_POINT('Ctrl Pts',(22.133845733665,67.1596871921246,32.0013864334682));
#30258=CARTESIAN_POINT('Ctrl Pts',(22.1316475021699,64.8362771269967,31.8902533154767));
#30259=CARTESIAN_POINT('Ctrl Pts',(20.1784815758609,63.5779520389273,31.7791201974851));
#30260=CARTESIAN_POINT('Ctrl Pts',(18.0619622863575,64.5363805757104,31.6679870794936));
#30261=CARTESIAN_POINT('Ctrl Pts',(17.719211392801,66.8343712171026,31.556853961502));
#30262=CARTESIAN_POINT('Ctrl Pts',(19.4639280035177,68.3687124800713,31.4457208435104));
#30263=CARTESIAN_POINT('Ctrl Pts',(21.6992788050032,67.7351148496642,31.3345877255189));
#30264=CARTESIAN_POINT('Ctrl Pts',(22.3793827611878,65.5134718153893,31.2234546075273));
#30265=CARTESIAN_POINT('Ctrl Pts',(20.8817819627404,63.737118525233,31.1123214895358));
#30266=CARTESIAN_POINT('Ctrl Pts',(18.5771396053932,64.0318434269302,31.0011883715442));
#30267=CARTESIAN_POINT('Ctrl Pts',(17.5747550844295,66.1279026901889,30.8900552535526));
#30268=CARTESIAN_POINT('Ctrl Pts',(18.7920501669056,68.1069003771858,30.7789221355611));
#30269=CARTESIAN_POINT('Ctrl Pts',(21.1149084810719,68.1575799121915,30.6677890175695));
#30270=CARTESIAN_POINT('Ctrl Pts',(22.4173586709909,66.2335573900417,30.556655899578));
#30271=CARTESIAN_POINT('Ctrl Pts',(21.507347058909,64.0957739517965,30.4455227815864));
#30272=CARTESIAN_POINT('Ctrl Pts',(19.2177520899114,63.700813142474,30.3343896635948));
#30273=CARTESIAN_POINT('Ctrl Pts',(17.6441011972046,65.4101586402722,30.2232565456033));
#30274=CARTESIAN_POINT('Ctrl Pts',(18.2266616160895,67.6593501664229,30.1121234276117));
#30275=CARTESIAN_POINT('Ctrl Pts',(20.4322511218479,68.3898391088773,30.0009903096202));
#30276=CARTESIAN_POINT('Ctrl Pts',(22.2422273876527,66.9330532357364,29.8898571916286));
#30277=CARTESIAN_POINT('Ctrl Pts',(22.0000288950678,64.622300316632,29.778724073637));
#30278=CARTESIAN_POINT('Ctrl Pts',(19.9273252373466,63.5724723734772,29.6675909556455));
#30279=CARTESIAN_POINT('Ctrl Pts',(17.9211363828566,64.7444132606722,29.5564578376539));
#30280=CARTESIAN_POINT('Ctrl Pts',(17.8176053340508,67.0655165511127,29.4453247196624));
#30281=CARTESIAN_POINT('Ctrl Pts',(19.7114877817388,68.4114171556518,29.3341916016708));
#30282=CARTESIAN_POINT('Ctrl Pts',(21.8694279673096,67.5502938668842,29.2230584836792));
#30283=CARTESIAN_POINT('Ctrl Pts',(22.316394097231,65.2702806121721,29.1119253656877));
#30284=CARTESIAN_POINT('Ctrl Pts',(20.6433051769832,63.6581352626753,29.0007922476961));
#30285=CARTESIAN_POINT('Ctrl Pts',(18.3814380385156,64.1893566956759,28.8896591297046));
#30286=CARTESIAN_POINT('Ctrl Pts',(17.600942513176,66.37775014702,28.778526011713));
#30287=CARTESIAN_POINT('Ctrl Pts',(19.0161588257614,68.2204117957101,28.6673928937215));
#30288=CARTESIAN_POINT('Ctrl Pts',(21.3318253046188,68.0308651744107,28.5562597757299));
#30289=CARTESIAN_POINT('Ctrl Pts',(22.4285528445608,65.982590811414,28.4451266577383));
#30290=CARTESIAN_POINT('Ctrl Pts',(21.3025732342425,63.9502500230349,28.3339935397468));
#30291=CARTESIAN_POINT('Ctrl Pts',(18.9844273311818,63.7939210909379,28.2228604217552));
#30292=CARTESIAN_POINT('Ctrl Pts',(17.595773507136,65.6566824068527,28.1117273037637));
#30293=CARTESIAN_POINT('Ctrl Pts',(18.4075623988682,67.833661496828,28.0005941857721));
#30294=CARTESIAN_POINT('Ctrl Pts',(20.6768128607374,68.3324014127664,27.8894610677805));
#30295=CARTESIAN_POINT('Ctrl Pts',(22.3266175536682,66.6964357531696,27.778327949789));
#30296=CARTESIAN_POINT('Ctrl Pts',(21.8470102861031,64.4230646811199,27.6671948317974));
#30297=CARTESIAN_POINT('Ctrl Pts',(19.6769465082846,63.592966879896,27.5560617138059));
#30298=CARTESIAN_POINT('Ctrl Pts',(17.8025539989437,64.9658805312536,27.4449285958143));
#30299=CARTESIAN_POINT('Ctrl Pts',(17.9393505651906,67.2852610206366,27.3337954778227));
#30300=CARTESIAN_POINT('Ctrl Pts',(19.9621345909966,68.4283200411723,27.2226623598312));
#30301=CARTESIAN_POINT('Ctrl Pts',(22.0195745485331,67.3488849730689,27.1115292418396));
#30302=CARTESIAN_POINT('Ctrl Pts',(22.2286203516014,65.0348973043881,27.0003961238481));
#30303=CARTESIAN_POINT('Ctrl Pts',(20.3979451669564,63.6042095721724,26.8892630058565));
#30304=CARTESIAN_POINT('Ctrl Pts',(18.2030547515686,64.366243609939,26.7781298878649));
#30305=CARTESIAN_POINT('Ctrl Pts',(17.6527996556662,66.6235556542679,26.6669967698734));
#30306=CARTESIAN_POINT('Ctrl Pts',(19.2507940995179,68.310165311319,26.5558636518818));
#30307=CARTESIAN_POINT('Ctrl Pts',(21.5344924689199,67.8824201691326,26.4447305338903));
#30308=CARTESIAN_POINT('Ctrl Pts',(22.4137605469628,65.7318111515436,26.3335974158987));
#30309=CARTESIAN_POINT('Ctrl Pts',(21.0838647269646,63.8266568213479,26.2224642979072));
#30310=CARTESIAN_POINT('Ctrl Pts',(18.7619637584228,63.9106363014535,26.1113311799156));
#30311=CARTESIAN_POINT('Ctrl Pts',(17.5731812097634,65.906874520057,26.000198061924));
#30312=CARTESIAN_POINT('Ctrl Pts',(18.605481004107,67.988363098335,25.8890649439325));
#30313=CARTESIAN_POINT('Ctrl Pts',(20.9141747100121,68.249987107151,25.7779318259409));
#30314=CARTESIAN_POINT('Ctrl Pts',(22.3860297127563,66.4524069399739,25.6667987079494));
#30315=CARTESIAN_POINT('Ctrl Pts',(21.6743955698345,64.2406214035846,25.5556655899578));
#30316=CARTESIAN_POINT('Ctrl Pts',(19.4296920915163,63.6393770033003,25.4445324719662));
#30317=CARTESIAN_POINT('Ctrl Pts',(17.7081475008618,65.1980921999731,25.3333993539747));
#30318=CARTESIAN_POINT('Ctrl Pts',(18.081809228925,67.4918926803607,25.2222662359831));
#30319=CARTESIAN_POINT('Ctrl Pts',(20.2159933450493,68.4179588201339,25.1111331179916));
#30320=CARTESIAN_POINT('Ctrl Pts',(21.4986774253635,67.5629326473988,25.0370443726639));
#30321=CARTESIAN_POINT('Ctrl Pts',(21.8174278887594,66.9586205879593,25.));
#30322=CARTESIAN_POINT('Ctrl Pts',(21.2690708798523,67.0793586530486,36.));
#30323=CARTESIAN_POINT('Ctrl Pts',(21.3144000771637,67.0370713228889,36.));
#30324=CARTESIAN_POINT('Ctrl Pts',(21.3569992688451,66.9922148769181,36.));
#30325=CARTESIAN_POINT('Ctrl Pts',(21.3968699348127,66.9451343396547,36.));
#30326=CARTESIAN_POINT('Ctrl Pts',(21.4393722087531,66.8949463168699,36.));
#30327=CARTESIAN_POINT('Ctrl Pts',(21.4787746097791,66.8422306840625,36.));
#30328=CARTESIAN_POINT('Ctrl Pts',(21.5150500980415,66.7873506773072,36.));
#30329=CARTESIAN_POINT('Ctrl Pts',(21.5467911502712,66.7393306713963,36.));
#30330=CARTESIAN_POINT('Ctrl Pts',(21.5761379164984,66.6896523410759,36.));
#30331=CARTESIAN_POINT('Ctrl Pts',(21.6030493891106,66.6385314719273,36.));
#30332=CARTESIAN_POINT('Ctrl Pts',(21.6165496501045,66.612886458528,36.));
#30333=CARTESIAN_POINT('Ctrl Pts',(21.6294366912151,66.5868780640734,36.));
#30334=CARTESIAN_POINT('Ctrl Pts',(21.6417029941218,66.5605316893449,36.));
#30335=CARTESIAN_POINT('Ctrl Pts',(21.647311956908,66.5484843889866,36.));
#30336=CARTESIAN_POINT('Ctrl Pts',(21.6527917063131,66.5363647353609,36.));
#30337=CARTESIAN_POINT('Ctrl Pts',(21.6581330108966,66.5241951160997,36.));
#30338=CARTESIAN_POINT('Ctrl Pts',(21.6850519415314,66.462863070413,36.));
#30339=CARTESIAN_POINT('Ctrl Pts',(21.7085097094311,66.4001555622147,36.));
#30340=CARTESIAN_POINT('Ctrl Pts',(21.7284828098912,66.3364303588019,36.));
#30341=CARTESIAN_POINT('Ctrl Pts',(21.7488102273524,66.2715746887893,36.));
#30342=CARTESIAN_POINT('Ctrl Pts',(21.7655288042216,66.20566405463,36.));
#30343=CARTESIAN_POINT('Ctrl Pts',(21.7785744463911,66.1390390910945,36.));
#30344=CARTESIAN_POINT('Ctrl Pts',(21.7894856788381,66.0833147001856,36.));
#30345=CARTESIAN_POINT('Ctrl Pts',(21.7978269670469,66.0270896613916,36.));
#30346=CARTESIAN_POINT('Ctrl Pts',(21.8035359856737,65.970550992101,36.));
#30347=CARTESIAN_POINT('Ctrl Pts',(21.8061656064956,65.9445088171278,36.));
#30348=CARTESIAN_POINT('Ctrl Pts',(21.8082364301197,65.9183999892448,36.));
#30349=CARTESIAN_POINT('Ctrl Pts',(21.8097405642396,65.8922423831419,36.));
#30350=CARTESIAN_POINT('Ctrl Pts',(21.8103979291679,65.8808104950978,36.));
#30351=CARTESIAN_POINT('Ctrl Pts',(21.8109469376435,65.8693694952185,36.));
#30352=CARTESIAN_POINT('Ctrl Pts',(21.8113865961963,65.8579350105965,36.));
#30353=CARTESIAN_POINT('Ctrl Pts',(21.8140829654057,65.7878087909138,36.));
#30354=CARTESIAN_POINT('Ctrl Pts',(21.8126785983873,65.7177962634573,36.));
#30355=CARTESIAN_POINT('Ctrl Pts',(21.8071188655741,65.6482582300993,36.));
#30356=CARTESIAN_POINT('Ctrl Pts',(21.8021493024575,65.5861017097425,36.));
#30357=CARTESIAN_POINT('Ctrl Pts',(21.7938593908609,65.5243233307745,36.));
#30358=CARTESIAN_POINT('Ctrl Pts',(21.7821770073433,65.4631686326352,36.));
#30359=CARTESIAN_POINT('Ctrl Pts',(21.7694465551382,65.3965275263397,36.));
#30360=CARTESIAN_POINT('Ctrl Pts',(21.7526887129988,65.3306261926924,36.));
#30361=CARTESIAN_POINT('Ctrl Pts',(21.7321487118934,65.2656782084348,36.));
#30362=CARTESIAN_POINT('Ctrl Pts',(21.7242193534609,65.2406053837546,36.));
#30363=CARTESIAN_POINT('Ctrl Pts',(21.7157257837476,65.2156746844024,36.));
#30364=CARTESIAN_POINT('Ctrl Pts',(21.7066801015395,65.1908987184666,36.));
#30365=CARTESIAN_POINT('Ctrl Pts',(21.7027127271974,65.1800321492803,36.));
#30366=CARTESIAN_POINT('Ctrl Pts',(21.698639247911,65.1691959127051,36.));
#30367=CARTESIAN_POINT('Ctrl Pts',(21.6944657697982,65.1584036090012,36.));
#30368=CARTESIAN_POINT('Ctrl Pts',(21.6692429532713,65.0931792831816,36.));
#30369=CARTESIAN_POINT('Ctrl Pts',(21.6403293178684,65.0294403704392,36.));
#30370=CARTESIAN_POINT('Ctrl Pts',(21.6080375203115,64.9674056751725,36.));
#30371=CARTESIAN_POINT('Ctrl Pts',(21.5749977153262,64.903934007783,36.));
#30372=CARTESIAN_POINT('Ctrl Pts',(21.5384211298212,64.8422456059961,36.));
#30373=CARTESIAN_POINT('Ctrl Pts',(21.4985865170694,64.7825785480101,36.));
#30374=CARTESIAN_POINT('Ctrl Pts',(21.4680938596675,64.7369045215376,36.));
#30375=CARTESIAN_POINT('Ctrl Pts',(21.4356909069961,64.6924148931467,36.));
#30376=CARTESIAN_POINT('Ctrl Pts',(21.401483143624,64.6492225546256,36.));
#30377=CARTESIAN_POINT('Ctrl Pts',(21.3801865973203,64.6223325288946,36.));
#30378=CARTESIAN_POINT('Ctrl Pts',(21.3581902064885,64.5959454384605,36.));
#30379=CARTESIAN_POINT('Ctrl Pts',(21.3355165165973,64.570090213464,36.));
#30380=CARTESIAN_POINT('Ctrl Pts',(21.3228384297211,64.5556331581599,36.));
#30381=CARTESIAN_POINT('Ctrl Pts',(21.3099441169479,64.5413378602927,36.));
#30382=CARTESIAN_POINT('Ctrl Pts',(21.2968612031401,64.527234782426,36.));
#30383=CARTESIAN_POINT('Ctrl Pts',(21.2459899661476,64.4723967679729,36.));
#30384=CARTESIAN_POINT('Ctrl Pts',(21.192222187541,64.42040369654,36.));
#30385=CARTESIAN_POINT('Ctrl Pts',(21.1358428134485,64.3715194870934,36.));
#30386=CARTESIAN_POINT('Ctrl Pts',(21.0936832442526,64.334964678816,36.));
#30387=CARTESIAN_POINT('Ctrl Pts',(21.0500621658713,64.3001484832718,36.));
#30388=CARTESIAN_POINT('Ctrl Pts',(21.0050823390709,64.2671910015265,36.));
#30389=CARTESIAN_POINT('Ctrl Pts',(20.9910186946901,64.2568863308347,36.));
#30390=CARTESIAN_POINT('Ctrl Pts',(20.9768221267921,64.2467634444957,36.));
#30391=CARTESIAN_POINT('Ctrl Pts',(20.9624955349648,64.2368262403725,36.));
#30392=CARTESIAN_POINT('Ctrl Pts',(20.9487061818225,64.2272616755022,36.));
#30393=CARTESIAN_POINT('Ctrl Pts',(20.9348034145042,64.2178740747608,36.));
#30394=CARTESIAN_POINT('Ctrl Pts',(20.9207951922747,64.2086696546068,36.));
#30395=CARTESIAN_POINT('Ctrl Pts',(20.8578415028037,64.1673045050084,36.));
#30396=CARTESIAN_POINT('Ctrl Pts',(20.7927303594474,64.129615031017,36.));
#30397=CARTESIAN_POINT('Ctrl Pts',(20.7257230462104,64.0958803998092,36.));
#30398=CARTESIAN_POINT('Ctrl Pts',(20.674495644503,64.0700901178109,36.));
#30399=CARTESIAN_POINT('Ctrl Pts',(20.6221590194026,64.046611719858,36.));
#30400=CARTESIAN_POINT('Ctrl Pts',(20.5688160527906,64.0255852000049,36.));
#30401=CARTESIAN_POINT('Ctrl Pts',(20.5563688085073,64.0206787944249,36.));
#30402=CARTESIAN_POINT('Ctrl Pts',(20.5438667254187,64.0159059590366,36.));
#30403=CARTESIAN_POINT('Ctrl Pts',(20.5313117419429,64.0112661051077,36.));
#30404=CARTESIAN_POINT('Ctrl Pts',(18.332682423241,65.9986976781594,34.8714803633902));
#30405=CARTESIAN_POINT('Ctrl Pts',(18.3319481375098,65.9132137662013,34.8772098489549));
#30406=CARTESIAN_POINT('Ctrl Pts',(18.3379547564459,65.8278333817693,34.8829393345197));
#30407=CARTESIAN_POINT('Ctrl Pts',(18.3510613223839,65.7435572610759,34.8886688200844));
#30408=CARTESIAN_POINT('Ctrl Pts',(18.4358027022978,65.198664358152,34.9257131927483));
#30409=CARTESIAN_POINT('Ctrl Pts',(18.8173471166954,64.6999336066327,34.9627575654121));
#30410=CARTESIAN_POINT('Ctrl Pts',(19.321092927466,64.4755855291333,34.999801938076));
#30411=CARTESIAN_POINT('Ctrl Pts',(19.8248387382366,64.251237451634,35.0368463107398));
#30412=CARTESIAN_POINT('Ctrl Pts',(20.4507859453801,64.3012720481544,35.0738906834037));
#30413=CARTESIAN_POINT('Ctrl Pts',(20.9124876026766,64.6028094202091,35.1109350560675));
#30414=CARTESIAN_POINT('Ctrl Pts',(21.3741892599732,64.9043467922638,35.1479794287314));
#30415=CARTESIAN_POINT('Ctrl Pts',(21.671645367423,65.4573869398528,35.1850238013952));
#30416=CARTESIAN_POINT('Ctrl Pts',(21.6687365206648,66.0088140739646,35.2220681740591));
#30417=CARTESIAN_POINT('Ctrl Pts',(21.6658276739067,66.5602412080764,35.2591125467229));
#30418=CARTESIAN_POINT('Ctrl Pts',(21.3625538729407,67.1100553287111,35.2961569193868));
#30419=CARTESIAN_POINT('Ctrl Pts',(20.8976944633723,67.4067179401272,35.3332012920506));
#30420=CARTESIAN_POINT('Ctrl Pts',(20.4328350538039,67.7033805515432,35.3702456647145));
#30421=CARTESIAN_POINT('Ctrl Pts',(19.806390035633,67.7468916537407,35.4072900373783));
#30422=CARTESIAN_POINT('Ctrl Pts',(19.3050423733628,67.5172055704405,35.4443344100422));
#30423=CARTESIAN_POINT('Ctrl Pts',(18.8036947110926,67.2875194871403,35.4813787827061));
#30424=CARTESIAN_POINT('Ctrl Pts',(18.4274444047231,66.7846362183425,35.5184231553699));
#30425=CARTESIAN_POINT('Ctrl Pts',(18.3484523152824,66.2389526568346,35.5554675280338));
#30426=CARTESIAN_POINT('Ctrl Pts',(18.337070583666,66.1603267603867,35.5608051398193));
#30427=CARTESIAN_POINT('Ctrl Pts',(18.3318602470798,66.0808122845869,35.5661427516047));
#30428=CARTESIAN_POINT('Ctrl Pts',(18.3325226254757,66.0012132166996,35.5714803633902));
#30429=CARTESIAN_POINT('Ctrl Pts',(19.4698297828115,64.0148256743282,36.));
#30430=CARTESIAN_POINT('Ctrl Pts',(18.809740437582,64.1911123142462,35.9629556273362));
#30431=CARTESIAN_POINT('Ctrl Pts',(17.6907270524739,65.2513727719513,35.8888668820085));
#30432=CARTESIAN_POINT('Ctrl Pts',(18.1186749695233,67.5381215598298,35.7777337640169));
#30433=CARTESIAN_POINT('Ctrl Pts',(20.2718170903172,68.4128312567252,35.6666006460253));
#30434=CARTESIAN_POINT('Ctrl Pts',(22.1745315590613,67.0812974610511,35.5554675280338));
#30435=CARTESIAN_POINT('Ctrl Pts',(22.0878552063855,64.7590834656903,35.4443344100422));
#30436=CARTESIAN_POINT('Ctrl Pts',(20.0898773670193,63.5731233891133,35.3332012920506));
#30437=CARTESIAN_POINT('Ctrl Pts',(18.0098479899297,64.6080763840108,35.2220681740591));
#30438=CARTESIAN_POINT('Ctrl Pts',(17.7511798490307,66.91710303298,35.1109350560675));
#30439=CARTESIAN_POINT('Ctrl Pts',(19.5507726973617,68.3866954932114,34.999801938076));
#30440=CARTESIAN_POINT('Ctrl Pts',(21.761489833587,67.6719231014153,34.8886688200844));
#30441=CARTESIAN_POINT('Ctrl Pts',(22.3600352949887,65.4269244270303,34.7775357020928));
#30442=CARTESIAN_POINT('Ctrl Pts',(20.7985769670495,63.7064353263736,34.6664025841013));
#30443=CARTESIAN_POINT('Ctrl Pts',(18.5062328763905,64.0851027489721,34.5552694661098));
#30444=CARTESIAN_POINT('Ctrl Pts',(17.5810415914568,66.2163615818994,34.4441363481181));
#30445=CARTESIAN_POINT('Ctrl Pts',(18.869777083907,68.1495967375546,34.3330032301266));
#30446=CARTESIAN_POINT('Ctrl Pts',(21.1929366566675,68.1154368741692,34.221870112135));
#30447=CARTESIAN_POINT('Ctrl Pts',(22.4242738572048,66.1451456586872,34.1107369941435));
#30448=CARTESIAN_POINT('Ctrl Pts',(21.4368201000595,64.0420115549533,33.9996038761519));
#30449=CARTESIAN_POINT('Ctrl Pts',(19.1343320873597,63.7309054758618,33.8884707581604));
#30450=CARTESIAN_POINT('Ctrl Pts',(17.6241373942269,65.4965640490266,33.7773376401688));
#30451=CARTESIAN_POINT('Ctrl Pts',(18.2884256842001,67.7229870029778,33.6662045221773));
#30452=CARTESIAN_POINT('Ctrl Pts',(20.5192141482499,68.3724644440178,33.5550714041857));
#30453=CARTESIAN_POINT('Ctrl Pts',(22.2747973910883,66.850569042428,33.4439382861942));
#30454=CARTESIAN_POINT('Ctrl Pts',(21.9483965247762,64.5501993772306,33.3328051682026));
#30455=CARTESIAN_POINT('Ctrl Pts',(19.8387464716884,63.5767443045379,33.221672050211));
#30456=CARTESIAN_POINT('Ctrl Pts',(17.8766819941674,64.8211482232738,33.1105389322195));
#30457=CARTESIAN_POINT('Ctrl Pts',(17.8579617287779,67.144483686959,32.9994058142279));
#30458=CARTESIAN_POINT('Ctrl Pts',(19.7997191989097,68.420342634033,32.8882726962363));
#30459=CARTESIAN_POINT('Ctrl Pts',(21.924781541228,67.4810087386156,32.7771395782448));
#30460=CARTESIAN_POINT('Ctrl Pts',(22.2882080583246,65.1861973537148,32.6660064602532));
#30461=CARTESIAN_POINT('Ctrl Pts',(20.5573764974643,63.6362101816373,32.5548733422617));
#30462=CARTESIAN_POINT('Ctrl Pts',(18.3164120279928,64.2496564891946,32.4437402242701));
#30463=CARTESIAN_POINT('Ctrl Pts',(17.6163335358825,66.4650860706858,32.3326071062786));
#30464=CARTESIAN_POINT('Ctrl Pts',(19.0978804119286,68.2548505746783,32.221473988287));
#30465=CARTESIAN_POINT('Ctrl Pts',(21.4050826420595,67.9808870826703,32.1103408702955));
#30466=CARTESIAN_POINT('Ctrl Pts',(22.4262979346632,65.8939377656472,31.9992077523039));
#30467=CARTESIAN_POINT('Ctrl Pts',(21.2268698593072,63.9040607800724,31.8880746343123));
#30468=CARTESIAN_POINT('Ctrl Pts',(18.9045621995861,63.8324698639393,31.7769415163208));
#30469=CARTESIAN_POINT('Ctrl Pts',(17.5848423308155,65.7446878414837,31.6658083983292));
#30470=CARTESIAN_POINT('Ctrl Pts',(18.4755698205621,67.8905775554909,31.5546752803376));
#30471=CARTESIAN_POINT('Ctrl Pts',(20.7615158115174,68.3061362783054,31.4435421623461));
#30472=CARTESIAN_POINT('Ctrl Pts',(22.3504925588018,66.6110283105753,31.3324090443545));
#30473=CARTESIAN_POINT('Ctrl Pts',(21.7882060017851,64.3566831831669,31.2212759263629));
#30474=CARTESIAN_POINT('Ctrl Pts',(19.5892829288324,63.6063662868436,31.1101428083714));
#30475=CARTESIAN_POINT('Ctrl Pts',(17.7662642850786,65.0467971773061,30.9990096903798));
#30476=CARTESIAN_POINT('Ctrl Pts',(17.9876484866019,67.3596368087955,30.8878765723883));
#30477=CARTESIAN_POINT('Ctrl Pts',(20.0508159985709,68.4280833180919,30.7767434543967));
#30478=CARTESIAN_POINT('Ctrl Pts',(22.0674747085496,67.2742524062426,30.6656103364052));
#30479=CARTESIAN_POINT('Ctrl Pts',(22.1918991902521,64.954175538114,30.5544772184136));
#30480=CARTESIAN_POINT('Ctrl Pts',(20.3102112607245,63.5912783807532,30.4433441004221));
#30481=CARTESIAN_POINT('Ctrl Pts',(18.1446057755856,64.4329380556861,30.3322109824305));
#30482=CARTESIAN_POINT('Ctrl Pts',(17.6771301122358,66.7088345010122,30.2210778644389));
#30483=CARTESIAN_POINT('Ctrl Pts',(19.3356363974357,68.3359777115578,30.1099447464474));
#30484=CARTESIAN_POINT('Ctrl Pts',(21.602194400799,67.8251421772989,29.9988116284558));
#30485=CARTESIAN_POINT('Ctrl Pts',(22.402361026794,65.6438646854799,29.8876785104642));
#30486=CARTESIAN_POINT('Ctrl Pts',(21.0037922850585,63.7885362508592,29.7765453924727));
#30487=CARTESIAN_POINT('Ctrl Pts',(18.6865133351581,63.957226481817,29.6654122744811));
#30488=CARTESIAN_POINT('Ctrl Pts',(17.5713890792524,65.9955434393982,29.5542791564896));
#30489=CARTESIAN_POINT('Ctrl Pts',(18.6790251272092,68.0379392166506,29.443146038498));
#30490=CARTESIAN_POINT('Ctrl Pts',(20.9956693718085,68.2151328103185,29.3320129205064));
#30491=CARTESIAN_POINT('Ctrl Pts',(22.4010378181641,66.3649496692051,29.2208798025149));
#30492=CARTESIAN_POINT('Ctrl Pts',(21.6088819494082,64.1807502265562,29.1097466845233));
#30493=CARTESIAN_POINT('Ctrl Pts',(19.3442139955776,63.6615997815364,28.9986135665318));
#30494=CARTESIAN_POINT('Ctrl Pts',(17.6797472044798,65.2826452549903,28.8874804485402));
#30495=CARTESIAN_POINT('Ctrl Pts',(18.1388670961024,67.5602420258845,28.7763473305487));
#30496=CARTESIAN_POINT('Ctrl Pts',(20.301369074849,68.4098438841618,28.6652142125571));
#30497=CARTESIAN_POINT('Ctrl Pts',(22.1880462145232,67.053861769123,28.5540810945655));
#30498=CARTESIAN_POINT('Ctrl Pts',(22.0721373380047,64.7333438833879,28.442947976574));
#30499=CARTESIAN_POINT('Ctrl Pts',(20.059726811216,63.5721195306752,28.3318148585824));
#30500=CARTESIAN_POINT('Ctrl Pts',(17.9926519559727,64.6329869439321,28.2206817405909));
#30501=CARTESIAN_POINT('Ctrl Pts',(17.7627810390829,66.9449985112133,28.1095486225993));
#30502=CARTESIAN_POINT('Ctrl Pts',(19.5805009712835,68.3921102462499,27.9984155046077));
#30503=CARTESIAN_POINT('Ctrl Pts',(21.7821629259284,67.6498685313834,27.8872823866162));
#30504=CARTESIAN_POINT('Ctrl Pts',(22.3527192254304,65.3976021983889,27.7761492686246));
#30505=CARTESIAN_POINT('Ctrl Pts',(20.7699742878597,63.6966740436017,27.6650161506331));
#30506=CARTESIAN_POINT('Ctrl Pts',(18.482518575813,64.103840462084,27.5538830326415));
#30507=CARTESIAN_POINT('Ctrl Pts',(17.5839215913354,66.2464467218836,27.4427499146499));
#30508=CARTESIAN_POINT('Ctrl Pts',(18.8966146610587,68.1634952415589,27.3316167966584));
#30509=CARTESIAN_POINT('Ctrl Pts',(21.2191694244532,68.1004277622309,27.2204836786668));
#30510=CARTESIAN_POINT('Ctrl Pts',(22.4258923392674,66.1149661220525,27.1093505606753));
#30511=CARTESIAN_POINT('Ctrl Pts',(21.4123431135179,64.0242829635948,26.9982174426837));
#30512=CARTESIAN_POINT('Ctrl Pts',(19.1061618600091,63.7418537970392,26.8870843246921));
#30513=CARTESIAN_POINT('Ctrl Pts',(17.6180564951812,65.5261689217424,26.7759512067006));
#30514=CARTESIAN_POINT('Ctrl Pts',(18.3099994949436,67.7441528860369,26.664818088709));
#30515=CARTESIAN_POINT('Ctrl Pts',(20.5486976409782,68.3658195058375,26.5536849707175));
#30516=CARTESIAN_POINT('Ctrl Pts',(22.2852057779767,66.8221949443221,26.4425518527259));
#30517=CARTESIAN_POINT('Ctrl Pts',(21.9302043029995,64.5260653118046,26.3314187347344));
#30518=CARTESIAN_POINT('Ctrl Pts',(19.8086025603331,63.5789385134492,26.2202856167428));
#30519=CARTESIAN_POINT('Ctrl Pts',(17.8621779143328,64.8476628902778,26.1091524987512));
#30520=CARTESIAN_POINT('Ctrl Pts',(17.8723669486581,67.1710507268108,25.9980193807597));
#30521=CARTESIAN_POINT('Ctrl Pts',(19.8298599336245,68.4226484781515,25.8868862627681));
#30522=CARTESIAN_POINT('Ctrl Pts',(21.9430509921809,67.4569397340099,25.7757531447766));
#30523=CARTESIAN_POINT('Ctrl Pts',(22.2779267956692,65.1577888874642,25.664620026785));
#30524=CARTESIAN_POINT('Ctrl Pts',(20.5278716209092,63.6294498681163,25.5534869087934));
#30525=CARTESIAN_POINT('Ctrl Pts',(18.2948524671343,64.2707574153019,25.4423537908019));
#30526=CARTESIAN_POINT('Ctrl Pts',(17.6221226867318,66.4946844357757,25.3312206728103));
#30527=CARTESIAN_POINT('Ctrl Pts',(19.1263753077513,68.2659593106943,25.2200875548188));
#30528=CARTESIAN_POINT('Ctrl Pts',(21.4288959883911,67.963134090779,25.1089544368272));
#30529=CARTESIAN_POINT('Ctrl Pts',(22.4262527337127,65.8639872238968,24.9978213188357));
#30530=CARTESIAN_POINT('Ctrl Pts',(21.1976535364003,63.8884104850849,24.8866882008441));
#30531=CARTESIAN_POINT('Ctrl Pts',(19.6563391459161,63.8620828587222,24.8125994555164));
#30532=CARTESIAN_POINT('Ctrl Pts',(19.0504464477386,64.1778184465077,24.7755550828525));
#30533=CARTESIAN_POINT('Ctrl Pts',(19.5032651029124,64.1400211999972,36.0748149723825));
#30534=CARTESIAN_POINT('Ctrl Pts',(18.8848044607624,64.3051902779623,36.0377705997186));
#30535=CARTESIAN_POINT('Ctrl Pts',(17.8363619404734,65.2985851392148,35.963681854391));
#30536=CARTESIAN_POINT('Ctrl Pts',(18.2373212128777,67.4411195309724,35.8525487363994));
#30537=CARTESIAN_POINT('Ctrl Pts',(20.2546748761206,68.2606654375174,35.7414156184078));
#30538=CARTESIAN_POINT('Ctrl Pts',(22.0373941711252,67.0131051606116,35.6302825004163));
#30539=CARTESIAN_POINT('Ctrl Pts',(21.9561840847596,64.8373421837361,35.5191493824247));
#30540=CARTESIAN_POINT('Ctrl Pts',(20.0842092279223,63.7261749821672,35.4080162644331));
#30541=CARTESIAN_POINT('Ctrl Pts',(18.1353574345361,64.6958584022151,35.2968831464416));
#30542=CARTESIAN_POINT('Ctrl Pts',(17.8930022659816,66.8592656960662,35.18575002845));
#30543=CARTESIAN_POINT('Ctrl Pts',(19.5791033318916,68.2361779326022,35.0746169104584));
#30544=CARTESIAN_POINT('Ctrl Pts',(21.6504010275187,67.5664828441779,34.9634837924669));
#30545=CARTESIAN_POINT('Ctrl Pts',(22.2111990665867,65.4630655843475,34.8523506744753));
#30546=CARTESIAN_POINT('Ctrl Pts',(20.7482145067436,63.8510795680691,34.7412175564838));
#30547=CARTESIAN_POINT('Ctrl Pts',(18.6004376814038,64.2058662329868,34.6300844384922));
#30548=CARTESIAN_POINT('Ctrl Pts',(17.7335938210583,66.2027166834992,34.5189513205006));
#30549=CARTESIAN_POINT('Ctrl Pts',(18.9410548806594,68.0140318705027,34.4078182025091));
#30550=CARTESIAN_POINT('Ctrl Pts',(21.1177038018548,67.9820263076229,34.2966850845175));
#30551=CARTESIAN_POINT('Ctrl Pts',(22.2713864074764,66.135992010666,34.185551966526));
#30552=CARTESIAN_POINT('Ctrl Pts',(21.3462066736251,64.16549259612,34.0744188485344));
#30553=CARTESIAN_POINT('Ctrl Pts',(19.1889256552778,63.8740065013327,33.9632857305429));
#30554=CARTESIAN_POINT('Ctrl Pts',(17.7739717760243,65.5283133658033,33.8521526125513));
#30555=CARTESIAN_POINT('Ctrl Pts',(18.3963665553957,67.6143263877517,33.7410194945598));
#30556=CARTESIAN_POINT('Ctrl Pts',(20.4864697754337,68.2228443681591,33.6298863765682));
#30557=CARTESIAN_POINT('Ctrl Pts',(22.1313367128573,66.7969276886147,33.5187532585767));
#30558=CARTESIAN_POINT('Ctrl Pts',(21.8255204005102,64.6416314236435,33.4076201405851));
#30559=CARTESIAN_POINT('Ctrl Pts',(19.8489159666199,63.7295675436361,33.2964870225935));
#30560=CARTESIAN_POINT('Ctrl Pts',(18.0105895862942,64.8954928115371,33.185353904602));
#30561=CARTESIAN_POINT('Ctrl Pts',(17.9930499192208,67.0723065310512,33.0742207866104));
#30562=CARTESIAN_POINT('Ctrl Pts',(19.8123499587627,68.2677031078975,32.9630876686188));
#30563=CARTESIAN_POINT('Ctrl Pts',(21.8033947019285,67.3876085444093,32.8519545506273));
#30564=CARTESIAN_POINT('Ctrl Pts',(22.1439016329405,65.2375200253688,32.7408214326357));
#30565=CARTESIAN_POINT('Ctrl Pts',(20.522225406352,63.7852831900144,32.6296883146442));
#30566=CARTESIAN_POINT('Ctrl Pts',(18.4225879332721,64.360042349571,32.5185551966526));
#30567=CARTESIAN_POINT('Ctrl Pts',(17.7666600699987,66.4357552989003,32.407422078661));
#30568=CARTESIAN_POINT('Ctrl Pts',(19.154772814064,68.1126478475166,32.2962889606695));
#30569=CARTESIAN_POINT('Ctrl Pts',(21.3164707465165,67.8559619330757,32.1851558426779));
#30570=CARTESIAN_POINT('Ctrl Pts',(22.2732828359731,65.9006266075346,32.0740227246864));
#30571=CARTESIAN_POINT('Ctrl Pts',(21.1494969984068,64.0362417220762,31.9628896066948));
#30572=CARTESIAN_POINT('Ctrl Pts',(18.9736462641375,63.9691657053464,31.8517564887033));
#30573=CARTESIAN_POINT('Ctrl Pts',(17.737154865819,65.7607891679424,31.7406233707117));
#30574=CARTESIAN_POINT('Ctrl Pts',(18.5717083990195,67.7713477992842,31.6294902527202));
#30575=CARTESIAN_POINT('Ctrl Pts',(20.713490622447,68.1606992051511,31.5183571347285));
#30576=CARTESIAN_POINT('Ctrl Pts',(22.2022581454937,66.5724936541716,31.407224016737));
#30577=CARTESIAN_POINT('Ctrl Pts',(21.6754323337487,64.4603193777638,31.2960908987454));
#30578=CARTESIAN_POINT('Ctrl Pts',(19.6151849057827,63.7573214080651,31.1849577807539));
#30579=CARTESIAN_POINT('Ctrl Pts',(17.907135398219,65.1069111566746,31.0738246627623));
#30580=CARTESIAN_POINT('Ctrl Pts',(18.1145579485532,67.2738909663297,30.9626915447708));
#30581=CARTESIAN_POINT('Ctrl Pts',(20.0476112746476,68.2749556237401,30.8515584267792));
#30582=CARTESIAN_POINT('Ctrl Pts',(21.9370888882229,67.1938913529227,30.7404253087876));
#30583=CARTESIAN_POINT('Ctrl Pts',(22.053666508221,65.0201307248047,30.6292921907961));
#30584=CARTESIAN_POINT('Ctrl Pts',(20.2906477083691,63.7431850246242,30.5181590728045));
#30585=CARTESIAN_POINT('Ctrl Pts',(18.2616166860355,64.5317652172796,30.407025954813));
#30586=CARTESIAN_POINT('Ctrl Pts',(17.8236224947427,66.6641316722385,30.2958928368214));
#30587=CARTESIAN_POINT('Ctrl Pts',(19.3775346576452,68.1886586807968,30.1847597188299));
#30588=CARTESIAN_POINT('Ctrl Pts',(21.501151601868,67.7100391199237,30.0736266008383));
#30589=CARTESIAN_POINT('Ctrl Pts',(22.2508555153098,65.6663244500125,29.9624934828467));
#30590=CARTESIAN_POINT('Ctrl Pts',(20.9404878683304,63.9280027767916,29.8513603648552));
#30591=CARTESIAN_POINT('Ctrl Pts',(18.7693487070131,64.0860545152668,29.7402272468636));
#30592=CARTESIAN_POINT('Ctrl Pts',(17.7245500470004,65.9958244935304,29.6290941288721));
#30593=CARTESIAN_POINT('Ctrl Pts',(18.7623327448103,67.909416059661,29.5179610108805));
#30594=CARTESIAN_POINT('Ctrl Pts',(20.9328772286783,68.0754348941062,29.4068278928889));
#30595=CARTESIAN_POINT('Ctrl Pts',(22.24961575517,66.3419340251441,29.2956947748974));
#30596=CARTESIAN_POINT('Ctrl Pts',(21.5074173985168,64.2954816779778,29.1845616569058));
#30597=CARTESIAN_POINT('Ctrl Pts',(19.3855713073705,63.8090715883138,29.0734285389143));
#30598=CARTESIAN_POINT('Ctrl Pts',(17.8260745393962,65.3278854151269,28.9622954209227));
#30599=CARTESIAN_POINT('Ctrl Pts',(18.2562399178391,67.4618449641881,28.8511623029311));
#30600=CARTESIAN_POINT('Ctrl Pts',(20.2823631572033,68.2578664643672,28.7400291849396));
#30601=CARTESIAN_POINT('Ctrl Pts',(22.0500565213901,66.9873997075995,28.628896066948));
#30602=CARTESIAN_POINT('Ctrl Pts',(21.9414574677611,64.8132258747628,28.5177629489565));
#30603=CARTESIAN_POINT('Ctrl Pts',(20.0559601246183,63.7252344323179,28.4066298309649));
#30604=CARTESIAN_POINT('Ctrl Pts',(18.1192458728508,64.7191979713152,28.2954967129734));
#30605=CARTESIAN_POINT('Ctrl Pts',(17.9038718240213,66.8854019388429,28.1843635949818));
#30606=CARTESIAN_POINT('Ctrl Pts',(19.6069567846287,68.2412512028579,28.0732304769903));
#30607=CARTESIAN_POINT('Ctrl Pts',(21.6697703660137,67.5458191512356,27.9620973589987));
#30608=CARTESIAN_POINT('Ctrl Pts',(22.2043443868229,65.4355925695414,27.8509642410071));
#30609=CARTESIAN_POINT('Ctrl Pts',(20.7214156628193,63.8419338830873,27.7398311230155));
#30610=CARTESIAN_POINT('Ctrl Pts',(18.5782189292465,64.2234222474375,27.628698005024));
#30611=CARTESIAN_POINT('Ctrl Pts',(17.7362921930093,66.2309044964494,27.5175648870324));
#30612=CARTESIAN_POINT('Ctrl Pts',(18.9661999391564,68.0270538618038,27.4064317690409));
#30613=CARTESIAN_POINT('Ctrl Pts',(21.1422821934428,67.9679637491608,27.2952986510493));
#30614=CARTESIAN_POINT('Ctrl Pts',(22.2729028195545,66.107715754214,27.1841655330578));
#30615=CARTESIAN_POINT('Ctrl Pts',(21.3232733344888,64.1488820629017,27.0730324150662));
#30616=CARTESIAN_POINT('Ctrl Pts',(19.1625319905069,63.8842643638399,26.9618992970746));
#30617=CARTESIAN_POINT('Ctrl Pts',(17.7682743704294,65.556051199663,26.8507661790831));
#30618=CARTESIAN_POINT('Ctrl Pts',(18.4165798082567,67.6341574389921,26.7396330610915));
#30619=CARTESIAN_POINT('Ctrl Pts',(20.5140938841659,68.2166184947016,26.6284999431));
#30620=CARTESIAN_POINT('Ctrl Pts',(22.1410886921693,66.7703430102498,26.5173668251084));
#30621=CARTESIAN_POINT('Ctrl Pts',(21.8084754758444,64.6190193792151,26.4062337071169));
#30622=CARTESIAN_POINT('Ctrl Pts',(19.8206730887299,63.7316233742022,26.2951005891253));
#30623=CARTESIAN_POINT('Ctrl Pts',(17.9970002099573,64.9203353242972,26.1839674711337));
#30624=CARTESIAN_POINT('Ctrl Pts',(18.0065466702315,67.097198113752,26.0728343531422));
#30625=CARTESIAN_POINT('Ctrl Pts',(19.8405898603477,68.2698635333681,25.9617012351506));
#30626=CARTESIAN_POINT('Ctrl Pts',(21.8205119852927,67.3650574577238,25.8505681171591));
#30627=CARTESIAN_POINT('Ctrl Pts',(22.1342687607394,65.2109031462952,25.7394349991675));
#30628=CARTESIAN_POINT('Ctrl Pts',(20.4945812623694,63.7789492173915,25.6283018811759));
#30629=CARTESIAN_POINT('Ctrl Pts',(18.4023880316233,64.3798125403864,25.5171687631844));
#30630=CARTESIAN_POINT('Ctrl Pts',(17.7720841265718,66.4634870355391,25.4060356451928));
#30631=CARTESIAN_POINT('Ctrl Pts',(19.1814706720067,68.1230560082598,25.2949025272013));
#30632=CARTESIAN_POINT('Ctrl Pts',(21.3387822980822,67.8393285381504,25.1837694092097));
#30633=CARTESIAN_POINT('Ctrl Pts',(22.2732404856321,65.8725649043462,25.0726362912182));
#30634=CARTESIAN_POINT('Ctrl Pts',(21.122123210363,64.0215784169376,24.9615031732266));
#30635=CARTESIAN_POINT('Ctrl Pts',(19.6780122054164,63.996911149053,24.8874144278989));
#30636=CARTESIAN_POINT('Ctrl Pts',(19.1103302849356,64.2927347913866,24.850370055235));
#30637=CARTESIAN_POINT('Ctrl Pts',(19.5367004230133,64.2652167256662,36.149629944765));
#30638=CARTESIAN_POINT('Ctrl Pts',(18.9598684839429,64.4192682416784,36.1125855721011));
#30639=CARTESIAN_POINT('Ctrl Pts',(17.9819968284729,65.3457975064782,36.0384968267734));
#30640=CARTESIAN_POINT('Ctrl Pts',(18.3559674562322,67.3441175021151,35.9273637087819));
#30641=CARTESIAN_POINT('Ctrl Pts',(20.2375326619242,68.1084996183096,35.8162305907903));
#30642=CARTESIAN_POINT('Ctrl Pts',(21.9002567831891,66.9449128601723,35.7050974727988));
#30643=CARTESIAN_POINT('Ctrl Pts',(21.8245129631337,64.9156009017816,35.5939643548072));
#30644=CARTESIAN_POINT('Ctrl Pts',(20.0785410888253,63.8792265752211,35.4828312368157));
#30645=CARTESIAN_POINT('Ctrl Pts',(18.2608668791425,64.7836404204194,35.371698118824));
#30646=CARTESIAN_POINT('Ctrl Pts',(18.0348246829324,66.8014283591525,35.2605650008325));
#30647=CARTESIAN_POINT('Ctrl Pts',(19.6074339664214,68.0856603719928,35.1494318828409));
#30648=CARTESIAN_POINT('Ctrl Pts',(21.5393122214503,67.4610425869407,35.0382987648494));
#30649=CARTESIAN_POINT('Ctrl Pts',(22.0623628381848,65.4992067416645,34.9271656468578));
#30650=CARTESIAN_POINT('Ctrl Pts',(20.6978520464377,63.9957238097648,34.8160325288663));
#30651=CARTESIAN_POINT('Ctrl Pts',(18.6946424864171,64.3266297170013,34.7048994108747));
#30652=CARTESIAN_POINT('Ctrl Pts',(17.8861460506599,66.189071785099,34.5937662928832));
#30653=CARTESIAN_POINT('Ctrl Pts',(19.0123326774118,67.8784670034509,34.4826331748916));
#30654=CARTESIAN_POINT('Ctrl Pts',(21.042470947042,67.8486157410765,34.3715000569));
#30655=CARTESIAN_POINT('Ctrl Pts',(22.118498957748,66.1268383626448,34.2603669389085));
#30656=CARTESIAN_POINT('Ctrl Pts',(21.2555932471907,64.2889736372867,34.1492338209169));
#30657=CARTESIAN_POINT('Ctrl Pts',(19.2435192231959,64.0171075268036,34.0381007029254));
#30658=CARTESIAN_POINT('Ctrl Pts',(17.9238061578216,65.5600626825801,33.9269675849338));
#30659=CARTESIAN_POINT('Ctrl Pts',(18.5043074265913,67.5056657725256,33.8158344669422));
#30660=CARTESIAN_POINT('Ctrl Pts',(20.4537254026176,68.0732242923004,33.7047013489507));
#30661=CARTESIAN_POINT('Ctrl Pts',(21.9878760346263,66.7432863348013,33.5935682309592));
#30662=CARTESIAN_POINT('Ctrl Pts',(21.7026442762442,64.7330634700566,33.4824351129676));
#30663=CARTESIAN_POINT('Ctrl Pts',(19.8590854615513,63.8823907827342,33.371301994976));
#30664=CARTESIAN_POINT('Ctrl Pts',(18.1444971784209,64.9698373998005,33.2601688769845));
#30665=CARTESIAN_POINT('Ctrl Pts',(18.1281381096636,67.0001293751432,33.1490357589929));
#30666=CARTESIAN_POINT('Ctrl Pts',(19.8249807186157,68.1150635817621,33.0379026410013));
#30667=CARTESIAN_POINT('Ctrl Pts',(21.6820078626288,67.2942083502029,32.9267695230098));
#30668=CARTESIAN_POINT('Ctrl Pts',(21.9995952075565,65.2888426970229,32.8156364050182));
#30669=CARTESIAN_POINT('Ctrl Pts',(20.4870743152396,63.9343561983915,32.7045032870266));
#30670=CARTESIAN_POINT('Ctrl Pts',(18.5287638385514,64.4704282099475,32.5933701690351));
#30671=CARTESIAN_POINT('Ctrl Pts',(17.9169866041149,66.4064245271147,32.4822370510436));
#30672=CARTESIAN_POINT('Ctrl Pts',(19.2116652161993,67.9704451203549,32.3711039330519));
#30673=CARTESIAN_POINT('Ctrl Pts',(21.2278588509736,67.7310367834812,32.2599708150604));
#30674=CARTESIAN_POINT('Ctrl Pts',(22.120267737283,65.9073154494221,32.1488376970688));
#30675=CARTESIAN_POINT('Ctrl Pts',(21.0721241375063,64.16842266408,32.0377045790773));
#30676=CARTESIAN_POINT('Ctrl Pts',(19.0427303286889,64.1058615467534,31.9265714610857));
#30677=CARTESIAN_POINT('Ctrl Pts',(17.8894674008225,65.7768904944012,31.8154383430942));
#30678=CARTESIAN_POINT('Ctrl Pts',(18.667846977477,67.6521180430775,31.7043052251026));
#30679=CARTESIAN_POINT('Ctrl Pts',(20.6654654333766,68.0152621319967,31.5931721071111));
#30680=CARTESIAN_POINT('Ctrl Pts',(22.0540237321857,66.5339589977681,31.4820389891195));
#30681=CARTESIAN_POINT('Ctrl Pts',(21.5626586657121,64.5639555723606,31.3709058711279));
#30682=CARTESIAN_POINT('Ctrl Pts',(19.6410868827332,63.9082765292868,31.2597727531364));
#30683=CARTESIAN_POINT('Ctrl Pts',(18.0480065113594,65.167025136043,31.1486396351448));
#30684=CARTESIAN_POINT('Ctrl Pts',(18.2414674105046,67.1881451238641,31.0375065171532));
#30685=CARTESIAN_POINT('Ctrl Pts',(20.0444065507242,68.1218279293882,30.9263733991617));
#30686=CARTESIAN_POINT('Ctrl Pts',(21.8067030678963,67.1135302996029,30.8152402811701));
#30687=CARTESIAN_POINT('Ctrl Pts',(21.9154338261898,65.0860859114954,30.7041071631786));
#30688=CARTESIAN_POINT('Ctrl Pts',(20.2710841560138,63.8950916684954,30.592974045187));
#30689=CARTESIAN_POINT('Ctrl Pts',(18.3786275964855,64.630592378873,30.4818409271955));
#30690=CARTESIAN_POINT('Ctrl Pts',(17.9701148772496,66.6194288434647,30.3707078092039));
#30691=CARTESIAN_POINT('Ctrl Pts',(19.4194329178548,68.041339650036,30.2595746912123));
#30692=CARTESIAN_POINT('Ctrl Pts',(21.4001088029369,67.5949360625485,30.1484415732208));
#30693=CARTESIAN_POINT('Ctrl Pts',(22.0993500038257,65.688784214545,30.0373084552292));
#30694=CARTESIAN_POINT('Ctrl Pts',(20.8771834516022,64.0674693027239,29.9261753372377));
#30695=CARTESIAN_POINT('Ctrl Pts',(18.8521840788682,64.2148825487168,29.8150422192461));
#30696=CARTESIAN_POINT('Ctrl Pts',(17.8777110147484,65.9961055476625,29.7039091012546));
#30697=CARTESIAN_POINT('Ctrl Pts',(18.8456403624114,67.7808929026714,29.592775983263));
#30698=CARTESIAN_POINT('Ctrl Pts',(20.870085085548,67.935736977894,29.4816428652714));
#30699=CARTESIAN_POINT('Ctrl Pts',(22.0981936921759,66.318918381083,29.3705097472799));
#30700=CARTESIAN_POINT('Ctrl Pts',(21.4059528476254,64.4102131293996,29.2593766292883));
#30701=CARTESIAN_POINT('Ctrl Pts',(19.4269286191633,63.9565433950913,29.1482435112968));
#30702=CARTESIAN_POINT('Ctrl Pts',(17.9724018743126,65.3731255752635,29.0371103933052));
#30703=CARTESIAN_POINT('Ctrl Pts',(18.3736127395757,67.3634479024916,28.9259772753137));
#30704=CARTESIAN_POINT('Ctrl Pts',(20.2633572395576,68.1058890445728,28.8148441573221));
#30705=CARTESIAN_POINT('Ctrl Pts',(21.912066828257,66.9209376460759,28.7037110393305));
#30706=CARTESIAN_POINT('Ctrl Pts',(21.8107775975175,64.8931078661378,28.592577921339));
#30707=CARTESIAN_POINT('Ctrl Pts',(20.0521934380205,63.8783493339604,28.4814448033474));
#30708=CARTESIAN_POINT('Ctrl Pts',(18.2458397897289,64.8054089986984,28.3703116853558));
#30709=CARTESIAN_POINT('Ctrl Pts',(18.0449626089597,66.8258053664725,28.2591785673643));
#30710=CARTESIAN_POINT('Ctrl Pts',(19.633412597974,68.0903921594658,28.1480454493727));
#30711=CARTESIAN_POINT('Ctrl Pts',(21.5573778060989,67.441769771088,28.0369123313812));
#30712=CARTESIAN_POINT('Ctrl Pts',(22.0559695482155,65.4735829406938,27.9257792133896));
#30713=CARTESIAN_POINT('Ctrl Pts',(20.6728570377789,63.987193722573,27.814646095398));
#30714=CARTESIAN_POINT('Ctrl Pts',(18.6739192826801,64.3430040327909,27.7035129774065));
#30715=CARTESIAN_POINT('Ctrl Pts',(17.8886627946832,66.2153622710153,27.5923798594149));
#30716=CARTESIAN_POINT('Ctrl Pts',(19.035785217254,67.8906124820486,27.4812467414234));
#30717=CARTESIAN_POINT('Ctrl Pts',(21.0653949624323,67.8354997360908,27.3701136234318));
#30718=CARTESIAN_POINT('Ctrl Pts',(22.1199132998416,66.1004653863756,27.2589805054402));
#30719=CARTESIAN_POINT('Ctrl Pts',(21.2342035554597,64.2734811622086,27.1478473874487));
#30720=CARTESIAN_POINT('Ctrl Pts',(19.2189021210048,64.0266749306405,27.0367142694571));
#30721=CARTESIAN_POINT('Ctrl Pts',(17.9184922456775,65.5859334775838,26.9255811514656));
#30722=CARTESIAN_POINT('Ctrl Pts',(18.5231601215699,67.524161991947,26.814448033474));
#30723=CARTESIAN_POINT('Ctrl Pts',(20.4794901273535,68.0674174835658,26.7033149154825));
#30724=CARTESIAN_POINT('Ctrl Pts',(21.9969716063619,66.7184910761775,26.5921817974909));
#30725=CARTESIAN_POINT('Ctrl Pts',(21.6867466486893,64.7119734466258,26.4810486794993));
#30726=CARTESIAN_POINT('Ctrl Pts',(19.8327436171269,63.8843082349551,26.3699155615078));
#30727=CARTESIAN_POINT('Ctrl Pts',(18.1318225055817,64.9930077583167,26.2587824435162));
#30728=CARTESIAN_POINT('Ctrl Pts',(18.140726391805,67.0233455006932,26.1476493255247));
#30729=CARTESIAN_POINT('Ctrl Pts',(19.8513197870709,68.1170785885846,26.0365162075331));
#30730=CARTESIAN_POINT('Ctrl Pts',(21.6979729784046,67.2731751814378,25.9253830895416));
#30731=CARTESIAN_POINT('Ctrl Pts',(21.9906107258095,65.2640174051259,25.81424997155));
#30732=CARTESIAN_POINT('Ctrl Pts',(20.4612909038297,63.9284485666668,25.7031168535584));
#30733=CARTESIAN_POINT('Ctrl Pts',(18.5099235961124,64.4888676654707,25.5919837355669));
#30734=CARTESIAN_POINT('Ctrl Pts',(17.9220455664116,66.4322896353026,25.4808506175753));
#30735=CARTESIAN_POINT('Ctrl Pts',(19.2365660362622,67.9801527058252,25.3697174995838));
#30736=CARTESIAN_POINT('Ctrl Pts',(21.2486686077732,67.7155229855219,25.2585843815922));
#30737=CARTESIAN_POINT('Ctrl Pts',(22.1202282375515,65.8811425847956,25.1474512636007));
#30738=CARTESIAN_POINT('Ctrl Pts',(21.0465928843257,64.1547463487904,25.0363181456091));
#30739=CARTESIAN_POINT('Ctrl Pts',(19.6996852649168,64.1317394393838,24.9622294002814));
#30740=CARTESIAN_POINT('Ctrl Pts',(19.1702141221326,64.4076511362656,24.9251850276175));
#30741=CARTESIAN_POINT('Ctrl Pts',(19.5701357431142,64.3904122513351,36.2244449171475));
#30742=CARTESIAN_POINT('Ctrl Pts',(19.0349325071233,64.5333462053944,36.1874005444836));
#30743=CARTESIAN_POINT('Ctrl Pts',(18.1276317164724,65.3930098737417,36.1133117991559));
#30744=CARTESIAN_POINT('Ctrl Pts',(18.4746136995867,67.2471154732578,36.0021786811644));
#30745=CARTESIAN_POINT('Ctrl Pts',(20.2203904477277,67.9563337991017,35.8910455631728));
#30746=CARTESIAN_POINT('Ctrl Pts',(21.763119395253,66.8767205597329,35.7799124451812));
#30747=CARTESIAN_POINT('Ctrl Pts',(21.6928418415078,64.9938596198273,35.6687793271897));
#30748=CARTESIAN_POINT('Ctrl Pts',(20.0728729497283,64.0322781682749,35.5576462091981));
#30749=CARTESIAN_POINT('Ctrl Pts',(18.3863763237488,64.8714224386236,35.4465130912065));
#30750=CARTESIAN_POINT('Ctrl Pts',(18.1766470998833,66.7435910222386,35.335379973215));
#30751=CARTESIAN_POINT('Ctrl Pts',(19.6357646009513,67.9351428113835,35.2242468552234));
#30752=CARTESIAN_POINT('Ctrl Pts',(21.4282234153819,67.3556023297033,35.1131137372319));
#30753=CARTESIAN_POINT('Ctrl Pts',(21.9135266097828,65.5353478989816,35.0019806192403));
#30754=CARTESIAN_POINT('Ctrl Pts',(20.6474895861319,64.1403680514604,34.8908475012488));
#30755=CARTESIAN_POINT('Ctrl Pts',(18.7888472914304,64.447393201016,34.7797143832572));
#30756=CARTESIAN_POINT('Ctrl Pts',(18.0386982802614,66.1754268866989,34.6685812652656));
#30757=CARTESIAN_POINT('Ctrl Pts',(19.0836104741642,67.742902136399,34.5574481472741));
#30758=CARTESIAN_POINT('Ctrl Pts',(20.9672380922293,67.7152051745302,34.4463150292825));
#30759=CARTESIAN_POINT('Ctrl Pts',(21.9656115080195,66.1176847146236,34.335181911291));
#30760=CARTESIAN_POINT('Ctrl Pts',(21.1649798207563,64.4124546784534,34.2240487932994));
#30761=CARTESIAN_POINT('Ctrl Pts',(19.2981127911139,64.1602085522744,34.1129156753079));
#30762=CARTESIAN_POINT('Ctrl Pts',(18.073640539619,65.5918119993568,34.0017825573163));
#30763=CARTESIAN_POINT('Ctrl Pts',(18.6122482977868,67.3970051572994,33.8906494393248));
#30764=CARTESIAN_POINT('Ctrl Pts',(20.4209810298014,67.9236042164417,33.7795163213331));
#30765=CARTESIAN_POINT('Ctrl Pts',(21.8444153563953,66.689644980988,33.6683832033417));
#30766=CARTESIAN_POINT('Ctrl Pts',(21.5797681519781,64.8244955164696,33.55725008535));
#30767=CARTESIAN_POINT('Ctrl Pts',(19.8692549564828,64.0352140218324,33.4461169673585));
#30768=CARTESIAN_POINT('Ctrl Pts',(18.2784047705477,65.0441819880638,33.3349838493669));
#30769=CARTESIAN_POINT('Ctrl Pts',(18.2632263001066,66.9279522192353,33.2238507313754));
#30770=CARTESIAN_POINT('Ctrl Pts',(19.8376114784687,67.9624240556267,33.1127176133838));
#30771=CARTESIAN_POINT('Ctrl Pts',(21.5606210233293,67.2008081559964,33.0015844953923));
#30772=CARTESIAN_POINT('Ctrl Pts',(21.8552887821724,65.3401653686769,32.8904513774007));
#30773=CARTESIAN_POINT('Ctrl Pts',(20.4519232241273,64.0834292067686,32.7793182594091));
#30774=CARTESIAN_POINT('Ctrl Pts',(18.6349397438307,64.5808140703239,32.6681851414176));
#30775=CARTESIAN_POINT('Ctrl Pts',(18.0673131382311,66.3770937553291,32.557052023426));
#30776=CARTESIAN_POINT('Ctrl Pts',(19.2685576183346,67.8282423931933,32.4459189054345));
#30777=CARTESIAN_POINT('Ctrl Pts',(21.1392469554306,67.6061116338867,32.3347857874429));
#30778=CARTESIAN_POINT('Ctrl Pts',(21.9672526385929,65.9140042913095,32.2236526694513));
#30779=CARTESIAN_POINT('Ctrl Pts',(20.9947512766059,64.3006036060839,32.1125195514598));
#30780=CARTESIAN_POINT('Ctrl Pts',(19.1118143932403,64.2425573881604,32.0013864334682));
#30781=CARTESIAN_POINT('Ctrl Pts',(18.0417799358261,65.79299182086,31.8902533154767));
#30782=CARTESIAN_POINT('Ctrl Pts',(18.7639855559345,67.5328882868707,31.7791201974851));
#30783=CARTESIAN_POINT('Ctrl Pts',(20.6174402443061,67.8698250588426,31.6679870794936));
#30784=CARTESIAN_POINT('Ctrl Pts',(21.9057893188776,66.4954243413644,31.556853961502));
#30785=CARTESIAN_POINT('Ctrl Pts',(21.4498849976757,64.6675917669575,31.4457208435104));
#30786=CARTESIAN_POINT('Ctrl Pts',(19.6669888596835,64.0592316505081,31.3345877255189));
#30787=CARTESIAN_POINT('Ctrl Pts',(18.1888776244998,65.2271391154115,31.2234546075273));
#30788=CARTESIAN_POINT('Ctrl Pts',(18.3683768724559,67.1023992813984,31.1123214895357));
#30789=CARTESIAN_POINT('Ctrl Pts',(20.0412018268009,67.9687002350364,31.0011883715442));
#30790=CARTESIAN_POINT('Ctrl Pts',(21.6763172475696,67.0331692462831,30.8900552535526));
#30791=CARTESIAN_POINT('Ctrl Pts',(21.7772011441587,65.1520410981861,30.7789221355611));
#30792=CARTESIAN_POINT('Ctrl Pts',(20.2515206036584,64.0469983123664,30.6677890175695));
#30793=CARTESIAN_POINT('Ctrl Pts',(18.4956385069354,64.7294195404663,30.556655899578));
#30794=CARTESIAN_POINT('Ctrl Pts',(18.1166072597565,66.574726014691,30.4455227815864));
#30795=CARTESIAN_POINT('Ctrl Pts',(19.4613311780644,67.8940206192749,30.3343896635949));
#30796=CARTESIAN_POINT('Ctrl Pts',(21.2990660040059,67.4798330051734,30.2232565456033));
#30797=CARTESIAN_POINT('Ctrl Pts',(21.9478444923416,65.7112439790775,30.1121234276117));
#30798=CARTESIAN_POINT('Ctrl Pts',(20.8138790348741,64.2069358286563,30.0009903096202));
#30799=CARTESIAN_POINT('Ctrl Pts',(18.9350194507232,64.3437105821668,29.8898571916286));
#30800=CARTESIAN_POINT('Ctrl Pts',(18.0308719824964,65.9963866017945,29.7787240736371));
#30801=CARTESIAN_POINT('Ctrl Pts',(18.9289479800125,67.6523697456819,29.6675909556455));
#30802=CARTESIAN_POINT('Ctrl Pts',(20.8072929424178,67.7960390616817,29.5564578376539));
#30803=CARTESIAN_POINT('Ctrl Pts',(21.9467716291819,66.2959027370219,29.4453247196624));
#30804=CARTESIAN_POINT('Ctrl Pts',(21.3044882967339,64.5249445808212,29.3341916016708));
#30805=CARTESIAN_POINT('Ctrl Pts',(19.4682859309562,64.1040152018687,29.2230584836793));
#30806=CARTESIAN_POINT('Ctrl Pts',(18.118729209229,65.4183657354002,29.1119253656877));
#30807=CARTESIAN_POINT('Ctrl Pts',(18.4909855613124,67.2650508407951,29.0007922476961));
#30808=CARTESIAN_POINT('Ctrl Pts',(20.2443513219119,67.9539116247784,28.8896591297046));
#30809=CARTESIAN_POINT('Ctrl Pts',(21.7740771351238,66.8544755845523,28.778526011713));
#30810=CARTESIAN_POINT('Ctrl Pts',(21.6800977272738,64.9729898575127,28.6673928937215));
#30811=CARTESIAN_POINT('Ctrl Pts',(20.0484267514227,64.0314642356028,28.5562597757298));
#30812=CARTESIAN_POINT('Ctrl Pts',(18.3724337066069,64.8916200260816,28.4451266577384));
#30813=CARTESIAN_POINT('Ctrl Pts',(18.1860533938981,66.7662087941021,28.3339935397467));
#30814=CARTESIAN_POINT('Ctrl Pts',(19.6598684113193,67.9395331160738,28.2228604217553));
#30815=CARTESIAN_POINT('Ctrl Pts',(21.4449852461841,67.3377203909403,28.1117273037636));
#30816=CARTESIAN_POINT('Ctrl Pts',(21.907594709608,65.5115733118462,28.0005941857721));
#30817=CARTESIAN_POINT('Ctrl Pts',(20.6242984127384,64.1324535620588,27.8894610677805));
#30818=CARTESIAN_POINT('Ctrl Pts',(18.7696196361136,64.4625858181443,27.778327949789));
#30819=CARTESIAN_POINT('Ctrl Pts',(18.0410333963571,66.1998200455812,27.6671948317974));
#30820=CARTESIAN_POINT('Ctrl Pts',(19.1053704953516,67.7541711022934,27.5560617138059));
#30821=CARTESIAN_POINT('Ctrl Pts',(20.9885077314219,67.7030357230207,27.4449285958143));
#30822=CARTESIAN_POINT('Ctrl Pts',(21.9669237801287,66.0932150185373,27.3337954778227));
#30823=CARTESIAN_POINT('Ctrl Pts',(21.1451337764306,64.3980802615155,27.2226623598312));
#30824=CARTESIAN_POINT('Ctrl Pts',(19.2752722515027,64.1690854974412,27.1115292418396));
#30825=CARTESIAN_POINT('Ctrl Pts',(18.0687101209256,65.6158157555045,27.0003961238481));
#30826=CARTESIAN_POINT('Ctrl Pts',(18.6297404348831,67.414166544902,26.8892630058565));
#30827=CARTESIAN_POINT('Ctrl Pts',(20.4448863705412,67.9182164724299,26.778129887865));
#30828=CARTESIAN_POINT('Ctrl Pts',(21.8528545205544,66.6666391421051,26.6669967698734));
#30829=CARTESIAN_POINT('Ctrl Pts',(21.5650178215341,64.8049275140365,26.5558636518819));
#30830=CARTESIAN_POINT('Ctrl Pts',(19.8448141455237,64.0369930957082,26.4447305338902));
#30831=CARTESIAN_POINT('Ctrl Pts',(18.2666448012062,65.0656801923361,26.3335974158987));
#30832=CARTESIAN_POINT('Ctrl Pts',(18.2749061133784,66.9494928876345,26.2224642979072));
#30833=CARTESIAN_POINT('Ctrl Pts',(19.8620497137941,67.9642936438011,26.1113311799156));
#30834=CARTESIAN_POINT('Ctrl Pts',(21.5754339715164,67.1812929051517,26.000198061924));
#30835=CARTESIAN_POINT('Ctrl Pts',(21.8469526908796,65.3171316639569,25.8890649439325));
#30836=CARTESIAN_POINT('Ctrl Pts',(20.42800054529,64.0779479159419,25.7779318259409));
#30837=CARTESIAN_POINT('Ctrl Pts',(18.6174591606014,64.5979227905551,25.6667987079493));
#30838=CARTESIAN_POINT('Ctrl Pts',(18.0720070062515,66.4010922350662,25.5556655899578));
#30839=CARTESIAN_POINT('Ctrl Pts',(19.2916614005177,67.8372494033905,25.4445324719663));
#30840=CARTESIAN_POINT('Ctrl Pts',(21.1585549174642,67.5917174328935,25.3333993539747));
#30841=CARTESIAN_POINT('Ctrl Pts',(21.9672159894709,65.8897202652449,25.2222662359831));
#30842=CARTESIAN_POINT('Ctrl Pts',(20.9710625582884,64.2879142806432,25.1111331179916));
#30843=CARTESIAN_POINT('Ctrl Pts',(19.7213583244172,64.2665677297147,25.0370443726639));
#30844=CARTESIAN_POINT('Ctrl Pts',(19.2300979593296,64.5225674811446,25.));
#30845=CARTESIAN_POINT('Ctrl Pts',(18.3361559304958,66.0009441564151,35.3785196366098));
#30846=CARTESIAN_POINT('Ctrl Pts',(18.3350370261301,66.2166368244897,35.3641397488115));
#30847=CARTESIAN_POINT('Ctrl Pts',(18.3739569457115,66.4319423497591,35.3497598610133));
#30848=CARTESIAN_POINT('Ctrl Pts',(18.4547882207056,66.630154889827,35.335379973215));
#30849=CARTESIAN_POINT('Ctrl Pts',(18.6630196002393,67.1407749519536,35.2983356005512));
#30850=CARTESIAN_POINT('Ctrl Pts',(19.1493921005953,67.5379588816685,35.2612912278873));
#30851=CARTESIAN_POINT('Ctrl Pts',(19.6913214865117,67.639960766246,35.2242468552234));
#30852=CARTESIAN_POINT('Ctrl Pts',(20.2332508724282,67.7419626508234,35.1872024825596));
#30853=CARTESIAN_POINT('Ctrl Pts',(20.830737143905,67.5487824902634,35.1501581098958));
#30854=CARTESIAN_POINT('Ctrl Pts',(21.2103641453769,67.1488166715297,35.1131137372319));
#30855=CARTESIAN_POINT('Ctrl Pts',(21.5899911468489,66.7488508527961,35.076069364568));
#30856=CARTESIAN_POINT('Ctrl Pts',(21.7517588783158,66.1420993758888,35.0390249919042));
#30857=CARTESIAN_POINT('Ctrl Pts',(21.6216365734408,65.6062269961817,35.0019806192403));
#30858=CARTESIAN_POINT('Ctrl Pts',(21.4915142685658,65.0703546164746,34.9649362465764));
#30859=CARTESIAN_POINT('Ctrl Pts',(21.0695019273488,64.6053613339675,34.9278918739126));
#30860=CARTESIAN_POINT('Ctrl Pts',(20.5487220409568,64.4240355509732,34.8908475012488));
#30861=CARTESIAN_POINT('Ctrl Pts',(20.0279421545647,64.2427097679789,34.8538031285849));
#30862=CARTESIAN_POINT('Ctrl Pts',(19.4083947229975,64.3450514844974,34.8167587559211));
#30863=CARTESIAN_POINT('Ctrl Pts',(18.9735961720191,64.6842279570372,34.7797143832572));
#30864=CARTESIAN_POINT('Ctrl Pts',(18.5776806249338,64.9930726815236,34.7459828010414));
#30865=CARTESIAN_POINT('Ctrl Pts',(18.3349481418111,65.4982870590469,34.7122512188256));
#30866=CARTESIAN_POINT('Ctrl Pts',(18.3317911471719,66.0008588710395,34.6785196366098));
#30867=CARTESIAN_POINT('Ctrl Pts',(19.4698297828115,64.0148256743282,36.));
#30868=CARTESIAN_POINT('Ctrl Pts',(19.4011650087939,64.0402496944362,36.));
#30869=CARTESIAN_POINT('Ctrl Pts',(19.3342035794783,64.0695633948039,36.));
#30870=CARTESIAN_POINT('Ctrl Pts',(19.2691344316336,64.1024727495347,36.));
#30871=CARTESIAN_POINT('Ctrl Pts',(19.202254333301,64.1362980100978,36.));
#30872=CARTESIAN_POINT('Ctrl Pts',(19.1373725394216,64.1739225412136,36.));
#30873=CARTESIAN_POINT('Ctrl Pts',(19.0747254199949,64.2150717234713,36.));
#30874=CARTESIAN_POINT('Ctrl Pts',(19.0217926982225,64.2498400932789,36.));
#30875=CARTESIAN_POINT('Ctrl Pts',(18.9704556772988,64.2871258137782,36.));
#30876=CARTESIAN_POINT('Ctrl Pts',(18.9208796779014,64.3267812441764,36.));
#30877=CARTESIAN_POINT('Ctrl Pts',(18.8988500225955,64.3444025825921,36.));
#30878=CARTESIAN_POINT('Ctrl Pts',(18.8771683964782,64.3624920156554,36.));
#30879=CARTESIAN_POINT('Ctrl Pts',(18.8558508586253,64.381037312981,36.));
#30880=CARTESIAN_POINT('Ctrl Pts',(18.8441382800365,64.3912267285635,36.));
#30881=CARTESIAN_POINT('Ctrl Pts',(18.8325356292319,64.401553765981,36.));
#30882=CARTESIAN_POINT('Ctrl Pts',(18.8210457040405,64.4120164383406,36.));
#30883=CARTESIAN_POINT('Ctrl Pts',(18.8104521548357,64.421662874902,36.));
#30884=CARTESIAN_POINT('Ctrl Pts',(18.799952995123,64.4314261244654,36.));
#30885=CARTESIAN_POINT('Ctrl Pts',(18.7895663054278,64.4412891742485,36.));
#30886=CARTESIAN_POINT('Ctrl Pts',(18.7364815316182,64.4916977049905,36.));
#30887=CARTESIAN_POINT('Ctrl Pts',(18.6862367517015,64.5447946360434,36.));
#30888=CARTESIAN_POINT('Ctrl Pts',(18.63905063298,64.6003205030525,36.));
#30889=CARTESIAN_POINT('Ctrl Pts',(18.5922306751828,64.6554154932839,36.));
#30890=CARTESIAN_POINT('Ctrl Pts',(18.5484215844064,64.7129027523719,36.));
#30891=CARTESIAN_POINT('Ctrl Pts',(18.5078817685123,64.7725530493182,36.));
#30892=CARTESIAN_POINT('Ctrl Pts',(18.4741933336872,64.8221222221587,36.));
#30893=CARTESIAN_POINT('Ctrl Pts',(18.4427631560478,64.8731857427967,36.));
#30894=CARTESIAN_POINT('Ctrl Pts',(18.4137671253403,64.9256185424461,36.));
#30895=CARTESIAN_POINT('Ctrl Pts',(18.4016609562457,64.9475098262932,36.));
#30896=CARTESIAN_POINT('Ctrl Pts',(18.389979418784,64.9696398359853,36.));
#30897=CARTESIAN_POINT('Ctrl Pts',(18.3787367554887,64.991999552123,36.));
#30898=CARTESIAN_POINT('Ctrl Pts',(18.3735359303309,65.0023430953879,36.));
#30899=CARTESIAN_POINT('Ctrl Pts',(18.3684290349839,65.0127357949179,36.));
#30900=CARTESIAN_POINT('Ctrl Pts',(18.3634175445956,65.0231767558657,36.));
#30901=CARTESIAN_POINT('Ctrl Pts',(18.358185554435,65.0340771070014,36.));
#30902=CARTESIAN_POINT('Ctrl Pts',(18.3530611587919,65.0450226072079,36.));
#30903=CARTESIAN_POINT('Ctrl Pts',(18.3480474161898,65.0560079490254,36.));
#30904=CARTESIAN_POINT('Ctrl Pts',(18.31950701775,65.1185412813777,36.));
#30905=CARTESIAN_POINT('Ctrl Pts',(18.2945275906019,65.1824076820533,36.));
#30906=CARTESIAN_POINT('Ctrl Pts',(18.2733325947284,65.2474026988709,36.));
#30907=CARTESIAN_POINT('Ctrl Pts',(18.2541301194199,65.3062875985454,36.));
#30908=CARTESIAN_POINT('Ctrl Pts',(18.2380343018762,65.36609948651,36.));
#30909=CARTESIAN_POINT('Ctrl Pts',(18.2252480174595,65.4266911450279,36.));
#30910=CARTESIAN_POINT('Ctrl Pts',(18.2101155115003,65.4984010807457,36.));
#30911=CARTESIAN_POINT('Ctrl Pts',(18.1996179357092,65.5712047291577,36.));
#30912=CARTESIAN_POINT('Ctrl Pts',(18.1936801509955,65.6446789881755,36.));
#30913=CARTESIAN_POINT('Ctrl Pts',(18.1923733282017,65.6608496378493,36.));
#30914=CARTESIAN_POINT('Ctrl Pts',(18.1912875955242,65.6770526886534,36.));
#30915=CARTESIAN_POINT('Ctrl Pts',(18.1904225212166,65.6932834657235,36.));
#30916=CARTESIAN_POINT('Ctrl Pts',(18.1895271920146,65.7100818939691,36.));
#30917=CARTESIAN_POINT('Ctrl Pts',(18.1888682156112,65.7269162162858,36.));
#30918=CARTESIAN_POINT('Ctrl Pts',(18.1884456743354,65.7437469754922,36.));
#30919=CARTESIAN_POINT('Ctrl Pts',(18.1867244318773,65.8123078925095,36.));
#30920=CARTESIAN_POINT('Ctrl Pts',(18.1889147956501,65.8808963864675,36.));
#30921=CARTESIAN_POINT('Ctrl Pts',(18.1948961812499,65.9491741310747,36.));
#30922=CARTESIAN_POINT('Ctrl Pts',(18.2008763308016,66.0174377661452,36.));
#30923=CARTESIAN_POINT('Ctrl Pts',(18.2106463891817,66.0853918518815,36.));
#30924=CARTESIAN_POINT('Ctrl Pts',(18.224135451783,66.1526832386545,36.));
#30925=CARTESIAN_POINT('Ctrl Pts',(18.2338954440545,66.2013718269017,36.));
#30926=CARTESIAN_POINT('Ctrl Pts',(18.2456034689683,66.2497132117657,36.));
#30927=CARTESIAN_POINT('Ctrl Pts',(18.2592468713223,66.297563972578,36.));
#30928=CARTESIAN_POINT('Ctrl Pts',(18.2694832221723,66.3334653675088,36.));
#30929=CARTESIAN_POINT('Ctrl Pts',(18.2808092805504,66.369090426564,36.));
#30930=CARTESIAN_POINT('Ctrl Pts',(18.2932236165998,66.4043744002987,36.));
#30931=CARTESIAN_POINT('Ctrl Pts',(18.2973531525319,66.4161113499661,36.));
#30932=CARTESIAN_POINT('Ctrl Pts',(18.301599913114,66.4278013646143,36.));
#30933=CARTESIAN_POINT('Ctrl Pts',(18.305963253358,66.4394418832697,36.));
#30934=CARTESIAN_POINT('Ctrl Pts',(18.32908720388,66.5011319561002,36.));
#30935=CARTESIAN_POINT('Ctrl Pts',(18.3554837407933,66.5614384947313,36.));
#30936=CARTESIAN_POINT('Ctrl Pts',(18.3851028692742,66.6200274070333,36.));
#30937=CARTESIAN_POINT('Ctrl Pts',(18.4059351993179,66.6612353567799,36.));
#30938=CARTESIAN_POINT('Ctrl Pts',(18.4283625607903,66.7015930886865,36.));
#30939=CARTESIAN_POINT('Ctrl Pts',(18.4523779599159,66.7409730135987,36.));
#30940=CARTESIAN_POINT('Ctrl Pts',(18.4600909786022,66.7536206525209,36.));
#30941=CARTESIAN_POINT('Ctrl Pts',(18.4679689605213,66.7661690371134,36.));
#30942=CARTESIAN_POINT('Ctrl Pts',(18.476008349553,66.7786083058229,36.));
#30943=CARTESIAN_POINT('Ctrl Pts',(18.5102528592992,66.8315945037637,36.));
#30944=CARTESIAN_POINT('Ctrl Pts',(18.5473531312327,66.882496911613,36.));
#30945=CARTESIAN_POINT('Ctrl Pts',(18.5872749277835,66.9310003064575,36.));
#30946=CARTESIAN_POINT('Ctrl Pts',(18.6240617394812,66.9756948194054,36.));
#30947=CARTESIAN_POINT('Ctrl Pts',(18.6632449234927,67.0183523994197,36.));
#30948=CARTESIAN_POINT('Ctrl Pts',(18.7048191306495,67.0586935104123,36.));
#30949=CARTESIAN_POINT('Ctrl Pts',(18.7126374799383,67.066279966487,36.));
#30950=CARTESIAN_POINT('Ctrl Pts',(18.7205404424604,67.0737843957438,36.));
#30951=CARTESIAN_POINT('Ctrl Pts',(18.7285264260868,67.0812061322332,36.));
#30952=CARTESIAN_POINT('Origin',(20.,66.,30.));
#30953=CARTESIAN_POINT('Origin',(-20.,66.,25.));
#30954=CARTESIAN_POINT('Ctrl Pts',(-20.7699020406705,64.5225674811446,25.));
#30955=CARTESIAN_POINT('Ctrl Pts',(-20.7181607868987,64.4874948453559,25.));
#30956=CARTESIAN_POINT('Ctrl Pts',(-20.6644430498644,64.4556772957763,25.));
#30957=CARTESIAN_POINT('Ctrl Pts',(-20.609080128741,64.4270507909171,25.));
#30958=CARTESIAN_POINT('Ctrl Pts',(-20.5739699369606,64.408896364539,25.));
#30959=CARTESIAN_POINT('Ctrl Pts',(-20.5381971797729,64.3920259834258,25.));
#30960=CARTESIAN_POINT('Ctrl Pts',(-20.501838755596,64.3764305264031,25.));
#30961=CARTESIAN_POINT('Ctrl Pts',(-20.4770533105217,64.3657991431075,25.));
#30962=CARTESIAN_POINT('Ctrl Pts',(-20.4519955812217,64.3557603488702,25.));
#30963=CARTESIAN_POINT('Ctrl Pts',(-20.4266886866948,64.3463128385714,25.));
#30964=CARTESIAN_POINT('Ctrl Pts',(-20.4131995684787,64.3412771127089,25.));
#30965=CARTESIAN_POINT('Ctrl Pts',(-20.3996397067877,64.3364095523361,25.));
#30966=CARTESIAN_POINT('Ctrl Pts',(-20.3860263063337,64.3317144816325,25.));
#30967=CARTESIAN_POINT('Ctrl Pts',(-20.3236619057568,64.3102058753821,25.));
#30968=CARTESIAN_POINT('Ctrl Pts',(-20.2601062052714,64.2922869409266,25.));
#30969=CARTESIAN_POINT('Ctrl Pts',(-20.1957090968652,64.277911135731,25.));
#30970=CARTESIAN_POINT('Ctrl Pts',(-20.1492566725938,64.2675412446177,25.));
#30971=CARTESIAN_POINT('Ctrl Pts',(-20.1023655335798,64.2590157983247,25.));
#30972=CARTESIAN_POINT('Ctrl Pts',(-20.055157896439,64.2523313578685,25.));
#30973=CARTESIAN_POINT('Ctrl Pts',(-20.0422585355377,64.2505048523476,25.));
#30974=CARTESIAN_POINT('Ctrl Pts',(-20.029335510413,64.2488158742319,25.));
#30975=CARTESIAN_POINT('Ctrl Pts',(-20.0163912478524,64.2472645140858,25.));
#30976=CARTESIAN_POINT('Ctrl Pts',(-20.0030607156547,64.2456668598138,25.));
#30977=CARTESIAN_POINT('Ctrl Pts',(-19.98971558118,64.2442161491718,25.));
#30978=CARTESIAN_POINT('Ctrl Pts',(-19.9763641001265,64.2429124587624,25.));
#30979=CARTESIAN_POINT('Ctrl Pts',(-19.9088329220123,64.2363184525327,25.));
#30980=CARTESIAN_POINT('Ctrl Pts',(-19.8410980617049,64.2334768385416,25.));
#30981=CARTESIAN_POINT('Ctrl Pts',(-19.7735141943155,64.234339667057,25.));
#30982=CARTESIAN_POINT('Ctrl Pts',(-19.7049517537314,64.2352149888032,25.));
#30983=CARTESIAN_POINT('Ctrl Pts',(-19.6365437003715,64.2399024721089,25.));
#30984=CARTESIAN_POINT('Ctrl Pts',(-19.5686388483405,64.2484003486578,25.));
#30985=CARTESIAN_POINT('Ctrl Pts',(-19.5265709671915,64.2536648864631,25.));
#30986=CARTESIAN_POINT('Ctrl Pts',(-19.4846958449925,64.26039280583,25.));
#30987=CARTESIAN_POINT('Ctrl Pts',(-19.4430950409565,64.2685936305935,25.));
#30988=CARTESIAN_POINT('Ctrl Pts',(-19.4090314604675,64.275308631923,25.));
#30989=CARTESIAN_POINT('Ctrl Pts',(-19.3751517611351,64.2830113026909,25.));
#30990=CARTESIAN_POINT('Ctrl Pts',(-19.3415010618013,64.2917108536401,25.));
#30991=CARTESIAN_POINT('Ctrl Pts',(-19.3277178667536,64.2952741557389,25.));
#30992=CARTESIAN_POINT('Ctrl Pts',(-19.3139706268034,64.2990055872543,25.));
#30993=CARTESIAN_POINT('Ctrl Pts',(-19.3002856997927,64.3028989400252,25.));
#30994=CARTESIAN_POINT('Ctrl Pts',(-19.232490402017,64.3221866578365,25.));
#30995=CARTESIAN_POINT('Ctrl Pts',(-19.1661047027307,64.3454735719371,25.));
#30996=CARTESIAN_POINT('Ctrl Pts',(-19.1014913319554,64.3727409719143,25.));
#30997=CARTESIAN_POINT('Ctrl Pts',(-19.0943245786266,64.3757654036567,25.));
#30998=CARTESIAN_POINT('Ctrl Pts',(-19.0871796217495,64.378838858274,25.));
#30999=CARTESIAN_POINT('Ctrl Pts',(-19.080056952154,64.3819613496012,25.));
#31000=CARTESIAN_POINT('Ctrl Pts',(-19.0183043681621,64.4090329279418,25.));
#31001=CARTESIAN_POINT('Ctrl Pts',(-18.9582262212172,64.4397861035812,25.));
#31002=CARTESIAN_POINT('Ctrl Pts',(-18.8999644475876,64.4739106753168,25.));
#31003=CARTESIAN_POINT('Ctrl Pts',(-18.8372885650046,64.5106206399824,25.));
#31004=CARTESIAN_POINT('Ctrl Pts',(-18.7767137054592,64.5512322190085,25.));
#31005=CARTESIAN_POINT('Ctrl Pts',(-18.7184364558154,64.5954203083505,25.));
#31006=CARTESIAN_POINT('Ctrl Pts',(-18.7079112053861,64.6034009647672,25.));
#31007=CARTESIAN_POINT('Ctrl Pts',(-18.6974609734778,64.6114984307375,25.));
#31008=CARTESIAN_POINT('Ctrl Pts',(-18.6870870232366,64.6197109799285,25.));
#31009=CARTESIAN_POINT('Ctrl Pts',(-18.6779109752736,64.6269752084551,25.));
#31010=CARTESIAN_POINT('Ctrl Pts',(-18.6688016088713,64.6343239571117,25.));
#31011=CARTESIAN_POINT('Ctrl Pts',(-18.6597615752311,64.6417539289658,25.));
#31012=CARTESIAN_POINT('Ctrl Pts',(-18.6048583606212,64.6868786879536,25.));
#31013=CARTESIAN_POINT('Ctrl Pts',(-18.5524872699802,64.7350141921525,25.));
#31014=CARTESIAN_POINT('Ctrl Pts',(-18.5027983210669,64.7858104381237,25.));
#31015=CARTESIAN_POINT('Ctrl Pts',(-18.4520616126594,64.8376777924631,25.));
#31016=CARTESIAN_POINT('Ctrl Pts',(-18.4041205870664,64.8923198235062,25.));
#31017=CARTESIAN_POINT('Ctrl Pts',(-18.3591551614209,64.9494152063453,25.));
#31018=CARTESIAN_POINT('Ctrl Pts',(-18.3139169717322,65.0068569345651,25.));
#31019=CARTESIAN_POINT('Ctrl Pts',(-18.2716898043235,65.0667825982523,25.));
#31020=CARTESIAN_POINT('Ctrl Pts',(-18.2326888228849,65.1289065313088,25.));
#31021=CARTESIAN_POINT('Ctrl Pts',(-18.2230617875061,65.1442412557014,25.));
#31022=CARTESIAN_POINT('Ctrl Pts',(-18.2136315088657,65.15971008858,25.));
#31023=CARTESIAN_POINT('Ctrl Pts',(-18.2044016076695,65.1753090388636,25.));
#31024=CARTESIAN_POINT('Ctrl Pts',(-18.1971519546457,65.1875612802137,25.));
#31025=CARTESIAN_POINT('Ctrl Pts',(-18.190025183174,65.1998953465914,25.));
#31026=CARTESIAN_POINT('Ctrl Pts',(-18.1830335133096,65.2122902250167,25.));
#31027=CARTESIAN_POINT('Ctrl Pts',(-18.1460182981017,65.2779110425448,25.));
#31028=CARTESIAN_POINT('Ctrl Pts',(-18.1127171633531,65.3453488100055,25.));
#31029=CARTESIAN_POINT('Ctrl Pts',(-18.0833108421231,65.4142572038605,25.));
#31030=CARTESIAN_POINT('Ctrl Pts',(-18.0538724456395,65.4832407602693,25.));
#31031=CARTESIAN_POINT('Ctrl Pts',(-18.0283365989439,65.5536989822687,25.));
#31032=CARTESIAN_POINT('Ctrl Pts',(-18.0069203644551,65.625322123177,25.));
#31033=CARTESIAN_POINT('Ctrl Pts',(-17.9859913623068,65.6953157941337,25.));
#31034=CARTESIAN_POINT('Ctrl Pts',(-17.9689961000931,65.7664228590063,25.));
#31035=CARTESIAN_POINT('Ctrl Pts',(-17.9561807640613,65.8383774456246,25.));
#31036=CARTESIAN_POINT('Ctrl Pts',(-17.9534319160524,65.853811471051,25.));
#31037=CARTESIAN_POINT('Ctrl Pts',(-17.9508755620075,65.869284549427,25.));
#31038=CARTESIAN_POINT('Ctrl Pts',(-17.9485144392445,65.8847941411762,25.));
#31039=CARTESIAN_POINT('Ctrl Pts',(-17.946501247731,65.8980182644525,25.));
#31040=CARTESIAN_POINT('Ctrl Pts',(-17.9446299912251,65.9112689334149,25.));
#31041=CARTESIAN_POINT('Ctrl Pts',(-17.9428998421776,65.9245444497166,25.));
#31042=CARTESIAN_POINT('Ctrl Pts',(-18.1825721112406,66.9586205879593,25.));
#31043=CARTESIAN_POINT('Ctrl Pts',(-18.2234186096542,67.0211003824849,25.));
#31044=CARTESIAN_POINT('Ctrl Pts',(-18.267861786798,67.0810294578375,25.));
#31045=CARTESIAN_POINT('Ctrl Pts',(-18.3155727964654,67.1382580395458,25.));
#31046=CARTESIAN_POINT('Ctrl Pts',(-18.362032339418,67.193985507242,25.));
#31047=CARTESIAN_POINT('Ctrl Pts',(-18.4115915278402,67.2471524989451,25.));
#31048=CARTESIAN_POINT('Ctrl Pts',(-18.463972782879,67.297583049384,25.));
#31049=CARTESIAN_POINT('Ctrl Pts',(-18.4756644509254,67.3088393137612,25.));
#31050=CARTESIAN_POINT('Ctrl Pts',(-18.4874983796361,67.3199605477055,25.));
#31051=CARTESIAN_POINT('Ctrl Pts',(-18.499466497088,67.330939853898,25.));
#31052=CARTESIAN_POINT('Ctrl Pts',(-18.5543876416691,67.3813233887536,25.));
#31053=CARTESIAN_POINT('Ctrl Pts',(-18.6120225103212,67.4286224459823,25.));
#31054=CARTESIAN_POINT('Ctrl Pts',(-18.6720549591814,67.4726645370967,25.));
#31055=CARTESIAN_POINT('Ctrl Pts',(-18.7141994128617,67.503583313595,25.));
#31056=CARTESIAN_POINT('Ctrl Pts',(-18.7575261800742,67.532896022068,25.));
#31057=CARTESIAN_POINT('Ctrl Pts',(-18.8019312037584,67.5605285808541,25.));
#31058=CARTESIAN_POINT('Ctrl Pts',(-18.8188066330934,67.5710298992737,25.));
#31059=CARTESIAN_POINT('Ctrl Pts',(-18.8358378192095,67.5812884311884,25.));
#31060=CARTESIAN_POINT('Ctrl Pts',(-18.8530191260934,67.5912996232851,25.));
#31061=CARTESIAN_POINT('Ctrl Pts',(-18.8694037899796,67.6008466279871,25.));
#31062=CARTESIAN_POINT('Ctrl Pts',(-18.8859302919879,67.6101714338832,25.));
#31063=CARTESIAN_POINT('Ctrl Pts',(-18.9025641525663,67.6192541843043,25.));
#31064=CARTESIAN_POINT('Ctrl Pts',(-18.9662810595884,67.6540461534543,25.));
#31065=CARTESIAN_POINT('Ctrl Pts',(-19.0316369227313,67.6853309714246,25.));
#31066=CARTESIAN_POINT('Ctrl Pts',(-19.0983400435049,67.7129470016749,25.));
#31067=CARTESIAN_POINT('Ctrl Pts',(-19.1636108196435,67.739970021099,25.));
#31068=CARTESIAN_POINT('Ctrl Pts',(-19.2301725386384,67.7634802778805,25.));
#31069=CARTESIAN_POINT('Ctrl Pts',(-19.2977604960306,67.7832780673405,25.));
#31070=CARTESIAN_POINT('Ctrl Pts',(-19.363866135499,67.8026416578796,25.));
#31071=CARTESIAN_POINT('Ctrl Pts',(-19.4309542545466,67.8184539478542,25.));
#31072=CARTESIAN_POINT('Ctrl Pts',(-19.4987732524779,67.8304795008119,25.));
#31073=CARTESIAN_POINT('Ctrl Pts',(-19.5208334683506,67.8343911819386,25.));
#31074=CARTESIAN_POINT('Ctrl Pts',(-19.5429709379166,67.8379018005825,25.));
#31075=CARTESIAN_POINT('Ctrl Pts',(-19.5651767076627,67.8410020802634,25.));
#31076=CARTESIAN_POINT('Ctrl Pts',(-19.577661186311,67.8427451126339,25.));
#31077=CARTESIAN_POINT('Ctrl Pts',(-19.5901685388999,67.8443584849207,25.));
#31078=CARTESIAN_POINT('Ctrl Pts',(-19.6026794702511,67.8458386692007,25.));
#31079=CARTESIAN_POINT('Ctrl Pts',(-19.6705100870722,67.8538637961796,25.));
#31080=CARTESIAN_POINT('Ctrl Pts',(-19.7385642439572,67.8579957018903,25.));
#31081=CARTESIAN_POINT('Ctrl Pts',(-19.8065962194624,67.8580563450086,25.));
#31082=CARTESIAN_POINT('Ctrl Pts',(-19.8163931634452,67.8580650779202,25.));
#31083=CARTESIAN_POINT('Ctrl Pts',(-19.8261896412384,67.8579892951331,25.));
#31084=CARTESIAN_POINT('Ctrl Pts',(-19.8359849096261,67.8578283749833,25.));
#31085=CARTESIAN_POINT('Ctrl Pts',(-19.905349147844,67.8566888346295,25.));
#31086=CARTESIAN_POINT('Ctrl Pts',(-19.9746541960652,67.8512840088951,25.));
#31087=CARTESIAN_POINT('Ctrl Pts',(-20.0435750455083,67.8417871266218,25.));
#31088=CARTESIAN_POINT('Ctrl Pts',(-20.1078703307363,67.8329276195282,25.));
#31089=CARTESIAN_POINT('Ctrl Pts',(-20.1718317704019,67.8205059706896,25.));
#31090=CARTESIAN_POINT('Ctrl Pts',(-20.2351749893643,67.8046283759774,25.));
#31091=CARTESIAN_POINT('Ctrl Pts',(-20.2490396161921,67.8011530722398,25.));
#31092=CARTESIAN_POINT('Ctrl Pts',(-20.2628745263258,67.7975120871324,25.));
#31093=CARTESIAN_POINT('Ctrl Pts',(-20.2766765599084,67.793706356147,25.));
#31094=CARTESIAN_POINT('Ctrl Pts',(-20.2877369911298,67.7906565863026,25.));
#31095=CARTESIAN_POINT('Ctrl Pts',(-20.2987757638788,67.787501080294,25.));
#31096=CARTESIAN_POINT('Ctrl Pts',(-20.3097781968535,67.7842444451942,25.));
#31097=CARTESIAN_POINT('Ctrl Pts',(-20.3753404535977,67.7648385240647,25.));
#31098=CARTESIAN_POINT('Ctrl Pts',(-20.4397363417765,67.7418126009015,25.));
#31099=CARTESIAN_POINT('Ctrl Pts',(-20.502663400315,67.7153486959875,25.));
#31100=CARTESIAN_POINT('Ctrl Pts',(-20.5652990969205,67.6890073230124,25.));
#31101=CARTESIAN_POINT('Ctrl Pts',(-20.6264804265539,67.6592590290608,25.));
#31102=CARTESIAN_POINT('Ctrl Pts',(-20.6858793170701,67.6262417671952,25.));
#31103=CARTESIAN_POINT('Ctrl Pts',(-20.7440054791047,67.5939319597818,25.));
#31104=CARTESIAN_POINT('Ctrl Pts',(-20.8004254400109,67.5584910682472,25.));
#31105=CARTESIAN_POINT('Ctrl Pts',(-20.8547918303173,67.52001896722,25.));
#31106=CARTESIAN_POINT('Ctrl Pts',(-20.8662882857036,67.5118835587336,25.));
#31107=CARTESIAN_POINT('Ctrl Pts',(-20.8776927475808,67.503612519805,25.));
#31108=CARTESIAN_POINT('Ctrl Pts',(-20.8890016529758,67.4952066661362,25.));
#31109=CARTESIAN_POINT('Ctrl Pts',(-20.8996328294733,67.4873045650181,25.));
#31110=CARTESIAN_POINT('Ctrl Pts',(-20.9101807913445,67.4792822117678,25.));
#31111=CARTESIAN_POINT('Ctrl Pts',(-20.9206259991789,67.4711535452534,25.));
#31112=CARTESIAN_POINT('Ctrl Pts',(-20.9721934579281,67.431022732941,25.));
#31113=CARTESIAN_POINT('Ctrl Pts',(-21.0213543413904,67.3882344350529,25.));
#31114=CARTESIAN_POINT('Ctrl Pts',(-21.0678175681512,67.34292066402,25.));
#31115=CARTESIAN_POINT('Ctrl Pts',(-21.1133971413376,67.2984686858183,25.));
#31116=CARTESIAN_POINT('Ctrl Pts',(-21.1563812744484,67.2515857193821,25.));
#31117=CARTESIAN_POINT('Ctrl Pts',(-21.196452662785,67.2023706262552,25.));
#31118=CARTESIAN_POINT('Ctrl Pts',(-21.2352229187693,67.1547535648547,25.));
#31119=CARTESIAN_POINT('Ctrl Pts',(-21.2712668558046,67.1049527951087,25.));
#31120=CARTESIAN_POINT('Ctrl Pts',(-21.3042504198252,67.0530424950224,25.));
#31121=CARTESIAN_POINT('Ctrl Pts',(-21.3097028004787,67.0444614115553,25.));
#31122=CARTESIAN_POINT('Ctrl Pts',(-21.3150714402185,67.0358226586051,25.));
#31123=CARTESIAN_POINT('Ctrl Pts',(-21.3203546922529,67.0271265453092,25.));
#31124=CARTESIAN_POINT('Ctrl Pts',(-21.3260102782519,67.0178175787331,25.));
#31125=CARTESIAN_POINT('Ctrl Pts',(-21.3315680165281,67.0084428810478,25.));
#31126=CARTESIAN_POINT('Ctrl Pts',(-21.3370275036536,66.9990041127266,25.));
#31127=CARTESIAN_POINT('Origin',(-20.,66.,37.5459252805377));
#31128=CARTESIAN_POINT('Ctrl Pts',(-22.0565719673595,66.0014962574405,35.7959252805377));
#31129=CARTESIAN_POINT('Ctrl Pts',(-22.0573889181502,66.099669215357,35.7905876687522));
#31130=CARTESIAN_POINT('Ctrl Pts',(-22.0063638713597,66.8783588803798,35.7482056843029));
#31131=CARTESIAN_POINT('Ctrl Pts',(-21.0114091850863,68.208181319433,35.6687793271896));
#31132=CARTESIAN_POINT('Ctrl Pts',(-18.6935441236518,68.0471886637504,35.5576462091982));
#31133=CARTESIAN_POINT('Ctrl Pts',(-17.5714219821268,66.0128602375846,35.4465130912065));
#31134=CARTESIAN_POINT('Ctrl Pts',(-18.6720184527178,63.9665951580731,35.335379973215));
#31135=CARTESIAN_POINT('Ctrl Pts',(-20.988041711498,63.7814657159201,35.2242468552234));
#31136=CARTESIAN_POINT('Ctrl Pts',(-22.0019739085829,65.1068137933338,35.144428624331));
#31137=CARTESIAN_POINT('Ctrl Pts',(-22.057280493024,65.8929627817184,35.1016547661024));
#31138=CARTESIAN_POINT('Ctrl Pts',(-22.0563748666992,65.9983937868295,35.0959252805377));
#31139=CARTESIAN_POINT('Ctrl Pts',(-22.0526727182563,65.9976789726186,35.8540747194623));
#31140=CARTESIAN_POINT('Ctrl Pts',(-22.0491245254771,66.4678277317379,35.8286277343138));
#31141=CARTESIAN_POINT('Ctrl Pts',(-21.6566322253174,67.6294023146612,35.7661363765015));
#31142=CARTESIAN_POINT('Ctrl Pts',(-19.7281828950178,68.4128315562992,35.6666006460254));
#31143=CARTESIAN_POINT('Ctrl Pts',(-17.8254683675795,67.0812973613349,35.5554675280337));
#31144=CARTESIAN_POINT('Ctrl Pts',(-17.9121447447308,64.7590835038729,35.4443344100422));
#31145=CARTESIAN_POINT('Ctrl Pts',(-19.9101226209547,63.5731232768953,35.3332012920507));
#31146=CARTESIAN_POINT('Ctrl Pts',(-21.7210100698093,64.4741603064334,35.2364480618573));
#31147=CARTESIAN_POINT('Ctrl Pts',(-22.0499160183042,65.5818790726719,35.1767392043279));
#31148=CARTESIAN_POINT('Ctrl Pts',(-22.0520910576133,66.0011644713934,35.1540747194623));
#31149=CARTESIAN_POINT('Ctrl Pts',(-18.7309291201477,67.0793586530486,36.));
#31150=CARTESIAN_POINT('Ctrl Pts',(-18.372032101712,66.6573805147568,35.9629556273362));
#31151=CARTESIAN_POINT('Ctrl Pts',(-18.1147584132015,65.4342585881912,35.8888668820084));
#31152=CARTESIAN_POINT('Ctrl Pts',(-19.454738309765,64.1066458935492,35.7777337640169));
#31153=CARTESIAN_POINT('Ctrl Pts',(-21.294007127745,64.5163018976528,35.6666006460253));
#31154=CARTESIAN_POINT('Ctrl Pts',(-21.9488058936235,66.2817526841271,35.5554675280338));
#31155=CARTESIAN_POINT('Ctrl Pts',(-20.8200548496672,67.7904027634385,35.4443344100422));
#31156=CARTESIAN_POINT('Ctrl Pts',(-18.9407200438028,67.6598692365535,35.3332012920506));
#31157=CARTESIAN_POINT('Ctrl Pts',(-18.0308986602863,66.0104271350851,35.2220681740591));
#31158=CARTESIAN_POINT('Ctrl Pts',(-18.9232669386679,64.351306744543,35.1109350560675));
#31159=CARTESIAN_POINT('Ctrl Pts',(-20.8011084031418,64.2012030089904,34.999801938076));
#31160=CARTESIAN_POINT('Ctrl Pts',(-21.9457415640057,65.697395124653,34.8886688200844));
#31161=CARTESIAN_POINT('Ctrl Pts',(-21.3095566464544,67.4705601638215,34.7775357020928));
#31162=CARTESIAN_POINT('Ctrl Pts',(-19.4748133482442,67.8978021178438,34.6664025841013));
#31163=CARTESIAN_POINT('Ctrl Pts',(-18.1207418428944,66.5881051616333,34.5552694661097));
#31164=CARTESIAN_POINT('Ctrl Pts',(-18.4866412203222,64.7401490647328,34.4441363481182));
#31165=CARTESIAN_POINT('Ctrl Pts',(-20.2376261931116,64.0452592090235,34.3330032301266));
#31166=CARTESIAN_POINT('Ctrl Pts',(-21.7711262834811,65.1394245223657,34.2218701121351));
#31167=CARTESIAN_POINT('Ctrl Pts',(-21.6836219072211,67.0212226559639,34.1107369941435));
#31168=CARTESIAN_POINT('Ctrl Pts',(-20.0552004852982,67.9683574838607,33.9996038761519));
#31169=CARTESIAN_POINT('Ctrl Pts',(-18.3762574113062,67.1139741369633,33.8884707581604));
#31170=CARTESIAN_POINT('Ctrl Pts',(-18.1834274619919,65.240037780099,33.7773376401688));
#31171=CARTESIAN_POINT('Ctrl Pts',(-19.6531962002549,64.0616487758754,33.6662045221773));
#31172=CARTESIAN_POINT('Ctrl Pts',(-21.4403734255104,64.6573150961213,33.5550714041857));
#31173=CARTESIAN_POINT('Ctrl Pts',(-21.9092641994935,66.4818594922784,33.4439382861941));
#31174=CARTESIAN_POINT('Ctrl Pts',(-20.6307212300429,67.8653871131315,33.3328051682026));
#31175=CARTESIAN_POINT('Ctrl Pts',(-18.7749173659869,67.5416390282116,33.221672050211));
#31176=CARTESIAN_POINT('Ctrl Pts',(-18.0403573473244,65.8069222258068,33.1105389322195));
#31177=CARTESIAN_POINT('Ctrl Pts',(-19.0993394151928,64.248917802084,32.9994058142279));
#31178=CARTESIAN_POINT('Ctrl Pts',(-20.9826414999224,64.2935727276805,32.8882726962364));
#31179=CARTESIAN_POINT('Ctrl Pts',(-21.9665914075352,65.9000170572955,32.7771395782447));
#31180=CARTESIAN_POINT('Ctrl Pts',(-21.1506394546859,67.5979697113295,32.6660064602533));
#31181=CARTESIAN_POINT('Ctrl Pts',(-19.2815769841816,67.833397590097,32.5548733422616));
#31182=CARTESIAN_POINT('Ctrl Pts',(-18.0700435346081,66.3908278325732,32.4437402242701));
#31183=CARTESIAN_POINT('Ctrl Pts',(-18.6248822045078,64.590557059849,32.3326071062785));
#31184=CARTESIAN_POINT('Ctrl Pts',(-20.4382828049508,64.0802639410825,32.221473988287));
#31185=CARTESIAN_POINT('Ctrl Pts',(-21.8505497316599,65.3269888235133,32.1103408702954));
#31186=CARTESIAN_POINT('Ctrl Pts',(-21.5691207070261,67.189680024126,31.9992077523039));
#31187=CARTESIAN_POINT('Ctrl Pts',(-19.8515706513329,67.9635292413093,31.8880746343123));
#31188=CARTESIAN_POINT('Ctrl Pts',(-18.269868977662,66.9402792130885,31.7769415163208));
#31189=CARTESIAN_POINT('Ctrl Pts',(-18.2716513129284,65.0564486400198,31.6658083983292));
#31190=CARTESIAN_POINT('Ctrl Pts',(-19.8552863937441,64.0361934094247,31.5546752803376));
#31191=CARTESIAN_POINT('Ctrl Pts',(-21.5713690628773,64.8132912651982,31.4435421623461));
#31192=CARTESIAN_POINT('Ctrl Pts',(-21.8492729171815,66.6765116634631,31.3324090443545));
#31193=CARTESIAN_POINT('Ctrl Pts',(-20.4346494110085,67.9205619600867,31.2212759263629));
#31194=CARTESIAN_POINT('Ctrl Pts',(-18.6222176562464,67.406838358257,31.1101428083714));
#31195=CARTESIAN_POINT('Ctrl Pts',(-18.0707865314722,65.6055209183322,30.9990096903798));
#31196=CARTESIAN_POINT('Ctrl Pts',(-19.2850475061968,64.165246260495,30.8878765723883));
#31197=CARTESIAN_POINT('Ctrl Pts',(-21.1536611435061,64.4042104402565,30.7767434543968));
#31198=CARTESIAN_POINT('Ctrl Pts',(-21.9663986946184,66.1037040347599,30.6656103364051));
#31199=CARTESIAN_POINT('Ctrl Pts',(-20.9794107637176,67.7082836149003,30.5544772184136));
#31200=CARTESIAN_POINT('Ctrl Pts',(-19.0960275526304,67.7493747932959,30.4433441004221));
#31201=CARTESIAN_POINT('Ctrl Pts',(-18.0399955053847,66.1893693061462,30.3322109824305));
#31202=CARTESIAN_POINT('Ctrl Pts',(-18.7778367166361,64.4560455765083,30.2210778644389));
#31203=CARTESIAN_POINT('Ctrl Pts',(-20.6342498687002,64.1358097047038,30.1099447464473));
#31204=CARTESIAN_POINT('Ctrl Pts',(-21.9101725770983,65.5217541649695,29.9988116284558));
#31205=CARTESIAN_POINT('Ctrl Pts',(-21.4378301592761,67.3454080370277,29.8876785104642));
#31206=CARTESIAN_POINT('Ctrl Pts',(-19.6495289872407,67.9376915188538,29.7765453924727));
#31207=CARTESIAN_POINT('Ctrl Pts',(-18.1819926804873,66.75652345583,29.6654122744811));
#31208=CARTESIAN_POINT('Ctrl Pts',(-18.3783682286227,64.8829553495575,29.5542791564896));
#31209=CARTESIAN_POINT('Ctrl Pts',(-20.0589250007271,64.0317504738189,29.443146038498));
#31210=CARTESIAN_POINT('Ctrl Pts',(-21.6855512929007,64.9819650339878,29.3320129205065));
#31211=CARTESIAN_POINT('Ctrl Pts',(-21.7694946991591,66.8639252645168,29.2208798025149));
#31212=CARTESIAN_POINT('Ctrl Pts',(-20.2339269101145,67.9551870891929,29.1097466845233));
#31213=CARTESIAN_POINT('Ctrl Pts',(-18.4842600056596,67.2569847344258,28.9986135665318));
#31214=CARTESIAN_POINT('Ctrl Pts',(-18.1218580029699,65.408340476275,28.8874804485402));
#31215=CARTESIAN_POINT('Ctrl Pts',(-19.4784054789109,64.1012063017294,28.7763473305487));
#31216=CARTESIAN_POINT('Ctrl Pts',(-21.3123367903127,64.5319228556325,28.6652142125571));
#31217=CARTESIAN_POINT('Ctrl Pts',(-21.9451658181481,66.3062813950144,28.5540810945656));
#31218=CARTESIAN_POINT('Ctrl Pts',(-20.7977025282328,67.8003191465602,28.442947976574));
#31219=CARTESIAN_POINT('Ctrl Pts',(-18.9201504872152,67.6466339553042,28.3318148585824));
#31220=CARTESIAN_POINT('Ctrl Pts',(-18.0309192227571,65.9858845572708,28.2206817405909));
#31221=CARTESIAN_POINT('Ctrl Pts',(-18.9438681879035,64.3380541680053,28.1095486225993));
#31222=CARTESIAN_POINT('Ctrl Pts',(-20.8234305564082,64.2113020177245,27.9984155046077));
#31223=CARTESIAN_POINT('Ctrl Pts',(-21.9493568698083,65.7216366633037,27.8872823866162));
#31224=CARTESIAN_POINT('Ctrl Pts',(-21.291155049959,67.4867403908715,27.7761492686246));
#31225=CARTESIAN_POINT('Ctrl Pts',(-19.4512373091435,67.891120795242,27.6650161506331));
#31226=CARTESIAN_POINT('Ctrl Pts',(-18.1135687818421,66.5646730138986,27.5538830326415));
#31227=CARTESIAN_POINT('Ctrl Pts',(-18.5024363551,64.7214142651596,27.4427499146499));
#31228=CARTESIAN_POINT('Ctrl Pts',(-20.2619331187203,64.0483675051169,27.3316167966584));
#31229=CARTESIAN_POINT('Ctrl Pts',(-21.7816983844559,65.1615316208422,27.2204836786668));
#31230=CARTESIAN_POINT('Ctrl Pts',(-21.6707831578744,67.0420949970833,27.1093505606753));
#31231=CARTESIAN_POINT('Ctrl Pts',(-20.0307014315933,67.9688920192891,26.9982174426837));
#31232=CARTESIAN_POINT('Ctrl Pts',(-18.3625205312278,67.093681563121,26.8870843246922));
#31233=CARTESIAN_POINT('Ctrl Pts',(-18.193025322136,65.217490708422,26.7759512067006));
#31234=CARTESIAN_POINT('Ctrl Pts',(-19.6773443984712,64.0574831268864,26.664818088709));
#31235=CARTESIAN_POINT('Ctrl Pts',(-21.4569707037066,64.6753435036645,26.5536849707175));
#31236=CARTESIAN_POINT('Ctrl Pts',(-21.9031198303154,66.5055815255925,26.4425518527259));
#31237=CARTESIAN_POINT('Ctrl Pts',(-20.6074592701813,67.8730916715933,26.3314187347344));
#31238=CARTESIAN_POINT('Ctrl Pts',(-18.7558271036352,67.5262741254895,26.2202856167428));
#31239=CARTESIAN_POINT('Ctrl Pts',(-18.0429128818286,65.7825513633931,26.1091524987513));
#31240=CARTESIAN_POINT('Ctrl Pts',(-19.1211979533711,64.2378442836875,25.9980193807597));
#31241=CARTESIAN_POINT('Ctrl Pts',(-21.0038049577023,64.3059351985902,25.8868862627681));
#31242=CARTESIAN_POINT('Ctrl Pts',(-21.9676747832011,65.9244934704524,25.7757531447766));
#31243=CARTESIAN_POINT('Ctrl Pts',(-21.1306818475489,67.6121730972753,25.664620026785));
#31244=CARTESIAN_POINT('Ctrl Pts',(-19.2587832804016,67.8242989299444,25.5534869087934));
#31245=CARTESIAN_POINT('Ctrl Pts',(-18.0653972468034,66.3668134340257,25.4423537908019));
#31246=CARTESIAN_POINT('Ctrl Pts',(-18.642392926108,64.5734885052306,25.3312206728103));
#31247=CARTESIAN_POINT('Ctrl Pts',(-20.4624083103757,64.0859969852348,25.2200875548188));
#31248=CARTESIAN_POINT('Ctrl Pts',(-21.8582430905867,65.3498099340575,25.1089544368272));
#31249=CARTESIAN_POINT('Ctrl Pts',(-21.5552778968737,67.2096324841655,24.9978213188357));
#31250=CARTESIAN_POINT('Ctrl Pts',(-19.82486994896,67.9604919410323,24.8866882008441));
#31251=CARTESIAN_POINT('Ctrl Pts',(-18.7848659979775,67.2672324081111,24.8125994555164));
#31252=CARTESIAN_POINT('Ctrl Pts',(-18.5264217726374,66.7772536316049,24.7755550828525));
#31253=CARTESIAN_POINT('Ctrl Pts',(-18.6322193753412,67.1633123698098,36.0748149723825));
#31254=CARTESIAN_POINT('Ctrl Pts',(-18.2454069475584,66.7085123024942,36.0377705997186));
#31255=CARTESIAN_POINT('Ctrl Pts',(-17.9681222253528,65.3902545918245,35.9636818543909));
#31256=CARTESIAN_POINT('Ctrl Pts',(-19.4123272489249,63.9593787048971,35.8525487363994));
#31257=CARTESIAN_POINT('Ctrl Pts',(-21.3946564416527,64.4008982087198,35.7414156184078));
#31258=CARTESIAN_POINT('Ctrl Pts',(-22.1003861839689,66.3036677213329,35.6302825004163));
#31259=CARTESIAN_POINT('Ctrl Pts',(-20.8838396281403,67.9296622821033,35.5191493824247));
#31260=CARTESIAN_POINT('Ctrl Pts',(-18.8583280704192,67.7889757122858,35.4080162644331));
#31261=CARTESIAN_POINT('Ctrl Pts',(-17.8777397675665,66.0112381692516,35.2968831464416));
#31262=CARTESIAN_POINT('Ctrl Pts',(-18.8395174433512,64.223069549053,35.18575002845));
#31263=CARTESIAN_POINT('Ctrl Pts',(-20.8634195059272,64.0612905779669,35.0746169104585));
#31264=CARTESIAN_POINT('Ctrl Pts',(-22.0970835073845,65.6738581808173,34.9634837924669));
#31265=CARTESIAN_POINT('Ctrl Pts',(-21.4114154192253,67.5849419692808,34.8523506744753));
#31266=CARTESIAN_POINT('Ctrl Pts',(-19.4339637462294,68.0454152777701,34.7412175564838));
#31267=CARTESIAN_POINT('Ctrl Pts',(-17.9745710528634,66.6338486353397,34.6300844384922));
#31268=CARTESIAN_POINT('Ctrl Pts',(-18.3689304909105,64.6421564574729,34.5189513205007));
#31269=CARTESIAN_POINT('Ctrl Pts',(-20.2561090227579,63.8932172957598,34.4078182025091));
#31270=CARTESIAN_POINT('Ctrl Pts',(-21.9088864560908,65.0724880043724,34.2966850845175));
#31271=CARTESIAN_POINT('Ctrl Pts',(-21.8145758921015,67.1006544901989,34.185551966526));
#31272=CARTESIAN_POINT('Ctrl Pts',(-20.0594940404522,68.1214585186447,34.0744188485344));
#31273=CARTESIAN_POINT('Ctrl Pts',(-18.2499609064333,67.2006202845713,33.9632857305429));
#31274=CARTESIAN_POINT('Ctrl Pts',(-18.0421324291486,65.180927073219,33.8521526125513));
#31275=CARTESIAN_POINT('Ctrl Pts',(-19.6262214149106,63.9108816613538,33.7410194945598));
#31276=CARTESIAN_POINT('Ctrl Pts',(-21.5524072728828,64.5528795706346,33.6298863765682));
#31277=CARTESIAN_POINT('Ctrl Pts',(-22.0577688928814,66.51933905963,33.5187532585766));
#31278=CARTESIAN_POINT('Ctrl Pts',(-20.6797794289583,68.0104789979313,33.4076201405851));
#31279=CARTESIAN_POINT('Ctrl Pts',(-18.6796290758763,67.6615494268146,33.2964870225935));
#31280=CARTESIAN_POINT('Ctrl Pts',(-17.8879341618047,65.7919044217416,33.185353904602));
#31281=CARTESIAN_POINT('Ctrl Pts',(-19.0292850329711,64.1127166807475,33.0742207866104));
#31282=CARTESIAN_POINT('Ctrl Pts',(-21.059072448921,64.1608449161331,32.9630876686188));
#31283=CARTESIAN_POINT('Ctrl Pts',(-22.119555074938,65.8922402727864,32.8519545506273));
#31284=CARTESIAN_POINT('Ctrl Pts',(-21.2401374714945,67.7222615731301,32.7408214326357));
#31285=CARTESIAN_POINT('Ctrl Pts',(-19.2256972428052,67.9760012942087,32.6296883146441));
#31286=CARTESIAN_POINT('Ctrl Pts',(-17.9199293737595,66.4212268561652,32.5185551966526));
#31287=CARTESIAN_POINT('Ctrl Pts',(-18.5179240126315,64.4809290200364,32.407422078661));
#31288=CARTESIAN_POINT('Ctrl Pts',(-20.4723729290854,63.9309447348192,32.2962889606695));
#31289=CARTESIAN_POINT('Ctrl Pts',(-21.9944875484231,65.2746412655183,32.1851558426779));
#31290=CARTESIAN_POINT('Ctrl Pts',(-21.691168661179,67.282214659856,32.0740227246864));
#31291=CARTESIAN_POINT('Ctrl Pts',(-19.840025651474,68.1162547300167,31.9628896066948));
#31292=CARTESIAN_POINT('Ctrl Pts',(-18.135297462069,67.0134151762913,31.8517564887032));
#31293=CARTESIAN_POINT('Ctrl Pts',(-18.1372184293551,64.9830581655917,31.7406233707117));
#31294=CARTESIAN_POINT('Ctrl Pts',(-19.8440304084636,63.8834463481829,31.6294902527201));
#31295=CARTESIAN_POINT('Ctrl Pts',(-21.6935918966495,64.7209877396572,31.5183571347286));
#31296=CARTESIAN_POINT('Ctrl Pts',(-21.9931114218943,66.7291314932291,31.407224016737));
#31297=CARTESIAN_POINT('Ctrl Pts',(-20.4684569257203,68.0699454058618,31.2960908987455));
#31298=CARTESIAN_POINT('Ctrl Pts',(-18.5150522128422,67.5162638107925,31.1849577807539));
#31299=CARTESIAN_POINT('Ctrl Pts',(-17.9207301617462,65.5748378965238,31.0738246627623));
#31300=CARTESIAN_POINT('Ctrl Pts',(-19.2294377058835,64.0225370735738,30.9626915447708));
#31301=CARTESIAN_POINT('Ctrl Pts',(-21.2433941906325,64.2800881530714,30.8515584267792));
#31302=CARTESIAN_POINT('Ctrl Pts',(-22.1193473725962,66.1117702499486,30.7404253087876));
#31303=CARTESIAN_POINT('Ctrl Pts',(-21.0555904224601,67.8411558148388,30.6292921907961));
#31304=CARTESIAN_POINT('Ctrl Pts',(-19.0257155700544,67.8854431108016,30.5181590728045));
#31305=CARTESIAN_POINT('Ctrl Pts',(-17.8875441753963,66.2040986614413,30.407025954813));
#31306=CARTESIAN_POINT('Ctrl Pts',(-18.6827754968666,64.3359550838847,30.2958928368214));
#31307=CARTESIAN_POINT('Ctrl Pts',(-20.6835825290558,63.9908109097266,30.1847597188299));
#31308=CARTESIAN_POINT('Ctrl Pts',(-22.0587479251069,65.4845556718986,30.0736266008383));
#31309=CARTESIAN_POINT('Ctrl Pts',(-21.5496661885715,67.4500553708401,29.9624934828468));
#31310=CARTESIAN_POINT('Ctrl Pts',(-19.6222689619886,68.0884073207655,29.8513603648552));
#31311=CARTESIAN_POINT('Ctrl Pts',(-18.0405860487425,66.8153666918152,29.7402272468636));
#31312=CARTESIAN_POINT('Ctrl Pts',(-18.2522359054689,64.7960703739953,29.6290941288721));
#31313=CARTESIAN_POINT('Ctrl Pts',(-20.0635082528345,63.8786578361033,29.5179610108805));
#31314=CARTESIAN_POINT('Ctrl Pts',(-21.8166553475456,64.9027811418235,29.406827892889));
#31315=CARTESIAN_POINT('Ctrl Pts',(-21.9071279653252,66.9311223326602,29.2956947748974));
#31316=CARTESIAN_POINT('Ctrl Pts',(-20.2521220054139,68.1072637160285,29.1845616569058));
#31317=CARTESIAN_POINT('Ctrl Pts',(-18.3663640627225,67.3547544053958,29.0734285389143));
#31318=CARTESIAN_POINT('Ctrl Pts',(-17.9757740291112,65.362320540331,28.9622954209227));
#31319=CARTESIAN_POINT('Ctrl Pts',(-19.4378352768154,63.9535160155744,28.8511623029312));
#31320=CARTESIAN_POINT('Ctrl Pts',(-21.4144118057657,64.4177341821886,28.7400291849396));
#31321=CARTESIAN_POINT('Ctrl Pts',(-22.0964629793736,66.3301043026398,28.628896066948));
#31322=CARTESIAN_POINT('Ctrl Pts',(-20.8597487182789,67.9403499725357,28.5177629489565));
#31323=CARTESIAN_POINT('Ctrl Pts',(-18.8361585908377,67.7747109761374,28.4066298309649));
#31324=CARTESIAN_POINT('Ctrl Pts',(-17.8777619294091,65.9847866424326,28.2954967129734));
#31325=CARTESIAN_POINT('Ctrl Pts',(-18.8617210806702,64.2087861723696,28.1843635949818));
#31326=CARTESIAN_POINT('Ctrl Pts',(-20.8874779011068,64.072175098835,28.0732304769902));
#31327=CARTESIAN_POINT('Ctrl Pts',(-22.1009800156942,65.6999852533116,27.9620973589987));
#31328=CARTESIAN_POINT('Ctrl Pts',(-21.3915825260838,67.6023807123903,27.8509642410071));
#31329=CARTESIAN_POINT('Ctrl Pts',(-19.4085539365804,68.0382142744638,27.7398311230156));
#31330=CARTESIAN_POINT('Ctrl Pts',(-17.9668400631429,66.6085939090873,27.628698005024));
#31331=CARTESIAN_POINT('Ctrl Pts',(-18.3859541888425,64.6219644443474,27.5175648870324));
#31332=CARTESIAN_POINT('Ctrl Pts',(-20.2823065680806,63.8965673585811,27.4064317690409));
#31333=CARTESIAN_POINT('Ctrl Pts',(-21.9202808668403,65.0963146175614,27.2952986510493));
#31334=CARTESIAN_POINT('Ctrl Pts',(-21.8007385305482,67.1231503052298,27.1841655330578));
#31335=CARTESIAN_POINT('Ctrl Pts',(-20.0330894230963,68.1220346308335,27.0730324150662));
#31336=CARTESIAN_POINT('Ctrl Pts',(-18.2351555565408,67.178749331761,26.9618992970747));
#31337=CARTESIAN_POINT('Ctrl Pts',(-18.0524768215319,65.1566262652246,26.8507661790831));
#31338=CARTESIAN_POINT('Ctrl Pts',(-19.6522478868477,63.9063920035524,26.7396330610915));
#31339=CARTESIAN_POINT('Ctrl Pts',(-21.5702955058407,64.5723102477722,26.6284999431));
#31340=CARTESIAN_POINT('Ctrl Pts',(-22.0511466078334,66.5449062190847,26.5173668251084));
#31341=CARTESIAN_POINT('Ctrl Pts',(-20.654708127981,68.0187828255213,26.4062337071169));
#31342=CARTESIAN_POINT('Ctrl Pts',(-18.6590539516821,67.644989424866,26.2951005891253));
#31343=CARTESIAN_POINT('Ctrl Pts',(-17.8906884686255,65.7656379665382,26.1839674711338));
#31344=CARTESIAN_POINT('Ctrl Pts',(-19.0528437525653,64.1007818517715,26.0728343531422));
#31345=CARTESIAN_POINT('Ctrl Pts',(-21.0818820239902,64.1741689537826,25.9617012351506));
#31346=CARTESIAN_POINT('Ctrl Pts',(-22.1207227167685,65.9186204885875,25.8505681171591));
#31347=CARTESIAN_POINT('Ctrl Pts',(-21.2186275394726,67.7375697142351,25.7394349991675));
#31348=CARTESIAN_POINT('Ctrl Pts',(-19.2011306193885,67.9661949301477,25.6283018811759));
#31349=CARTESIAN_POINT('Ctrl Pts',(-17.9149216925206,66.395344590984,25.5171687631844));
#31350=CARTESIAN_POINT('Ctrl Pts',(-18.5367967376375,64.4625328542518,25.4060356451928));
#31351=CARTESIAN_POINT('Ctrl Pts',(-20.4983749431605,63.9371237015234,25.2949025272012));
#31352=CARTESIAN_POINT('Ctrl Pts',(-22.0027793053657,65.2992374274278,25.1837694092097));
#31353=CARTESIAN_POINT('Ctrl Pts',(-21.6762491418536,67.3037190444335,25.0726362912181));
#31354=CARTESIAN_POINT('Ctrl Pts',(-19.8112481387675,68.1129811851452,24.9615031732266));
#31355=CARTESIAN_POINT('Ctrl Pts',(-18.6903515235305,67.3657991545403,24.8874144278989));
#31356=CARTESIAN_POINT('Ctrl Pts',(-18.4118052188384,66.837709283723,24.850370055235));
#31357=CARTESIAN_POINT('Ctrl Pts',(-18.5335096305348,67.247266086571,36.149629944765));
#31358=CARTESIAN_POINT('Ctrl Pts',(-18.1187817934049,66.7596440902317,36.1125855721011));
#31359=CARTESIAN_POINT('Ctrl Pts',(-17.8214860375041,65.3462505954579,36.0384968267734));
#31360=CARTESIAN_POINT('Ctrl Pts',(-19.3699161880848,63.8121115162452,35.9273637087819));
#31361=CARTESIAN_POINT('Ctrl Pts',(-21.4953057555605,64.2854945197867,35.8162305907903));
#31362=CARTESIAN_POINT('Ctrl Pts',(-22.2519664743143,66.3255827585387,35.7050974727988));
#31363=CARTESIAN_POINT('Ctrl Pts',(-20.9476244066133,68.0689218007681,35.5939643548072));
#31364=CARTESIAN_POINT('Ctrl Pts',(-18.7759360970355,67.9180821880181,35.4828312368156));
#31365=CARTESIAN_POINT('Ctrl Pts',(-17.7245808748466,66.0120492034181,35.3716981188241));
#31366=CARTESIAN_POINT('Ctrl Pts',(-18.7557679480345,64.0948323535631,35.2605650008325));
#31367=CARTESIAN_POINT('Ctrl Pts',(-20.9257306087126,63.9213781469436,35.149431882841));
#31368=CARTESIAN_POINT('Ctrl Pts',(-22.2484254507633,65.6503212369814,35.0382987648494));
#31369=CARTESIAN_POINT('Ctrl Pts',(-21.5132741919963,67.6993237747403,34.9271656468578));
#31370=CARTESIAN_POINT('Ctrl Pts',(-19.3931141442146,68.1930284376963,34.8160325288663));
#31371=CARTESIAN_POINT('Ctrl Pts',(-17.8284002628325,66.6795921090463,34.7048994108747));
#31372=CARTESIAN_POINT('Ctrl Pts',(-18.2512197614988,64.5441638502129,34.5937662928831));
#31373=CARTESIAN_POINT('Ctrl Pts',(-20.2745918524042,63.7411753824961,34.4826331748916));
#31374=CARTESIAN_POINT('Ctrl Pts',(-22.0466466287005,65.0055514863792,34.3715000569));
#31375=CARTESIAN_POINT('Ctrl Pts',(-21.9455298769819,67.1800863244337,34.2603669389085));
#31376=CARTESIAN_POINT('Ctrl Pts',(-20.0637875956061,68.2745595534289,34.1492338209169));
#31377=CARTESIAN_POINT('Ctrl Pts',(-18.1236644015604,67.2872664321791,34.0381007029254));
#31378=CARTESIAN_POINT('Ctrl Pts',(-17.9008373963053,65.1218163663389,33.9269675849338));
#31379=CARTESIAN_POINT('Ctrl Pts',(-19.5992466295663,63.7601145468323,33.8158344669422));
#31380=CARTESIAN_POINT('Ctrl Pts',(-21.6644411202551,64.4484440451478,33.7047013489507));
#31381=CARTESIAN_POINT('Ctrl Pts',(-22.2062735862694,66.5568186269816,33.5935682309591));
#31382=CARTESIAN_POINT('Ctrl Pts',(-20.7288376278737,68.1555708827312,33.4824351129676));
#31383=CARTESIAN_POINT('Ctrl Pts',(-18.5843407857658,67.7814598254175,33.371301994976));
#31384=CARTESIAN_POINT('Ctrl Pts',(-17.735510976285,65.7768866176765,33.2601688769845));
#31385=CARTESIAN_POINT('Ctrl Pts',(-18.9592306507495,63.9765155594109,33.1490357589929));
#31386=CARTESIAN_POINT('Ctrl Pts',(-21.1355033979196,64.0281171045857,33.0379026410013));
#31387=CARTESIAN_POINT('Ctrl Pts',(-22.2725187423409,65.8844634882773,32.9267695230097));
#31388=CARTESIAN_POINT('Ctrl Pts',(-21.329635488303,67.8465534349308,32.8156364050182));
#31389=CARTESIAN_POINT('Ctrl Pts',(-19.1698175014287,68.1186049983203,32.7045032870266));
#31390=CARTESIAN_POINT('Ctrl Pts',(-17.769815212911,66.4516258797572,32.5933701690351));
#31391=CARTESIAN_POINT('Ctrl Pts',(-18.4109658207552,64.3713009802238,32.4822370510435));
#31392=CARTESIAN_POINT('Ctrl Pts',(-20.50646305322,63.7816255285558,32.371103933052));
#31393=CARTESIAN_POINT('Ctrl Pts',(-22.1384253651864,65.2222937075232,32.2599708150604));
#31394=CARTESIAN_POINT('Ctrl Pts',(-21.8132166153319,67.3747492955862,32.1488376970689));
#31395=CARTESIAN_POINT('Ctrl Pts',(-19.8284806516152,68.2689802187239,32.0377045790773));
#31396=CARTESIAN_POINT('Ctrl Pts',(-18.000725946476,67.0865511394943,31.9265714610858));
#31397=CARTESIAN_POINT('Ctrl Pts',(-18.0027855457819,64.9096676911634,31.8154383430942));
#31398=CARTESIAN_POINT('Ctrl Pts',(-19.832774423183,63.7306992869412,31.7043052251026));
#31399=CARTESIAN_POINT('Ctrl Pts',(-21.8158147304217,64.6286842141161,31.593172107111));
#31400=CARTESIAN_POINT('Ctrl Pts',(-22.136949926607,66.7817513229953,31.4820389891195));
#31401=CARTESIAN_POINT('Ctrl Pts',(-20.5022644404321,68.2193288516369,31.3709058711279));
#31402=CARTESIAN_POINT('Ctrl Pts',(-18.407886769438,67.625689263328,31.2597727531364));
#31403=CARTESIAN_POINT('Ctrl Pts',(-17.7706737920203,65.5441548747155,31.1486396351448));
#31404=CARTESIAN_POINT('Ctrl Pts',(-19.1738279055702,63.8798278866525,31.0375065171532));
#31405=CARTESIAN_POINT('Ctrl Pts',(-21.333127237759,64.1559658658865,30.9263733991617));
#31406=CARTESIAN_POINT('Ctrl Pts',(-22.2722960505739,66.1198364651373,30.8152402811701));
#31407=CARTESIAN_POINT('Ctrl Pts',(-21.1317700812027,67.9740280147772,30.7041071631786));
#31408=CARTESIAN_POINT('Ctrl Pts',(-18.9554035874784,68.0215114283074,30.592974045187));
#31409=CARTESIAN_POINT('Ctrl Pts',(-17.735092845408,66.2188280167362,30.4818409271955));
#31410=CARTESIAN_POINT('Ctrl Pts',(-18.5877142770972,64.2158645912613,30.3707078092039));
#31411=CARTESIAN_POINT('Ctrl Pts',(-20.7329151894114,63.8458121147493,30.2595746912123));
#31412=CARTESIAN_POINT('Ctrl Pts',(-22.2073232731155,65.4473571788279,30.1484415732208));
#31413=CARTESIAN_POINT('Ctrl Pts',(-21.6615022178669,67.5547027046525,30.0373084552292));
#31414=CARTESIAN_POINT('Ctrl Pts',(-19.5950089367365,68.2391231226771,29.9261753372376));
#31415=CARTESIAN_POINT('Ctrl Pts',(-17.8991794169977,66.8742099278003,29.8150422192461));
#31416=CARTESIAN_POINT('Ctrl Pts',(-18.126103582315,64.7091853984332,29.7039091012545));
#31417=CARTESIAN_POINT('Ctrl Pts',(-20.0680915049419,63.7255651983877,29.592775983263));
#31418=CARTESIAN_POINT('Ctrl Pts',(-21.9477594021904,64.8235972496592,29.4816428652714));
#31419=CARTESIAN_POINT('Ctrl Pts',(-22.0447612314913,66.9983194008037,29.3705097472799));
#31420=CARTESIAN_POINT('Ctrl Pts',(-20.2703171007134,68.2593403428639,29.2593766292883));
#31421=CARTESIAN_POINT('Ctrl Pts',(-18.2484681197853,67.4525240763659,29.1482435112968));
#31422=CARTESIAN_POINT('Ctrl Pts',(-17.8296900552526,65.316300604387,29.0371103933052));
#31423=CARTESIAN_POINT('Ctrl Pts',(-19.3972650747199,63.8058257294195,28.9259772753136));
#31424=CARTESIAN_POINT('Ctrl Pts',(-21.5164868212187,64.3035455087446,28.8148441573221));
#31425=CARTESIAN_POINT('Ctrl Pts',(-22.2477601405991,66.3539272102652,28.7037110393305));
#31426=CARTESIAN_POINT('Ctrl Pts',(-20.9217949083251,68.0803807985112,28.592577921339));
#31427=CARTESIAN_POINT('Ctrl Pts',(-18.7521666944602,67.9027879969706,28.4814448033474));
#31428=CARTESIAN_POINT('Ctrl Pts',(-17.7246046360611,65.9836887275945,28.3703116853559));
#31429=CARTESIAN_POINT('Ctrl Pts',(-18.7795739734368,64.0795181767337,28.2591785673643));
#31430=CARTESIAN_POINT('Ctrl Pts',(-20.9515252458054,63.9330481799455,28.1480454493727));
#31431=CARTESIAN_POINT('Ctrl Pts',(-22.2526031615802,65.6783338433195,28.0369123313812));
#31432=CARTESIAN_POINT('Ctrl Pts',(-21.4920100022086,67.7180210339092,27.9257792133896));
#31433=CARTESIAN_POINT('Ctrl Pts',(-19.3658705640173,68.1853077536856,27.8146460953981));
#31434=CARTESIAN_POINT('Ctrl Pts',(-17.8201113444436,66.652514804276,27.7035129774064));
#31435=CARTESIAN_POINT('Ctrl Pts',(-18.269472022585,64.5225146235353,27.592379859415));
#31436=CARTESIAN_POINT('Ctrl Pts',(-20.3026800174408,63.7447672120453,27.4812467414234));
#31437=CARTESIAN_POINT('Ctrl Pts',(-22.0588633492247,65.0310976142806,27.3701136234318));
#31438=CARTESIAN_POINT('Ctrl Pts',(-21.930693903222,67.2042056133763,27.2589805054403));
#31439=CARTESIAN_POINT('Ctrl Pts',(-20.0354774145993,68.2751772423777,27.1478473874487));
#31440=CARTESIAN_POINT('Ctrl Pts',(-18.1077905818539,67.2638171004012,27.0367142694571));
#31441=CARTESIAN_POINT('Ctrl Pts',(-17.9119283209277,65.0957618220271,26.9255811514656));
#31442=CARTESIAN_POINT('Ctrl Pts',(-19.6271513752242,63.7553008802185,26.814448033474));
#31443=CARTESIAN_POINT('Ctrl Pts',(-21.6836203079748,64.4692769918797,26.7033149154825));
#31444=CARTESIAN_POINT('Ctrl Pts',(-22.1991733853515,66.5842309125769,26.5921817974909));
#31445=CARTESIAN_POINT('Ctrl Pts',(-20.7019569857807,68.1644739794492,26.4810486794993));
#31446=CARTESIAN_POINT('Ctrl Pts',(-18.5622807997289,67.7637047242426,26.3699155615078));
#31447=CARTESIAN_POINT('Ctrl Pts',(-17.7384640554224,65.7487245696832,26.2587824435162));
#31448=CARTESIAN_POINT('Ctrl Pts',(-18.9844895517596,63.9637194198555,26.1476493255246));
#31449=CARTESIAN_POINT('Ctrl Pts',(-21.1599590902781,64.0424027089751,26.0365162075331));
#31450=CARTESIAN_POINT('Ctrl Pts',(-22.2737706503358,65.9127475067224,25.9253830895415));
#31451=CARTESIAN_POINT('Ctrl Pts',(-21.3065732313963,67.862966331195,25.81424997155));
#31452=CARTESIAN_POINT('Ctrl Pts',(-19.1434779583753,68.1080909303509,25.7031168535584));
#31453=CARTESIAN_POINT('Ctrl Pts',(-17.7644461382379,66.4238757479422,25.5919837355669));
#31454=CARTESIAN_POINT('Ctrl Pts',(-18.431200549167,64.3515772032731,25.4808506175753));
#31455=CARTESIAN_POINT('Ctrl Pts',(-20.5343415759454,63.7882504178119,25.3697174995837));
#31456=CARTESIAN_POINT('Ctrl Pts',(-22.1473155201447,65.2486649207981,25.2585843815922));
#31457=CARTESIAN_POINT('Ctrl Pts',(-21.7972203868335,67.3978056047015,25.1474512636006));
#31458=CARTESIAN_POINT('Ctrl Pts',(-19.7976263285751,68.2654704292581,25.0363181456091));
#31459=CARTESIAN_POINT('Ctrl Pts',(-18.5958370490835,67.4643659009695,24.9622294002814));
#31460=CARTESIAN_POINT('Ctrl Pts',(-18.2971886650395,66.8981649358411,24.9251850276175));
#31461=CARTESIAN_POINT('Ctrl Pts',(-18.4347998857283,67.3312198033323,36.2244449171475));
#31462=CARTESIAN_POINT('Ctrl Pts',(-17.9921566392513,66.8107758779691,36.1874005444836));
#31463=CARTESIAN_POINT('Ctrl Pts',(-17.6748498496554,65.3022465990912,36.1133117991559));
#31464=CARTESIAN_POINT('Ctrl Pts',(-19.3275051272447,63.6648443275931,36.0021786811644));
#31465=CARTESIAN_POINT('Ctrl Pts',(-21.5959550694682,64.1700908308537,35.8910455631727));
#31466=CARTESIAN_POINT('Ctrl Pts',(-22.4035467646596,66.3474977957444,35.7799124451813));
#31467=CARTESIAN_POINT('Ctrl Pts',(-21.0114091850863,68.208181319433,35.6687793271896));
#31468=CARTESIAN_POINT('Ctrl Pts',(-18.6935441236518,68.0471886637504,35.5576462091982));
#31469=CARTESIAN_POINT('Ctrl Pts',(-17.5714219821268,66.0128602375846,35.4465130912065));
#31470=CARTESIAN_POINT('Ctrl Pts',(-18.6720184527178,63.9665951580731,35.335379973215));
#31471=CARTESIAN_POINT('Ctrl Pts',(-20.988041711498,63.7814657159201,35.2242468552234));
#31472=CARTESIAN_POINT('Ctrl Pts',(-22.3997673941421,65.6267842931457,35.1131137372319));
#31473=CARTESIAN_POINT('Ctrl Pts',(-21.6151329647672,67.8137055801995,35.0019806192403));
#31474=CARTESIAN_POINT('Ctrl Pts',(-19.3522645421998,68.3406415976227,34.8908475012488));
#31475=CARTESIAN_POINT('Ctrl Pts',(-17.6822294728015,66.7253355827527,34.7797143832572));
#31476=CARTESIAN_POINT('Ctrl Pts',(-18.1335090320871,64.4461712429531,34.6685812652656));
#31477=CARTESIAN_POINT('Ctrl Pts',(-20.2930746820505,63.5891334692323,34.5574481472741));
#31478=CARTESIAN_POINT('Ctrl Pts',(-22.1844068013102,64.9386149683859,34.4463150292826));
#31479=CARTESIAN_POINT('Ctrl Pts',(-22.0764838618623,67.2595181586686,34.3351819112909));
#31480=CARTESIAN_POINT('Ctrl Pts',(-20.0680811507602,68.427660588213,34.2240487932995));
#31481=CARTESIAN_POINT('Ctrl Pts',(-17.9973678966875,67.3739125797871,34.1129156753078));
#31482=CARTESIAN_POINT('Ctrl Pts',(-17.7595423634621,65.0627056594589,34.0017825573163));
#31483=CARTESIAN_POINT('Ctrl Pts',(-19.572271844222,63.6093474323109,33.8906494393247));
#31484=CARTESIAN_POINT('Ctrl Pts',(-21.7764749676275,64.344008519661,33.7795163213332));
#31485=CARTESIAN_POINT('Ctrl Pts',(-22.3547782796574,66.5942981943332,33.6683832033416));
#31486=CARTESIAN_POINT('Ctrl Pts',(-20.7778958267891,68.3006627675311,33.5572500853501));
#31487=CARTESIAN_POINT('Ctrl Pts',(-18.4890524956552,67.9013702240204,33.4461169673585));
#31488=CARTESIAN_POINT('Ctrl Pts',(-17.5830877907652,65.7618688136113,33.334983849367));
#31489=CARTESIAN_POINT('Ctrl Pts',(-18.8891762685279,63.8403144380744,33.2238507313753));
#31490=CARTESIAN_POINT('Ctrl Pts',(-21.2119343469181,63.8953892930382,33.1127176133839));
#31491=CARTESIAN_POINT('Ctrl Pts',(-22.4254824097437,65.8766867037682,33.0015844953922));
#31492=CARTESIAN_POINT('Ctrl Pts',(-21.4191335051115,67.9708452967313,32.8904513774008));
#31493=CARTESIAN_POINT('Ctrl Pts',(-19.1139377600523,68.2612087024321,32.7793182594091));
#31494=CARTESIAN_POINT('Ctrl Pts',(-17.6197010520624,66.4820249033491,32.6681851414176));
#31495=CARTESIAN_POINT('Ctrl Pts',(-18.304007628879,64.2616729404111,32.557052023426));
#31496=CARTESIAN_POINT('Ctrl Pts',(-20.5405531773546,63.6323063222924,32.4459189054345));
#31497=CARTESIAN_POINT('Ctrl Pts',(-22.2823631819496,65.1699461495282,32.3347857874429));
#31498=CARTESIAN_POINT('Ctrl Pts',(-21.9352645694849,67.4672839313162,32.2236526694514));
#31499=CARTESIAN_POINT('Ctrl Pts',(-19.8169356517564,68.4217057074312,32.1125195514598));
#31500=CARTESIAN_POINT('Ctrl Pts',(-17.866154430883,67.1596871026972,32.0013864334682));
#31501=CARTESIAN_POINT('Ctrl Pts',(-17.8683526622086,64.8362772167352,31.8902533154766));
#31502=CARTESIAN_POINT('Ctrl Pts',(-19.8215184379026,63.5779522256995,31.7791201974851));
#31503=CARTESIAN_POINT('Ctrl Pts',(-21.9380375641939,64.5363806885751,31.6679870794935));
#31504=CARTESIAN_POINT('Ctrl Pts',(-22.2807884313198,66.8343711527615,31.556853961502));
#31505=CARTESIAN_POINT('Ctrl Pts',(-20.5360719551439,68.3687122974119,31.4457208435104));
#31506=CARTESIAN_POINT('Ctrl Pts',(-18.3007213260338,67.7351147158636,31.3345877255189));
#31507=CARTESIAN_POINT('Ctrl Pts',(-17.6206174222944,65.513471852907,31.2234546075273));
#31508=CARTESIAN_POINT('Ctrl Pts',(-19.1182181052569,63.7371186997313,31.1123214895358));
#31509=CARTESIAN_POINT('Ctrl Pts',(-21.4228602848854,64.0318435787015,31.0011883715442));
#31510=CARTESIAN_POINT('Ctrl Pts',(-22.4252447285517,66.127902680326,30.8900552535526));
#31511=CARTESIAN_POINT('Ctrl Pts',(-21.2079497399452,68.1069002147157,30.778922135561));
#31512=CARTESIAN_POINT('Ctrl Pts',(-18.8850916049024,68.1575797458132,30.6677890175695));
#31513=CARTESIAN_POINT('Ctrl Pts',(-17.5826415154197,66.2335573720312,30.5566558995779));
#31514=CARTESIAN_POINT('Ctrl Pts',(-18.4926530573277,64.0957740986377,30.4455227815864));
#31515=CARTESIAN_POINT('Ctrl Pts',(-20.7822478497669,63.7008133197721,30.3343896635948));
#31516=CARTESIAN_POINT('Ctrl Pts',(-22.3558986211242,65.410158685757,30.2232565456033));
#31517=CARTESIAN_POINT('Ctrl Pts',(-21.7733382471624,67.659350038465,30.1121234276117));
#31518=CARTESIAN_POINT('Ctrl Pts',(-19.5677489114844,68.3898389245888,30.0009903096202));
#31519=CARTESIAN_POINT('Ctrl Pts',(-17.7577727852529,66.9330531637854,29.8898571916286));
#31520=CARTESIAN_POINT('Ctrl Pts',(-17.9999712591612,64.6223004228711,29.7787240736371));
#31521=CARTESIAN_POINT('Ctrl Pts',(-20.0726747570493,63.5724725606719,29.6675909556455));
#31522=CARTESIAN_POINT('Ctrl Pts',(-22.0788634568353,64.7444133574949,29.5564578376539));
#31523=CARTESIAN_POINT('Ctrl Pts',(-22.1823944976574,67.0655164689471,29.4453247196624));
#31524=CARTESIAN_POINT('Ctrl Pts',(-20.288512196013,68.4114169696994,29.3341916016708));
#31525=CARTESIAN_POINT('Ctrl Pts',(-18.1305721768482,67.5502937473358,29.2230584836793));
#31526=CARTESIAN_POINT('Ctrl Pts',(-17.683606081394,65.270280668443,29.1119253656876));
#31527=CARTESIAN_POINT('Ctrl Pts',(-19.3566948726244,63.6581354432645,29.0007922476961));
#31528=CARTESIAN_POINT('Ctrl Pts',(-21.6185618366717,64.1893568353006,28.8896591297046));
#31529=CARTESIAN_POINT('Ctrl Pts',(-22.3990573018246,66.3777501178906,28.778526011713));
#31530=CARTESIAN_POINT('Ctrl Pts',(-20.9838410983712,68.2204116244866,28.6673928937214));
#31531=CARTESIAN_POINT('Ctrl Pts',(-18.6681747980826,68.0308650178038,28.5562597757299));
#31532=CARTESIAN_POINT('Ctrl Pts',(-17.5714473427131,65.9825908127564,28.4451266577384));
#31533=CARTESIAN_POINT('Ctrl Pts',(-18.6974268662034,63.9502501810978,28.3339935397467));
#31534=CARTESIAN_POINT('Ctrl Pts',(-21.015572590504,63.7939212610561,28.2228604217552));
#31535=CARTESIAN_POINT('Ctrl Pts',(-22.4042263074661,65.6566824333273,28.1117273037636));
#31536=CARTESIAN_POINT('Ctrl Pts',(-21.5924374783333,67.8336613554281,28.0005941857721));
#31537=CARTESIAN_POINT('Ctrl Pts',(-19.3231871914542,68.3324012329073,27.8894610677805));
#31538=CARTESIAN_POINT('Ctrl Pts',(-17.6733826257443,66.6964356994646,27.778327949789));
#31539=CARTESIAN_POINT('Ctrl Pts',(-18.1529898563275,64.4230648027232,27.6671948317974));
#31540=CARTESIAN_POINT('Ctrl Pts',(-20.3230534668011,63.5929670655095,27.5560617138059));
#31541=CARTESIAN_POINT('Ctrl Pts',(-22.1974458316091,64.9658806109998,27.4449285958143));
#31542=CARTESIAN_POINT('Ctrl Pts',(-22.0606492758959,67.2852609215228,27.3337954778227));
#31543=CARTESIAN_POINT('Ctrl Pts',(-20.0378654061023,68.4283198539221,27.2226623598312));
#31544=CARTESIAN_POINT('Ctrl Pts',(-17.980425607167,67.3488848690413,27.1115292418396));
#31545=CARTESIAN_POINT('Ctrl Pts',(-17.7713798203235,65.0348973788296,27.0003961238481));
#31546=CARTESIAN_POINT('Ctrl Pts',(-19.6020548636007,63.6042097568846,26.8892630058565));
#31547=CARTESIAN_POINT('Ctrl Pts',(-21.7969451101088,64.3662437359872,26.778129887865));
#31548=CARTESIAN_POINT('Ctrl Pts',(-22.3472001628695,66.6235556060692,26.6669967698734));
#31549=CARTESIAN_POINT('Ctrl Pts',(-20.7492058435804,68.3101651333771,26.5558636518819));
#31550=CARTESIAN_POINT('Ctrl Pts',(-18.4655076477758,67.8824200236192,26.4447305338902));
#31551=CARTESIAN_POINT('Ctrl Pts',(-17.5862396422193,65.7318111728283,26.3335974158987));
#31552=CARTESIAN_POINT('Ctrl Pts',(-18.9161353509539,63.8266569879394,26.2224642979071));
#31553=CARTESIAN_POINT('Ctrl Pts',(-21.2380361565659,63.9106364641676,26.1113311799156));
#31554=CARTESIAN_POINT('Ctrl Pts',(-22.4268185839031,65.9068745248573,26.000198061924));
#31555=CARTESIAN_POINT('Ctrl Pts',(-21.3945189233201,67.988362948155,25.8890649439324));
#31556=CARTESIAN_POINT('Ctrl Pts',(-19.0858252973621,68.2499869305541,25.777931825941));
#31557=CARTESIAN_POINT('Ctrl Pts',(-17.6139705839552,66.4524069049006,25.6667987079493));
#31558=CARTESIAN_POINT('Ctrl Pts',(-18.3256043606965,64.2406215522943,25.5556655899578));
#31559=CARTESIAN_POINT('Ctrl Pts',(-20.5703082087302,63.6393771341005,25.4445324719662));
#31560=CARTESIAN_POINT('Ctrl Pts',(-22.2918517349237,65.1980924141684,25.3333993539747));
#31561=CARTESIAN_POINT('Ctrl Pts',(-21.9181916318134,67.4918921649695,25.2222662359831));
#31562=CARTESIAN_POINT('Ctrl Pts',(-19.7840045183826,68.4179596733709,25.1111331179915));
#31563=CARTESIAN_POINT('Ctrl Pts',(-18.5013225746364,67.5629326473987,25.0370443726639));
#31564=CARTESIAN_POINT('Ctrl Pts',(-18.1825721112405,66.9586205879592,25.));
#31565=CARTESIAN_POINT('Ctrl Pts',(-18.7309291201477,67.0793586530486,36.));
#31566=CARTESIAN_POINT('Ctrl Pts',(-18.6855998783608,67.037071281398,36.));
#31567=CARTESIAN_POINT('Ctrl Pts',(-18.6430006396261,66.9922147972381,36.));
#31568=CARTESIAN_POINT('Ctrl Pts',(-18.6031299258315,66.9451342242319,36.));
#31569=CARTESIAN_POINT('Ctrl Pts',(-18.5606276474992,66.8949462183622,36.));
#31570=CARTESIAN_POINT('Ctrl Pts',(-18.5212252344066,66.8422306107827,36.));
#31571=CARTESIAN_POINT('Ctrl Pts',(-18.4849497284356,66.7873506353329,36.));
#31572=CARTESIAN_POINT('Ctrl Pts',(-18.4532086607109,66.7393306568143,36.));
#31573=CARTESIAN_POINT('Ctrl Pts',(-18.4238618746648,66.6896523585445,36.));
#31574=CARTESIAN_POINT('Ctrl Pts',(-18.3969503791963,66.6385315246993,36.));
#31575=CARTESIAN_POINT('Ctrl Pts',(-18.3834500893461,66.6128864959755,36.));
#31576=CARTESIAN_POINT('Ctrl Pts',(-18.3705630201934,66.5868780860802,36.));
#31577=CARTESIAN_POINT('Ctrl Pts',(-18.3582966902476,66.5605316957194,36.));
#31578=CARTESIAN_POINT('Ctrl Pts',(-18.3526877469073,66.5484844565366,36.));
#31579=CARTESIAN_POINT('Ctrl Pts',(-18.3472080157328,66.5363648649589,36.));
#31580=CARTESIAN_POINT('Ctrl Pts',(-18.3418667280703,66.5241953083072,36.));
#31581=CARTESIAN_POINT('Ctrl Pts',(-18.3149477441457,66.462863262446,36.));
#31582=CARTESIAN_POINT('Ctrl Pts',(-18.2914899255357,66.4001557545952,36.));
#31583=CARTESIAN_POINT('Ctrl Pts',(-18.2715167789656,66.336430550718,36.));
#31584=CARTESIAN_POINT('Ctrl Pts',(-18.2511893221814,66.2715749044961,36.));
#31585=CARTESIAN_POINT('Ctrl Pts',(-18.2344707080506,66.2056642940756,36.));
#31586=CARTESIAN_POINT('Ctrl Pts',(-18.2214250327644,66.1390393524431,36.));
#31587=CARTESIAN_POINT('Ctrl Pts',(-18.2105137796048,66.0833150155311,36.));
#31588=CARTESIAN_POINT('Ctrl Pts',(-18.2021724702928,66.0270900300921,36.));
#31589=CARTESIAN_POINT('Ctrl Pts',(-18.1964634312906,65.9705514121168,36.));
#31590=CARTESIAN_POINT('Ctrl Pts',(-18.1938337965334,65.9445092157172,36.));
#31591=CARTESIAN_POINT('Ctrl Pts',(-18.1917629610617,65.9184003657446,36.));
#31592=CARTESIAN_POINT('Ctrl Pts',(-18.1902588173323,65.8922427368446,36.));
#31593=CARTESIAN_POINT('Ctrl Pts',(-18.1896014517996,65.8808109013618,36.));
#31594=CARTESIAN_POINT('Ctrl Pts',(-18.1890524419704,65.8693699541686,36.));
#31595=CARTESIAN_POINT('Ctrl Pts',(-18.1886127813066,65.857935522043,36.));
#31596=CARTESIAN_POINT('Ctrl Pts',(-18.1859163883022,65.7878093421686,36.));
#31597=CARTESIAN_POINT('Ctrl Pts',(-18.1873207361518,65.7177968496091,36.));
#31598=CARTESIAN_POINT('Ctrl Pts',(-18.1928804564878,65.6482588440327,36.));
#31599=CARTESIAN_POINT('Ctrl Pts',(-18.1978500052571,65.5861023884661,36.));
#31600=CARTESIAN_POINT('Ctrl Pts',(-18.2061399035841,65.5243240681204,36.));
#31601=CARTESIAN_POINT('Ctrl Pts',(-18.2178222762375,65.4631694203924,36.));
#31602=CARTESIAN_POINT('Ctrl Pts',(-18.2305527201426,65.3965283505056,36.));
#31603=CARTESIAN_POINT('Ctrl Pts',(-18.2473105590726,65.3306270439365,36.));
#31604=CARTESIAN_POINT('Ctrl Pts',(-18.2678505607771,65.2656790787157,36.));
#31605=CARTESIAN_POINT('Ctrl Pts',(-18.2757799272864,65.2406062365768,36.));
#31606=CARTESIAN_POINT('Ctrl Pts',(-18.2842735067606,65.2156755188473,36.));
#31607=CARTESIAN_POINT('Ctrl Pts',(-18.2933192003048,65.1908995337231,36.));
#31608=CARTESIAN_POINT('Ctrl Pts',(-18.2972865790838,65.1800329575862,36.));
#31609=CARTESIAN_POINT('Ctrl Pts',(-18.3013600630916,65.1691967138699,36.));
#31610=CARTESIAN_POINT('Ctrl Pts',(-18.3055335461828,65.1584044028859,36.));
#31611=CARTESIAN_POINT('Ctrl Pts',(-18.3307563695742,65.0931800931219,36.));
#31612=CARTESIAN_POINT('Ctrl Pts',(-18.3596700145117,65.0294411884365,36.));
#31613=CARTESIAN_POINT('Ctrl Pts',(-18.3919618229701,64.9674064946292,36.));
#31614=CARTESIAN_POINT('Ctrl Pts',(-18.4250016473144,64.903934812971,36.));
#31615=CARTESIAN_POINT('Ctrl Pts',(-18.461578255366,64.8422463908931,36.));
#31616=CARTESIAN_POINT('Ctrl Pts',(-18.5014128922655,64.7825793081379,36.));
#31617=CARTESIAN_POINT('Ctrl Pts',(-18.5319056213951,64.7369051829538,36.));
#31618=CARTESIAN_POINT('Ctrl Pts',(-18.5643086534008,64.6924154573582,36.));
#31619=CARTESIAN_POINT('Ctrl Pts',(-18.5985165024735,64.6492230243908,36.));
#31620=CARTESIAN_POINT('Ctrl Pts',(-18.6198130829703,64.6223329640543,36.));
#31621=CARTESIAN_POINT('Ctrl Pts',(-18.6418095092061,64.5959458391794,36.));
#31622=CARTESIAN_POINT('Ctrl Pts',(-18.6644832354918,64.570090580138,36.));
#31623=CARTESIAN_POINT('Ctrl Pts',(-18.6771613061568,64.5556335474889,36.));
#31624=CARTESIAN_POINT('Ctrl Pts',(-18.6900556017823,64.5413382714678,36.));
#31625=CARTESIAN_POINT('Ctrl Pts',(-18.7031384975848,64.5272352145414,36.));
#31626=CARTESIAN_POINT('Ctrl Pts',(-18.7540097800711,64.4723971569995,36.));
#31627=CARTESIAN_POINT('Ctrl Pts',(-18.8077776043746,64.4204040417605,36.));
#31628=CARTESIAN_POINT('Ctrl Pts',(-18.8641570225205,64.3715197896026,36.));
#31629=CARTESIAN_POINT('Ctrl Pts',(-18.9063166280107,64.3349649464802,36.));
#31630=CARTESIAN_POINT('Ctrl Pts',(-18.9499377420014,64.3001487169774,36.));
#31631=CARTESIAN_POINT('Ctrl Pts',(-18.9949176029387,64.2671912029343,36.));
#31632=CARTESIAN_POINT('Ctrl Pts',(-19.0089812491819,64.2568865286001,36.));
#31633=CARTESIAN_POINT('Ctrl Pts',(-19.0231778186317,64.2467636385533,36.));
#31634=CARTESIAN_POINT('Ctrl Pts',(-19.0375044116818,64.2368264306734,36.));
#31635=CARTESIAN_POINT('Ctrl Pts',(-19.0512937814086,64.2272618515002,36.));
#31636=CARTESIAN_POINT('Ctrl Pts',(-19.0651965653016,64.2178742367791,36.));
#31637=CARTESIAN_POINT('Ctrl Pts',(-19.0792048040081,64.2086698030378,36.));
#31638=CARTESIAN_POINT('Ctrl Pts',(-19.142158533753,64.1673046145694,36.));
#31639=CARTESIAN_POINT('Ctrl Pts',(-19.2072697134705,64.1296151054152,36.));
#31640=CARTESIAN_POINT('Ctrl Pts',(-19.274277057303,64.0958804445685,36.));
#31641=CARTESIAN_POINT('Ctrl Pts',(-19.3255044901851,64.070090135992,36.));
#31642=CARTESIAN_POINT('Ctrl Pts',(-19.3778411434284,64.0466117153907,36.));
#31643=CARTESIAN_POINT('Ctrl Pts',(-19.4311841342659,64.0255851777059,36.));
#31644=CARTESIAN_POINT('Ctrl Pts',(-19.4436313822641,64.0206787687289,36.));
#31645=CARTESIAN_POINT('Ctrl Pts',(-19.4561334688371,64.0159059301644,36.));
#31646=CARTESIAN_POINT('Ctrl Pts',(-19.4686884555734,64.0112660732732,36.));
#31647=CARTESIAN_POINT('Ctrl Pts',(-21.6673174487995,65.9986976755605,34.8714803633902));
#31648=CARTESIAN_POINT('Ctrl Pts',(-21.6680517344582,65.9132137702119,34.8772098489549));
#31649=CARTESIAN_POINT('Ctrl Pts',(-21.6620451159422,65.8278333924919,34.8829393345197));
#31650=CARTESIAN_POINT('Ctrl Pts',(-21.6489385509365,65.7435572785707,34.8886688200844));
#31651=CARTESIAN_POINT('Ctrl Pts',(-21.5641971770511,65.1986644194321,34.9257131927483));
#31652=CARTESIAN_POINT('Ctrl Pts',(-21.1826527900964,64.6999337142113,34.9627575654121));
#31653=CARTESIAN_POINT('Ctrl Pts',(-20.6789070192068,64.4755856508596,34.999801938076));
#31654=CARTESIAN_POINT('Ctrl Pts',(-20.1751612483172,64.2512375875079,35.0368463107398));
#31655=CARTESIAN_POINT('Ctrl Pts',(-19.5492140934925,64.3012721660255,35.0738906834037));
#31656=CARTESIAN_POINT('Ctrl Pts',(-19.0875124696833,64.6028095203746,35.1109350560675));
#31657=CARTESIAN_POINT('Ctrl Pts',(-18.625810845874,64.9043468747237,35.1479794287314));
#31658=CARTESIAN_POINT('Ctrl Pts',(-18.3283547530802,65.4573870049044,35.1850238013952));
#31659=CARTESIAN_POINT('Ctrl Pts',(-18.331263603936,66.0088140869061,35.2220681740591));
#31660=CARTESIAN_POINT('Ctrl Pts',(-18.3341724547918,66.5602411689079,35.2591125467229));
#31661=CARTESIAN_POINT('Ctrl Pts',(-18.6374462492973,67.1100552027307,35.2961569193868));
#31662=CARTESIAN_POINT('Ctrl Pts',(-19.1023056141942,67.4067178074562,35.3332012920506));
#31663=CARTESIAN_POINT('Ctrl Pts',(-19.567164979091,67.7033804121818,35.3702456647145));
#31664=CARTESIAN_POINT('Ctrl Pts',(-20.1936099143791,67.7468915878102,35.4072900373783));
#31665=CARTESIAN_POINT('Ctrl Pts',(-20.6949575560159,67.5172054957391,35.4443344100422));
#31666=CARTESIAN_POINT('Ctrl Pts',(-21.1963051976527,67.287519403668,35.4813787827061));
#31667=CARTESIAN_POINT('Ctrl Pts',(-21.5725555456381,66.7846360438976,35.5184231553699));
#31668=CARTESIAN_POINT('Ctrl Pts',(-21.6515475919844,66.2389525662666,35.5554675280338));
#31669=CARTESIAN_POINT('Ctrl Pts',(-21.6629293173915,66.1603266819043,35.5608051398192));
#31670=CARTESIAN_POINT('Ctrl Pts',(-21.6681396460096,66.0808122218201,35.5661427516047));
#31671=CARTESIAN_POINT('Ctrl Pts',(-21.6674772588494,66.0012131718681,35.5714803633902));
#31672=CARTESIAN_POINT('Ctrl Pts',(-20.5301702171886,64.0148256743283,36.));
#31673=CARTESIAN_POINT('Ctrl Pts',(-21.1902595624181,64.1911123142463,35.9629556273362));
#31674=CARTESIAN_POINT('Ctrl Pts',(-22.3092728128736,65.2513736304872,35.8888668820085));
#31675=CARTESIAN_POINT('Ctrl Pts',(-21.8813251479519,67.5381211991997,35.7777337640168));
#31676=CARTESIAN_POINT('Ctrl Pts',(-19.7281828950178,68.4128315562992,35.6666006460254));
#31677=CARTESIAN_POINT('Ctrl Pts',(-17.8254683675795,67.0812973613349,35.5554675280337));
#31678=CARTESIAN_POINT('Ctrl Pts',(-17.9121447447308,64.7590835038729,35.4443344100422));
#31679=CARTESIAN_POINT('Ctrl Pts',(-19.9101226209547,63.5731232768953,35.3332012920507));
#31680=CARTESIAN_POINT('Ctrl Pts',(-21.9901520744513,64.6080763665066,35.2220681740591));
#31681=CARTESIAN_POINT('Ctrl Pts',(-22.2488202123297,66.9171030470485,35.1109350560676));
#31682=CARTESIAN_POINT('Ctrl Pts',(-20.4492273182073,68.3866955695652,34.999801938076));
#31683=CARTESIAN_POINT('Ctrl Pts',(-18.2385101136685,67.6719231463612,34.8886688200844));
#31684=CARTESIAN_POINT('Ctrl Pts',(-17.6399646371577,65.4269244123525,34.7775357020929));
#31685=CARTESIAN_POINT('Ctrl Pts',(-19.2014230092252,63.706435258535,34.6664025841013));
#31686=CARTESIAN_POINT('Ctrl Pts',(-21.4937671673603,64.0851026938035,34.5552694661097));
#31687=CARTESIAN_POINT('Ctrl Pts',(-22.4189584788097,66.2163615878931,34.4441363481182));
#31688=CARTESIAN_POINT('Ctrl Pts',(-21.1302229490745,68.1495968002898,34.3330032301266));
#31689=CARTESIAN_POINT('Ctrl Pts',(-18.8070633085623,68.1154369356633,34.2218701121351));
#31690=CARTESIAN_POINT('Ctrl Pts',(-17.5757260722497,66.1451456629571,34.1107369941435));
#31691=CARTESIAN_POINT('Ctrl Pts',(-18.5631798581025,64.0420114979335,33.999603876152));
#31692=CARTESIAN_POINT('Ctrl Pts',(-20.8656679378464,63.730905409822,33.8884707581604));
#31693=CARTESIAN_POINT('Ctrl Pts',(-22.3758626749296,65.4965640343655,33.7773376401688));
#31694=CARTESIAN_POINT('Ctrl Pts',(-21.7115743656249,67.7229870531365,33.6662045221772));
#31695=CARTESIAN_POINT('Ctrl Pts',(-19.4807858366348,68.3724645130774,33.5550714041857));
#31696=CARTESIAN_POINT('Ctrl Pts',(-17.7252025426939,66.8505690671885,33.4439382861941));
#31697=CARTESIAN_POINT('Ctrl Pts',(-18.0516034185067,64.550199335027,33.3328051682026));
#31698=CARTESIAN_POINT('Ctrl Pts',(-20.1612535330058,63.5767442339982,33.221672050211));
#31699=CARTESIAN_POINT('Ctrl Pts',(-22.1233180676414,64.821148188958,33.1105389322195));
#31700=CARTESIAN_POINT('Ctrl Pts',(-22.1420383335758,67.1444837202745,32.9994058142279));
#31701=CARTESIAN_POINT('Ctrl Pts',(-20.2002808069203,68.4203427044879,32.8882726962364));
#31702=CARTESIAN_POINT('Ctrl Pts',(-18.0752184027424,67.4810087817272,32.7771395782448));
#31703=CARTESIAN_POINT('Ctrl Pts',(-17.7117918750668,65.1861973300252,32.6660064602532));
#31704=CARTESIAN_POINT('Ctrl Pts',(-19.4426234863108,63.6362101128286,32.5548733422617));
#31705=CARTESIAN_POINT('Ctrl Pts',(-21.6835880210157,64.2496564382428,32.4437402242701));
#31706=CARTESIAN_POINT('Ctrl Pts',(-22.3836665335049,66.4650860842244,32.3326071062786));
#31707=CARTESIAN_POINT('Ctrl Pts',(-20.9021196143316,68.2548506403159,32.221473988287));
#31708=CARTESIAN_POINT('Ctrl Pts',(-18.5949173170392,67.9808871403329,32.1103408702954));
#31709=CARTESIAN_POINT('Ctrl Pts',(-17.5737019947084,65.8939377625597,31.9992077523039));
#31710=CARTESIAN_POINT('Ctrl Pts',(-18.7731301049792,63.9040607190605,31.8880746343123));
#31711=CARTESIAN_POINT('Ctrl Pts',(-21.0954378323017,63.8324698008436,31.7769415163208));
#31712=CARTESIAN_POINT('Ctrl Pts',(-22.4151577394886,65.7446878340517,31.6658083983292));
#31713=CARTESIAN_POINT('Ctrl Pts',(-21.5244302238133,67.8905776105247,31.5546752803377));
#31714=CARTESIAN_POINT('Ctrl Pts',(-19.2384841663151,68.3061363454358,31.4435421623461));
#31715=CARTESIAN_POINT('Ctrl Pts',(-17.6495073727765,66.611028328362,31.3324090443545));
#31716=CARTESIAN_POINT('Ctrl Pts',(-18.2117939461611,64.3566831353306,31.221275926363));
#31717=CARTESIAN_POINT('Ctrl Pts',(-20.4107170831235,63.6063662171661,31.1101428083713));
#31718=CARTESIAN_POINT('Ctrl Pts',(-22.2337357799444,65.0467971495588,30.9990096903799));
#31719=CARTESIAN_POINT('Ctrl Pts',(-22.0123515719766,67.3596368483739,30.8878765723882));
#31720=CARTESIAN_POINT('Ctrl Pts',(-19.9491839999498,68.4280833887723,30.7767434543968));
#31721=CARTESIAN_POINT('Ctrl Pts',(-17.9325252312672,67.2742524433354,30.6656103364051));
#31722=CARTESIAN_POINT('Ctrl Pts',(-17.8081007459427,64.9541755076705,30.5544772184136));
#31723=CARTESIAN_POINT('Ctrl Pts',(-19.6897887302455,63.5912783106364,30.4433441004221));
#31724=CARTESIAN_POINT('Ctrl Pts',(-21.8553942784241,64.4329380100698,30.3322109824304));
#31725=CARTESIAN_POINT('Ctrl Pts',(-22.3228699553819,66.7088345216461,30.221077864439));
#31726=CARTESIAN_POINT('Ctrl Pts',(-20.6643636219036,68.335977779557,30.1099447464473));
#31727=CARTESIAN_POINT('Ctrl Pts',(-18.3978055525618,67.8251422304279,29.9988116284558));
#31728=CARTESIAN_POINT('Ctrl Pts',(-17.5976389032744,65.643864675113,29.8876785104642));
#31729=CARTESIAN_POINT('Ctrl Pts',(-18.9962076857216,63.7885361864844,29.7765453924727));
#31730=CARTESIAN_POINT('Ctrl Pts',(-21.3134867030769,63.9572264223528,29.6654122744811));
#31731=CARTESIAN_POINT('Ctrl Pts',(-22.4286109914434,65.9955434392686,29.5542791564896));
#31732=CARTESIAN_POINT('Ctrl Pts',(-21.3209749112437,68.037939275974,29.4431460384979));
#31733=CARTESIAN_POINT('Ctrl Pts',(-19.0043305992079,68.2151328748,29.3320129205065));
#31734=CARTESIAN_POINT('Ctrl Pts',(-17.5989621119428,66.3649496798285,29.2208798025149));
#31735=CARTESIAN_POINT('Ctrl Pts',(-18.391118003758,64.1807501735986,29.1097466845233));
#31736=CARTESIAN_POINT('Ctrl Pts',(-20.6557860235121,63.6615997134667,28.9986135665318));
#31737=CARTESIAN_POINT('Ctrl Pts',(-22.3202528630616,65.2826452341084,28.8874804485401));
#31738=CARTESIAN_POINT('Ctrl Pts',(-21.8611329580743,67.5602420713026,28.7763473305487));
#31739=CARTESIAN_POINT('Ctrl Pts',(-19.6986309163782,68.4098439543111,28.665214212557));
#31740=CARTESIAN_POINT('Ctrl Pts',(-17.8119537217837,67.0538617998004,28.5540810945656));
#31741=CARTESIAN_POINT('Ctrl Pts',(-17.9278626016764,64.733343846516,28.442947976574));
#31742=CARTESIAN_POINT('Ctrl Pts',(-19.9402731870454,63.5721194600009,28.3318148585824));
#31743=CARTESIAN_POINT('Ctrl Pts',(-22.0073481024602,64.6329869041389,28.2206817405909));
#31744=CARTESIAN_POINT('Ctrl Pts',(-22.2372190260415,66.944998538722,28.1095486225993));
#31745=CARTESIAN_POINT('Ctrl Pts',(-20.4194990409278,68.3921103158831,27.9984155046077));
#31746=CARTESIAN_POINT('Ctrl Pts',(-18.2178370221936,67.6498685794103,27.8872823866162));
#31747=CARTESIAN_POINT('Ctrl Pts',(-17.647280706083,65.3976021808533,27.7761492686246));
#31748=CARTESIAN_POINT('Ctrl Pts',(-19.2300256897269,63.6966739765529,27.6650161506331));
#31749=CARTESIAN_POINT('Ctrl Pts',(-21.51748146836,64.1038404068878,27.5538830326415));
#31750=CARTESIAN_POINT('Ctrl Pts',(-22.4160784789961,66.2464467290574,27.44274991465));
#31751=CARTESIAN_POINT('Ctrl Pts',(-21.1033853710592,68.1634953045376,27.3316167966584));
#31752=CARTESIAN_POINT('Ctrl Pts',(-18.7808305400592,68.1004278233727,27.2204836786668));
#31753=CARTESIAN_POINT('Ctrl Pts',(-17.5741075901122,66.1149661254002,27.1093505606753));
#31754=CARTESIAN_POINT('Ctrl Pts',(-18.5876568453766,64.0242829060802,26.9982174426837));
#31755=CARTESIAN_POINT('Ctrl Pts',(-20.8938381659967,63.7418537313102,26.8870843246922));
#31756=CARTESIAN_POINT('Ctrl Pts',(-22.3819435741815,65.5261689079406,26.7759512067006));
#31757=CARTESIAN_POINT('Ctrl Pts',(-21.6900005542035,67.7441529368256,26.664818088709));
#31758=CARTESIAN_POINT('Ctrl Pts',(-19.4513023431397,68.3658195746722,26.5536849707175));
#31759=CARTESIAN_POINT('Ctrl Pts',(-17.714794155333,66.8221949683201,26.4425518527259));
#31760=CARTESIAN_POINT('Ctrl Pts',(-18.0697956411282,64.5260652687741,26.3314187347344));
#31761=CARTESIAN_POINT('Ctrl Pts',(-20.1913974446539,63.5789384432151,26.2202856167427));
#31762=CARTESIAN_POINT('Ctrl Pts',(-22.1378221489769,64.8476628562653,26.1091524987513));
#31763=CARTESIAN_POINT('Ctrl Pts',(-22.127633111299,67.1710507618066,25.9980193807596));
#31764=CARTESIAN_POINT('Ctrl Pts',(-20.1701400749251,68.4226485469194,25.8868862627681));
#31765=CARTESIAN_POINT('Ctrl Pts',(-18.0569489447748,67.4569397798106,25.7757531447766));
#31766=CARTESIAN_POINT('Ctrl Pts',(-17.7220731495743,65.1577888564038,25.664620026785));
#31767=CARTESIAN_POINT('Ctrl Pts',(-19.4721283434274,63.6294498117299,25.5534869087935));
#31768=CARTESIAN_POINT('Ctrl Pts',(-21.7051476175159,64.2707573406571,25.4423537908019));
#31769=CARTESIAN_POINT('Ctrl Pts',(-22.3778773235377,66.4946844969483,25.3312206728103));
#31770=CARTESIAN_POINT('Ctrl Pts',(-20.8736248136923,68.2659592866881,25.2200875548188));
#31771=CARTESIAN_POINT('Ctrl Pts',(-18.5711038201239,67.9631343216322,25.1089544368272));
#31772=CARTESIAN_POINT('Ctrl Pts',(-17.5737474231758,65.8639868785843,24.9978213188357));
#31773=CARTESIAN_POINT('Ctrl Pts',(-18.8023459831469,63.888411209226,24.8866882008441));
#31774=CARTESIAN_POINT('Ctrl Pts',(-20.343660854084,63.8620828587222,24.8125994555164));
#31775=CARTESIAN_POINT('Ctrl Pts',(-20.9495535522615,64.1778184465077,24.7755550828525));
#31776=CARTESIAN_POINT('Ctrl Pts',(-20.4967348970876,64.1400211999972,36.0748149723825));
#31777=CARTESIAN_POINT('Ctrl Pts',(-21.1151955392376,64.3051902779623,36.0377705997186));
#31778=CARTESIAN_POINT('Ctrl Pts',(-22.163637933366,65.2985859436069,35.9636818543909));
#31779=CARTESIAN_POINT('Ctrl Pts',(-21.7626788971888,67.4411191930855,35.8525487363994));
#31780=CARTESIAN_POINT('Ctrl Pts',(-19.7453251101392,68.2606657181987,35.7414156184078));
#31781=CARTESIAN_POINT('Ctrl Pts',(-17.962605760142,67.0131050671841,35.6302825004162));
#31782=CARTESIAN_POINT('Ctrl Pts',(-18.0438158694395,64.8373422195106,35.5191493824247));
#31783=CARTESIAN_POINT('Ctrl Pts',(-19.9157907608102,63.7261748770262,35.4080162644331));
#31784=CARTESIAN_POINT('Ctrl Pts',(-21.8646426257847,64.6958583858148,35.2968831464416));
#31785=CARTESIAN_POINT('Ctrl Pts',(-22.1069977915091,66.8592657092475,35.18575002845));
#31786=CARTESIAN_POINT('Ctrl Pts',(-20.4208966826956,68.2361780041406,35.0746169104584));
#31787=CARTESIAN_POINT('Ctrl Pts',(-18.3495989230632,67.5664828862893,34.9634837924669));
#31788=CARTESIAN_POINT('Ctrl Pts',(-17.7888008698389,65.4630655705954,34.8523506744753));
#31789=CARTESIAN_POINT('Ctrl Pts',(-19.2517854710274,63.8510795045088,34.7412175564838));
#31790=CARTESIAN_POINT('Ctrl Pts',(-21.3995623595878,64.2058661812974,34.6300844384922));
#31791=CARTESIAN_POINT('Ctrl Pts',(-22.2664062447768,66.2027166891148,34.5189513205007));
#31792=CARTESIAN_POINT('Ctrl Pts',(-21.0589451502421,68.0140319292816,34.4078182025091));
#31793=CARTESIAN_POINT('Ctrl Pts',(-18.8822961655679,67.9820263652388,34.2966850845176));
#31794=CARTESIAN_POINT('Ctrl Pts',(-17.7286135264271,66.1359920146667,34.185551966526));
#31795=CARTESIAN_POINT('Ctrl Pts',(-18.6537932871754,64.1654925426962,34.0744188485344));
#31796=CARTESIAN_POINT('Ctrl Pts',(-20.8110743683388,63.8740064394576,33.9632857305429));
#31797=CARTESIAN_POINT('Ctrl Pts',(-22.2260282887709,65.5283133520668,33.8521526125513));
#31798=CARTESIAN_POINT('Ctrl Pts',(-21.6036334912871,67.6143264347472,33.7410194945597));
#31799=CARTESIAN_POINT('Ctrl Pts',(-19.5135302104043,68.2228444328634,33.6298863765682));
#31800=CARTESIAN_POINT('Ctrl Pts',(-17.868663225101,66.7969277118137,33.5187532585766));
#31801=CARTESIAN_POINT('Ctrl Pts',(-18.1744795463496,64.6416313841015,33.4076201405851));
#31802=CARTESIAN_POINT('Ctrl Pts',(-20.1510840377783,63.7295674775451,33.2964870225935));
#31803=CARTESIAN_POINT('Ctrl Pts',(-21.9894104716166,64.8954927793853,33.1853539046019));
#31804=CARTESIAN_POINT('Ctrl Pts',(-22.0069501392006,67.0723065622656,33.0742207866104));
#31805=CARTESIAN_POINT('Ctrl Pts',(-20.1876500466996,68.2677031739092,32.9630876686188));
#31806=CARTESIAN_POINT('Ctrl Pts',(-18.1966052455756,67.387608584802,32.8519545506273));
#31807=CARTESIAN_POINT('Ctrl Pts',(-17.8560983046515,65.2375200031732,32.7408214326357));
#31808=CARTESIAN_POINT('Ctrl Pts',(-19.4777745784464,63.7852831255451,32.6296883146441));
#31809=CARTESIAN_POINT('Ctrl Pts',(-21.5774121126457,64.3600423018326,32.5185551966526));
#31810=CARTESIAN_POINT('Ctrl Pts',(-22.2333399950128,66.435755311585,32.407422078661));
#31811=CARTESIAN_POINT('Ctrl Pts',(-20.8452272105401,68.1126479090148,32.2962889606695));
#31812=CARTESIAN_POINT('Ctrl Pts',(-18.6835292151616,67.8559619871019,32.1851558426779));
#31813=CARTESIAN_POINT('Ctrl Pts',(-17.7267170978527,65.9006266046419,32.0740227246864));
#31814=CARTESIAN_POINT('Ctrl Pts',(-18.850502968132,64.036241664912,31.9628896066948));
#31815=CARTESIAN_POINT('Ctrl Pts',(-21.0263537657393,63.9691656462299,31.8517564887033));
#31816=CARTESIAN_POINT('Ctrl Pts',(-22.2628452000513,65.7607891609791,31.7406233707116));
#31817=CARTESIAN_POINT('Ctrl Pts',(-21.4282916425573,67.7713478508474,31.6294902527201));
#31818=CARTESIAN_POINT('Ctrl Pts',(-19.2865093567836,68.1606992680479,31.5183571347286));
#31819=CARTESIAN_POINT('Ctrl Pts',(-17.7977417903996,66.5724936708367,31.407224016737));
#31820=CARTESIAN_POINT('Ctrl Pts',(-18.3245676174803,64.4603193329442,31.2960908987455));
#31821=CARTESIAN_POINT('Ctrl Pts',(-20.3848151054191,63.7573213427819,31.1849577807539));
#31822=CARTESIAN_POINT('Ctrl Pts',(-22.0928646627033,65.1069111306771,31.0738246627624));
#31823=CARTESIAN_POINT('Ctrl Pts',(-21.885442106331,67.2738910034122,30.9626915447707));
#31824=CARTESIAN_POINT('Ctrl Pts',(-19.9523887239665,68.274955689963,30.8515584267792));
#31825=CARTESIAN_POINT('Ctrl Pts',(-18.0629110553893,67.1938913876763,30.7404253087876));
#31826=CARTESIAN_POINT('Ctrl Pts',(-17.9463334319978,65.0201306962811,30.6292921907961));
#31827=CARTESIAN_POINT('Ctrl Pts',(-19.7093522831703,63.7431849589295,30.5181590728045));
#31828=CARTESIAN_POINT('Ctrl Pts',(-21.738383364568,64.53176517454,30.407025954813));
#31829=CARTESIAN_POINT('Ctrl Pts',(-22.1763775686106,66.6641316915711,30.2958928368214));
#31830=CARTESIAN_POINT('Ctrl Pts',(-20.6224653604744,68.1886587445077,30.1847597188299));
#31831=CARTESIAN_POINT('Ctrl Pts',(-18.4988483544341,67.7100391697021,30.0736266008383));
#31832=CARTESIAN_POINT('Ctrl Pts',(-17.7491444191688,65.6663244402993,29.9624934828468));
#31833=CARTESIAN_POINT('Ctrl Pts',(-19.0595121042925,63.9280027164766,29.8513603648552));
#31834=CARTESIAN_POINT('Ctrl Pts',(-21.2306513288106,64.0860544595529,29.7402272468636));
#31835=CARTESIAN_POINT('Ctrl Pts',(-22.2754500192369,65.9958244934088,29.6290941288721));
#31836=CARTESIAN_POINT('Ctrl Pts',(-21.2376672912176,67.9094161152432,29.5179610108805));
#31837=CARTESIAN_POINT('Ctrl Pts',(-19.067122744166,68.0754349545212,29.406827892889));
#31838=CARTESIAN_POINT('Ctrl Pts',(-17.7503841793447,66.3419340350975,29.2956947748974));
#31839=CARTESIAN_POINT('Ctrl Pts',(-18.492582557603,64.2954816283601,29.1845616569058));
#31840=CARTESIAN_POINT('Ctrl Pts',(-20.6144287105154,63.8090715245369,29.0734285389143));
#31841=CARTESIAN_POINT('Ctrl Pts',(-22.1739255238857,65.3278853955619,28.9622954209227));
#31842=CARTESIAN_POINT('Ctrl Pts',(-21.7437601329209,67.4618450067418,28.8511623029312));
#31843=CARTESIAN_POINT('Ctrl Pts',(-19.7176368345772,68.2578665300926,28.7400291849396));
#31844=CARTESIAN_POINT('Ctrl Pts',(-17.9499434189336,66.9873997363422,28.628896066948));
#31845=CARTESIAN_POINT('Ctrl Pts',(-18.0585424757241,64.8132258402162,28.5177629489565));
#31846=CARTESIAN_POINT('Ctrl Pts',(-19.9440398737528,63.7252343661005,28.4066298309649));
#31847=CARTESIAN_POINT('Ctrl Pts',(-21.8807541818971,64.7191979340316,28.2954967129734));
#31848=CARTESIAN_POINT('Ctrl Pts',(-22.096128236996,66.8854019646168,28.1843635949818));
#31849=CARTESIAN_POINT('Ctrl Pts',(-20.3930432268125,68.2412512680995,28.0732304769902));
#31850=CARTESIAN_POINT('Ctrl Pts',(-18.3302295853801,67.5458191962338,27.9620973589987));
#31851=CARTESIAN_POINT('Ctrl Pts',(-17.7956555490096,65.4355925531116,27.8509642410071));
#31852=CARTESIAN_POINT('Ctrl Pts',(-19.2785843161808,63.841933820267,27.7398311230155));
#31853=CARTESIAN_POINT('Ctrl Pts',(-21.4217811121406,64.2234221957222,27.628698005024));
#31854=CARTESIAN_POINT('Ctrl Pts',(-22.2637078728867,66.2309045031708,27.5175648870325));
#31855=CARTESIAN_POINT('Ctrl Pts',(-21.0338000909361,68.0270539208107,27.4064317690409));
#31856=CARTESIAN_POINT('Ctrl Pts',(-18.8577177733077,67.9679638064466,27.2952986510493));
#31857=CARTESIAN_POINT('Ctrl Pts',(-17.7270971142788,66.1077157573507,27.1841655330578));
#31858=CARTESIAN_POINT('Ctrl Pts',(-18.6767266269981,64.1488820090142,27.0730324150662));
#31859=CARTESIAN_POINT('Ctrl Pts',(-20.8374680338588,63.8842643022561,26.9618992970747));
#31860=CARTESIAN_POINT('Ctrl Pts',(-22.231725694559,65.5560511867317,26.8507661790831));
#31861=CARTESIAN_POINT('Ctrl Pts',(-21.5834202377908,67.6341574865776,26.7396330610915));
#31862=CARTESIAN_POINT('Ctrl Pts',(-19.4859061009536,68.2166185591953,26.6284999430999));
#31863=CARTESIAN_POINT('Ctrl Pts',(-17.8589112453462,66.7703430327343,26.5173668251085));
#31864=CARTESIAN_POINT('Ctrl Pts',(-18.191524471807,64.6190193388985,26.4062337071168));
#31865=CARTESIAN_POINT('Ctrl Pts',(-20.1793269159424,63.7316233083974,26.2951005891253));
#31866=CARTESIAN_POINT('Ctrl Pts',(-22.0029998493598,64.9203352924298,26.1839674711337));
#31867=CARTESIAN_POINT('Ctrl Pts',(-21.9934533859443,67.0971981465407,26.0728343531422));
#31868=CARTESIAN_POINT('Ctrl Pts',(-20.1594101476628,68.2698635977991,25.9617012351506));
#31869=CARTESIAN_POINT('Ctrl Pts',(-18.1794879556388,67.3650575006361,25.8505681171591));
#31870=CARTESIAN_POINT('Ctrl Pts',(-17.8657311879574,65.2109031171935,25.7394349991675));
#31871=CARTESIAN_POINT('Ctrl Pts',(-19.5054187042162,63.7789491645613,25.6283018811759));
#31872=CARTESIAN_POINT('Ctrl Pts',(-21.5976120476884,64.3798124704489,25.5171687631844));
#31873=CARTESIAN_POINT('Ctrl Pts',(-22.2279158830502,66.4634870928539,25.4060356451928));
#31874=CARTESIAN_POINT('Ctrl Pts',(-20.818529441778,68.1230559857674,25.2949025272013));
#31875=CARTESIAN_POINT('Ctrl Pts',(-18.6612175225089,67.8393287544449,25.1837694092097));
#31876=CARTESIAN_POINT('Ctrl Pts',(-17.7267596613622,65.8725645808109,25.0726362912181));
#31877=CARTESIAN_POINT('Ctrl Pts',(-18.8778763394841,64.0215790954106,24.9615031732266));
#31878=CARTESIAN_POINT('Ctrl Pts',(-20.3219877945836,63.996911149053,24.8874144278989));
#31879=CARTESIAN_POINT('Ctrl Pts',(-20.8896697150645,64.2927347913867,24.850370055235));
#31880=CARTESIAN_POINT('Ctrl Pts',(-20.4632995769867,64.2652167256662,36.149629944765));
#31881=CARTESIAN_POINT('Ctrl Pts',(-21.0401315160572,64.4192682416784,36.1125855721011));
#31882=CARTESIAN_POINT('Ctrl Pts',(-22.0180030538584,65.3457982567266,36.0384968267734));
#31883=CARTESIAN_POINT('Ctrl Pts',(-21.6440326464257,67.3441171869714,35.9273637087819));
#31884=CARTESIAN_POINT('Ctrl Pts',(-19.7624673252605,68.1084998800982,35.8162305907903));
#31885=CARTESIAN_POINT('Ctrl Pts',(-18.0997431527045,66.9449127730333,35.7050974727987));
#31886=CARTESIAN_POINT('Ctrl Pts',(-18.1754869941483,64.9156009351482,35.5939643548072));
#31887=CARTESIAN_POINT('Ctrl Pts',(-19.9214589006656,63.8792264771571,35.4828312368156));
#31888=CARTESIAN_POINT('Ctrl Pts',(-21.7391331771181,64.7836404051231,35.371698118824));
#31889=CARTESIAN_POINT('Ctrl Pts',(-21.9651753706885,66.8014283714463,35.2605650008325));
#31890=CARTESIAN_POINT('Ctrl Pts',(-20.3925660471839,68.0856604387161,35.1494318828409));
#31891=CARTESIAN_POINT('Ctrl Pts',(-18.4606877324579,67.4610426262175,35.0382987648494));
#31892=CARTESIAN_POINT('Ctrl Pts',(-17.93763710252,65.4992067288381,34.9271656468578));
#31893=CARTESIAN_POINT('Ctrl Pts',(-19.3021479328295,63.9957237504828,34.8160325288663));
#31894=CARTESIAN_POINT('Ctrl Pts',(-21.3053575518154,64.3266296687912,34.7048994108747));
#31895=CARTESIAN_POINT('Ctrl Pts',(-22.113854010744,66.1890717903366,34.5937662928832));
#31896=CARTESIAN_POINT('Ctrl Pts',(-20.9876673514096,67.8784670582733,34.4826331748916));
#31897=CARTESIAN_POINT('Ctrl Pts',(-18.9575290225734,67.8486157948143,34.3715000569));
#31898=CARTESIAN_POINT('Ctrl Pts',(-17.8815009806044,66.1268383663763,34.2603669389085));
#31899=CARTESIAN_POINT('Ctrl Pts',(-18.7444067162484,64.2889735874589,34.1492338209169));
#31900=CARTESIAN_POINT('Ctrl Pts',(-20.756480798831,64.0171074690934,34.0381007029254));
#31901=CARTESIAN_POINT('Ctrl Pts',(-22.0761939026122,65.5600626697681,33.9269675849338));
#31902=CARTESIAN_POINT('Ctrl Pts',(-21.4956926169493,67.5056658163578,33.8158344669422));
#31903=CARTESIAN_POINT('Ctrl Pts',(-19.5462745841737,68.0732243526495,33.7047013489507));
#31904=CARTESIAN_POINT('Ctrl Pts',(-18.012123907508,66.7432863564387,33.5935682309591));
#31905=CARTESIAN_POINT('Ctrl Pts',(-18.2973556741925,64.7330634331763,33.4824351129676));
#31906=CARTESIAN_POINT('Ctrl Pts',(-20.1409145425508,63.8823907210918,33.371301994976));
#31907=CARTESIAN_POINT('Ctrl Pts',(-21.8555028755919,64.9698373698129,33.2601688769845));
#31908=CARTESIAN_POINT('Ctrl Pts',(-21.8718619448253,67.0001294042565,33.1490357589929));
#31909=CARTESIAN_POINT('Ctrl Pts',(-20.175019286479,68.1150636433306,33.0379026410013));
#31910=CARTESIAN_POINT('Ctrl Pts',(-18.3179920884086,67.2942083878766,32.9267695230098));
#31911=CARTESIAN_POINT('Ctrl Pts',(-18.0004047342363,65.2888426763213,32.8156364050182));
#31912=CARTESIAN_POINT('Ctrl Pts',(-19.5129256705819,63.9343561382617,32.7045032870267));
#31913=CARTESIAN_POINT('Ctrl Pts',(-21.4712362042757,64.4704281654224,32.5933701690351));
#31914=CARTESIAN_POINT('Ctrl Pts',(-22.0830134565206,66.4064245389456,32.4822370510435));
#31915=CARTESIAN_POINT('Ctrl Pts',(-20.7883348067487,67.9704451777137,32.371103933052));
#31916=CARTESIAN_POINT('Ctrl Pts',(-18.772141113284,67.7310368338708,32.2599708150604));
#31917=CARTESIAN_POINT('Ctrl Pts',(-17.879732200997,65.907315446724,32.1488376970689));
#31918=CARTESIAN_POINT('Ctrl Pts',(-18.9278758312847,64.1684226107636,32.0377045790773));
#31919=CARTESIAN_POINT('Ctrl Pts',(-20.9572696991769,64.105861491616,31.9265714610858));
#31920=CARTESIAN_POINT('Ctrl Pts',(-22.1105326606141,65.7768904879066,31.8154383430941));
#31921=CARTESIAN_POINT('Ctrl Pts',(-21.3321530613013,67.6521180911699,31.7043052251027));
#31922=CARTESIAN_POINT('Ctrl Pts',(-19.334534547252,68.0152621906601,31.593172107111));
#31923=CARTESIAN_POINT('Ctrl Pts',(-17.9459762080226,66.5339590133113,31.4820389891195));
#31924=CARTESIAN_POINT('Ctrl Pts',(-18.4373412887996,64.5639555305579,31.3709058711279));
#31925=CARTESIAN_POINT('Ctrl Pts',(-20.3589131277147,63.9082764683976,31.2597727531364));
#31926=CARTESIAN_POINT('Ctrl Pts',(-21.9519935454622,65.1670251117956,31.1486396351448));
#31927=CARTESIAN_POINT('Ctrl Pts',(-21.7585326406854,67.1881451584504,31.0375065171532));
#31928=CARTESIAN_POINT('Ctrl Pts',(-19.9555934479831,68.1218279911537,30.9263733991617));
#31929=CARTESIAN_POINT('Ctrl Pts',(-18.1932968795114,67.1135303320171,30.8152402811701));
#31930=CARTESIAN_POINT('Ctrl Pts',(-18.0845661180528,65.0860858848918,30.7041071631786));
#31931=CARTESIAN_POINT('Ctrl Pts',(-19.7289158360952,63.8950916072225,30.592974045187));
#31932=CARTESIAN_POINT('Ctrl Pts',(-21.621372450712,64.6305923390101,30.4818409271955));
#31933=CARTESIAN_POINT('Ctrl Pts',(-22.0298851818394,66.6194288614961,30.3707078092039));
#31934=CARTESIAN_POINT('Ctrl Pts',(-20.5805670990452,68.0413397094584,30.2595746912124));
#31935=CARTESIAN_POINT('Ctrl Pts',(-18.5998911563065,67.5949361089764,30.1484415732208));
#31936=CARTESIAN_POINT('Ctrl Pts',(-17.9006499350632,65.6887842054856,30.0373084552293));
#31937=CARTESIAN_POINT('Ctrl Pts',(-19.1228165228634,64.0674692464688,29.9261753372376));
#31938=CARTESIAN_POINT('Ctrl Pts',(-21.1478159545443,64.2148824967529,29.8150422192461));
#31939=CARTESIAN_POINT('Ctrl Pts',(-22.1222890470305,65.996105547549,29.7039091012546));
#31940=CARTESIAN_POINT('Ctrl Pts',(-21.1543596711915,67.7808929545126,29.592775983263));
#31941=CARTESIAN_POINT('Ctrl Pts',(-19.1299148891241,67.9357370342423,29.4816428652714));
#31942=CARTESIAN_POINT('Ctrl Pts',(-17.9018062467466,66.3189183903665,29.3705097472799));
#31943=CARTESIAN_POINT('Ctrl Pts',(-18.594047111448,64.4102130831215,29.2593766292883));
#31944=CARTESIAN_POINT('Ctrl Pts',(-20.5730713975186,63.9565433356072,29.1482435112968));
#31945=CARTESIAN_POINT('Ctrl Pts',(-22.0275981847098,65.3731255570155,29.0371103933052));
#31946=CARTESIAN_POINT('Ctrl Pts',(-21.6263873077676,67.363447942181,28.9259772753137));
#31947=CARTESIAN_POINT('Ctrl Pts',(-19.7366427527761,68.1058891058742,28.8148441573221));
#31948=CARTESIAN_POINT('Ctrl Pts',(-18.0879331160836,66.920937672884,28.7037110393305));
#31949=CARTESIAN_POINT('Ctrl Pts',(-18.1892223497717,64.8931078339165,28.592577921339));
#31950=CARTESIAN_POINT('Ctrl Pts',(-19.9478065604602,63.8783492722001,28.4814448033474));
#31951=CARTESIAN_POINT('Ctrl Pts',(-21.754160261334,64.8054089639244,28.3703116853558));
#31952=CARTESIAN_POINT('Ctrl Pts',(-21.9550374479505,66.8258053905114,28.2591785673643));
#31953=CARTESIAN_POINT('Ctrl Pts',(-20.3665874126971,68.0903922203161,28.1480454493727));
#31954=CARTESIAN_POINT('Ctrl Pts',(-18.4426221485666,67.4417698130572,28.0369123313812));
#31955=CARTESIAN_POINT('Ctrl Pts',(-17.9440303919362,65.47358292537,27.9257792133896));
#31956=CARTESIAN_POINT('Ctrl Pts',(-19.3271429426348,63.9871936639811,27.8146460953981));
#31957=CARTESIAN_POINT('Ctrl Pts',(-21.3260807559213,64.3430039845566,27.7035129774064));
#31958=CARTESIAN_POINT('Ctrl Pts',(-22.1113372667774,66.2153622772843,27.592379859415));
#31959=CARTESIAN_POINT('Ctrl Pts',(-20.9642148108129,67.8906125370837,27.4812467414234));
#31960=CARTESIAN_POINT('Ctrl Pts',(-18.9346050065562,67.8354997895207,27.3701136234318));
#31961=CARTESIAN_POINT('Ctrl Pts',(-17.8800866384454,66.1004653893011,27.2589805054403));
#31962=CARTESIAN_POINT('Ctrl Pts',(-18.7657964086194,64.2734811119483,27.1478473874487));
#31963=CARTESIAN_POINT('Ctrl Pts',(-20.7810979017209,64.0266748732019,27.0367142694572));
#31964=CARTESIAN_POINT('Ctrl Pts',(-22.0815078149365,65.5859334655229,26.9255811514656));
#31965=CARTESIAN_POINT('Ctrl Pts',(-21.4768399213782,67.5241620363296,26.814448033474));
#31966=CARTESIAN_POINT('Ctrl Pts',(-19.5205098587676,68.0674175437184,26.7033149154824));
#31967=CARTESIAN_POINT('Ctrl Pts',(-18.0030283353595,66.7184910971486,26.5921817974909));
#31968=CARTESIAN_POINT('Ctrl Pts',(-18.3132533024857,64.7119734090229,26.4810486794993));
#31969=CARTESIAN_POINT('Ctrl Pts',(-20.1672563872311,63.8843081735796,26.3699155615078));
#31970=CARTESIAN_POINT('Ctrl Pts',(-21.8681775497427,64.9930077285944,26.2587824435162));
#31971=CARTESIAN_POINT('Ctrl Pts',(-21.8592736605897,67.0233455312749,26.1476493255247));
#31972=CARTESIAN_POINT('Ctrl Pts',(-20.1486802204003,68.1170786486788,26.0365162075331));
#31973=CARTESIAN_POINT('Ctrl Pts',(-18.3020269665029,67.2731752214615,25.9253830895416));
#31974=CARTESIAN_POINT('Ctrl Pts',(-18.0093892263405,65.2640173779833,25.8142499715499));
#31975=CARTESIAN_POINT('Ctrl Pts',(-19.5387090650051,63.9284485173924,25.7031168535584));
#31976=CARTESIAN_POINT('Ctrl Pts',(-21.4900764778608,64.4888676002409,25.5919837355669));
#31977=CARTESIAN_POINT('Ctrl Pts',(-22.0779544425627,66.4322896887595,25.4808506175753));
#31978=CARTESIAN_POINT('Ctrl Pts',(-20.7634340698636,67.9801526848469,25.3697174995838));
#31979=CARTESIAN_POINT('Ctrl Pts',(-18.7513312248939,67.7155231872575,25.2585843815922));
#31980=CARTESIAN_POINT('Ctrl Pts',(-17.8797718995485,65.8811422830375,25.1474512636006));
#31981=CARTESIAN_POINT('Ctrl Pts',(-18.9534066958213,64.1547469815952,25.0363181456091));
#31982=CARTESIAN_POINT('Ctrl Pts',(-20.3003147350832,64.1317394393838,24.9622294002814));
#31983=CARTESIAN_POINT('Ctrl Pts',(-20.8297858778675,64.4076511362656,24.9251850276175));
#31984=CARTESIAN_POINT('Ctrl Pts',(-20.4298642568858,64.3904122513351,36.2244449171475));
#31985=CARTESIAN_POINT('Ctrl Pts',(-20.9650674928767,64.5333462053945,36.1874005444836));
#31986=CARTESIAN_POINT('Ctrl Pts',(-21.8723681743508,65.3930105698463,36.1133117991559));
#31987=CARTESIAN_POINT('Ctrl Pts',(-21.5253863956627,67.2471151808573,36.0021786811643));
#31988=CARTESIAN_POINT('Ctrl Pts',(-19.7796095403819,67.9563340419976,35.8910455631728));
#31989=CARTESIAN_POINT('Ctrl Pts',(-18.236880545267,66.8767204788825,35.7799124451813));
#31990=CARTESIAN_POINT('Ctrl Pts',(-18.307158118857,64.9938596507859,35.6687793271897));
#31991=CARTESIAN_POINT('Ctrl Pts',(-19.927127040521,64.032278077288,35.5576462091981));
#31992=CARTESIAN_POINT('Ctrl Pts',(-21.6136237284516,64.8714224244312,35.4465130912065));
#31993=CARTESIAN_POINT('Ctrl Pts',(-21.8233529498679,66.7435910336453,35.3353799732151));
#31994=CARTESIAN_POINT('Ctrl Pts',(-20.3642354116722,67.9351428732915,35.2242468552234));
#31995=CARTESIAN_POINT('Ctrl Pts',(-18.5717765418526,67.3556023661456,35.1131137372319));
#31996=CARTESIAN_POINT('Ctrl Pts',(-18.0864733352012,65.5353478870809,35.0019806192403));
#31997=CARTESIAN_POINT('Ctrl Pts',(-19.3525103946316,64.1403679964566,34.8908475012488));
#31998=CARTESIAN_POINT('Ctrl Pts',(-21.2111527440429,64.447393156285,34.7797143832572));
#31999=CARTESIAN_POINT('Ctrl Pts',(-21.9613017767111,66.1754268915585,34.6685812652656));
#32000=CARTESIAN_POINT('Ctrl Pts',(-20.9163895525773,67.742902187265,34.5574481472741));
#32001=CARTESIAN_POINT('Ctrl Pts',(-19.0327618795789,67.7152052243898,34.4463150292825));
#32002=CARTESIAN_POINT('Ctrl Pts',(-18.0343884347818,66.1176847180857,34.3351819112909));
#32003=CARTESIAN_POINT('Ctrl Pts',(-18.8350201453212,64.4124546322215,34.2240487932994));
#32004=CARTESIAN_POINT('Ctrl Pts',(-20.7018872293234,64.1602084987291,34.1129156753078));
#32005=CARTESIAN_POINT('Ctrl Pts',(-21.9263595164535,65.5918119874694,34.0017825573163));
#32006=CARTESIAN_POINT('Ctrl Pts',(-21.3877517426115,67.3970051979684,33.8906494393247));
#32007=CARTESIAN_POINT('Ctrl Pts',(-19.5790189579431,67.9236042724355,33.7795163213332));
#32008=CARTESIAN_POINT('Ctrl Pts',(-18.1555845899151,66.6896450010639,33.6683832033416));
#32009=CARTESIAN_POINT('Ctrl Pts',(-18.4202318020353,64.8244954822508,33.5572500853501));
#32010=CARTESIAN_POINT('Ctrl Pts',(-20.1307450473233,64.0352139646386,33.4461169673585));
#32011=CARTESIAN_POINT('Ctrl Pts',(-21.7215952795671,65.0441819602404,33.3349838493669));
#32012=CARTESIAN_POINT('Ctrl Pts',(-21.7367737504501,66.9279522462476,33.2238507313754));
#32013=CARTESIAN_POINT('Ctrl Pts',(-20.1623885262583,67.9624241127519,33.1127176133838));
#32014=CARTESIAN_POINT('Ctrl Pts',(-18.4393789312417,67.2008081909514,33.0015844953923));
#32015=CARTESIAN_POINT('Ctrl Pts',(-18.144711163821,65.3401653494693,32.8904513774007));
#32016=CARTESIAN_POINT('Ctrl Pts',(-19.5480767627175,64.0834291509782,32.7793182594092));
#32017=CARTESIAN_POINT('Ctrl Pts',(-21.3650602959056,64.580814029012,32.6681851414176));
#32018=CARTESIAN_POINT('Ctrl Pts',(-21.9326869180286,66.3770937663063,32.557052023426));
#32019=CARTESIAN_POINT('Ctrl Pts',(-20.7314424029572,67.8282424464125,32.4459189054344));
#32020=CARTESIAN_POINT('Ctrl Pts',(-18.8607530114064,67.6061116806398,32.334785787443));
#32021=CARTESIAN_POINT('Ctrl Pts',(-18.0327473041412,65.9140042888062,32.2236526694513));
#32022=CARTESIAN_POINT('Ctrl Pts',(-19.0052486944375,64.3006035566151,32.1125195514598));
#32023=CARTESIAN_POINT('Ctrl Pts',(-20.8881856326145,64.2425573370022,32.0013864334682));
#32024=CARTESIAN_POINT('Ctrl Pts',(-21.9582201211768,65.7929918148341,31.8902533154766));
#32025=CARTESIAN_POINT('Ctrl Pts',(-21.2360144800452,67.5328883314924,31.7791201974851));
#32026=CARTESIAN_POINT('Ctrl Pts',(-19.3825597377204,67.8698251132723,31.6679870794935));
#32027=CARTESIAN_POINT('Ctrl Pts',(-18.0942106256457,66.4954243557859,31.556853961502));
#32028=CARTESIAN_POINT('Ctrl Pts',(-18.5501149601189,64.6675917281717,31.4457208435104));
#32029=CARTESIAN_POINT('Ctrl Pts',(-20.3330111500104,64.0592315940133,31.3345877255189));
#32030=CARTESIAN_POINT('Ctrl Pts',(-21.8111224282211,65.2271390929139,31.2234546075273));
#32031=CARTESIAN_POINT('Ctrl Pts',(-21.6316231750398,67.1023993134887,31.1123214895358));
#32032=CARTESIAN_POINT('Ctrl Pts',(-19.9587981719997,67.9687002923444,31.0011883715442));
#32033=CARTESIAN_POINT('Ctrl Pts',(-18.3236827036336,67.0331692763581,30.8900552535526));
#32034=CARTESIAN_POINT('Ctrl Pts',(-18.2227988041078,65.1520410735024,30.7789221355611));
#32035=CARTESIAN_POINT('Ctrl Pts',(-19.7484793890201,64.0469982555154,30.6677890175695));
#32036=CARTESIAN_POINT('Ctrl Pts',(-21.5043615368559,64.7294195034804,30.5566558995779));
#32037=CARTESIAN_POINT('Ctrl Pts',(-21.8833927950681,66.5747260314211,30.4455227815864));
#32038=CARTESIAN_POINT('Ctrl Pts',(-20.538668837616,67.8940206744091,30.3343896635948));
#32039=CARTESIAN_POINT('Ctrl Pts',(-18.7009339581788,67.4798330482506,30.2232565456033));
#32040=CARTESIAN_POINT('Ctrl Pts',(-18.0521554509576,65.711243970672,30.1121234276117));
#32041=CARTESIAN_POINT('Ctrl Pts',(-19.1861209414343,64.2069357764609,30.0009903096202));
#32042=CARTESIAN_POINT('Ctrl Pts',(-21.0649805802779,64.343710533953,29.8898571916286));
#32043=CARTESIAN_POINT('Ctrl Pts',(-21.969128074824,65.9963866016894,29.7787240736371));
#32044=CARTESIAN_POINT('Ctrl Pts',(-21.0710520511653,67.6523697937816,29.6675909556455));
#32045=CARTESIAN_POINT('Ctrl Pts',(-19.1927070340822,67.7960391139636,29.5564578376539));
#32046=CARTESIAN_POINT('Ctrl Pts',(-18.0532283141485,66.2959027456354,29.4453247196623));
#32047=CARTESIAN_POINT('Ctrl Pts',(-18.695511665293,64.524944537883,29.3341916016708));
#32048=CARTESIAN_POINT('Ctrl Pts',(-20.5317140845218,64.1040151466775,29.2230584836793));
#32049=CARTESIAN_POINT('Ctrl Pts',(-21.8812708455339,65.418365718469,29.1119253656877));
#32050=CARTESIAN_POINT('Ctrl Pts',(-21.5090144826143,67.2650508776204,29.0007922476962));
#32051=CARTESIAN_POINT('Ctrl Pts',(-19.7556486709751,67.9539116816557,28.8896591297046));
#32052=CARTESIAN_POINT('Ctrl Pts',(-18.2259228132335,66.8544756094258,28.778526011713));
#32053=CARTESIAN_POINT('Ctrl Pts',(-18.3199022238194,64.9729898276167,28.6673928937215));
#32054=CARTESIAN_POINT('Ctrl Pts',(-19.9515732471676,64.0314641782998,28.5562597757299));
#32055=CARTESIAN_POINT('Ctrl Pts',(-21.6275663407708,64.891619993817,28.4451266577383));
#32056=CARTESIAN_POINT('Ctrl Pts',(-21.813946658905,66.7662088164062,28.3339935397468));
#32057=CARTESIAN_POINT('Ctrl Pts',(-20.3401315985817,67.9395331725326,28.2228604217552));
#32058=CARTESIAN_POINT('Ctrl Pts',(-18.555014711753,67.3377204298807,28.1117273037637));
#32059=CARTESIAN_POINT('Ctrl Pts',(-18.0924052348628,65.5115732976283,28.0005941857721));
#32060=CARTESIAN_POINT('Ctrl Pts',(-19.3757015690887,64.1324535076954,27.8894610677806));
#32061=CARTESIAN_POINT('Ctrl Pts',(-21.230380399702,64.4625857733909,27.7783279497889));
#32062=CARTESIAN_POINT('Ctrl Pts',(-21.958966660668,66.1998200513978,27.6671948317975));
#32063=CARTESIAN_POINT('Ctrl Pts',(-20.8946295306897,67.7541711533567,27.5560617138058));
#32064=CARTESIAN_POINT('Ctrl Pts',(-19.0114922398047,67.7030357725946,27.4449285958143));
#32065=CARTESIAN_POINT('Ctrl Pts',(-18.033076162612,66.0932150212516,27.3337954778227));
#32066=CARTESIAN_POINT('Ctrl Pts',(-18.8548661902409,64.3980802148824,27.2226623598312));
#32067=CARTESIAN_POINT('Ctrl Pts',(-20.7247277695829,64.1690854441478,27.1115292418396));
#32068=CARTESIAN_POINT('Ctrl Pts',(-21.931289935314,65.6158157443139,27.0003961238481));
#32069=CARTESIAN_POINT('Ctrl Pts',(-21.3702596049656,67.4141665860817,26.8892630058565));
#32070=CARTESIAN_POINT('Ctrl Pts',(-19.5551136165815,67.9182165282414,26.7781298878649));
#32071=CARTESIAN_POINT('Ctrl Pts',(-18.1471454253728,66.6666391615628,26.6669967698734));
#32072=CARTESIAN_POINT('Ctrl Pts',(-18.4349821331645,64.8049274791473,26.5558636518818));
#32073=CARTESIAN_POINT('Ctrl Pts',(-20.1551858585197,64.036993038762,26.4447305338903));
#32074=CARTESIAN_POINT('Ctrl Pts',(-21.7333552501256,65.0656801647588,26.3335974158987));
#32075=CARTESIAN_POINT('Ctrl Pts',(-21.725093935235,66.9494929160091,26.2224642979072));
#32076=CARTESIAN_POINT('Ctrl Pts',(-20.137950293138,67.9642936995585,26.1113311799155));
#32077=CARTESIAN_POINT('Ctrl Pts',(-18.424565977367,67.181292942287,26.0001980619241));
#32078=CARTESIAN_POINT('Ctrl Pts',(-18.1530472647236,65.317131638773,25.8890649439324));
#32079=CARTESIAN_POINT('Ctrl Pts',(-19.5719994257939,64.0779478702237,25.7779318259409));
#32080=CARTESIAN_POINT('Ctrl Pts',(-21.3825409080333,64.5979227300327,25.6667987079493));
#32081=CARTESIAN_POINT('Ctrl Pts',(-21.9279930020751,66.4010922846652,25.5556655899578));
#32082=CARTESIAN_POINT('Ctrl Pts',(-20.7083386979493,67.8372493839263,25.4445324719662));
#32083=CARTESIAN_POINT('Ctrl Pts',(-18.841444927279,67.5917176200702,25.3333993539747));
#32084=CARTESIAN_POINT('Ctrl Pts',(-18.0327841377349,65.8897199852641,25.2222662359831));
#32085=CARTESIAN_POINT('Ctrl Pts',(-19.0289370521585,64.2879148677798,25.1111331179916));
#32086=CARTESIAN_POINT('Ctrl Pts',(-20.2786416755829,64.2665677297147,25.0370443726639));
#32087=CARTESIAN_POINT('Ctrl Pts',(-20.7699020406705,64.5225674811446,25.));
#32088=CARTESIAN_POINT('Ctrl Pts',(-21.6638441182547,66.0009441583361,35.3785196366098));
#32089=CARTESIAN_POINT('Ctrl Pts',(-21.6649630220915,66.2166368308252,35.3641397488116));
#32090=CARTESIAN_POINT('Ctrl Pts',(-21.6260431008204,66.4319423603926,35.3497598610133));
#32091=CARTESIAN_POINT('Ctrl Pts',(-21.5452118232659,66.630154905384,35.335379973215));
#32092=CARTESIAN_POINT('Ctrl Pts',(-21.336980437136,67.1407749801941,35.2983356005512));
#32093=CARTESIAN_POINT('Ctrl Pts',(-20.8506079244041,67.5379589267428,35.2612912278873));
#32094=CARTESIAN_POINT('Ctrl Pts',(-20.3086785230682,67.6399608154928,35.2242468552234));
#32095=CARTESIAN_POINT('Ctrl Pts',(-19.7667491217323,67.7419627042429,35.1872024825596));
#32096=CARTESIAN_POINT('Ctrl Pts',(-19.1692628317925,67.5487825351942,35.1501581098958));
#32097=CARTESIAN_POINT('Ctrl Pts',(-18.7896358190473,67.1488167041591,35.1131137372319));
#32098=CARTESIAN_POINT('Ctrl Pts',(-18.4100088063022,66.748850873124,35.0760693645681));
#32099=CARTESIAN_POINT('Ctrl Pts',(-18.2482410707517,66.1420993801025,35.0390249919042));
#32100=CARTESIAN_POINT('Ctrl Pts',(-18.3783633795482,65.6062269851543,35.0019806192403));
#32101=CARTESIAN_POINT('Ctrl Pts',(-18.5084856883447,65.0703545902061,34.9649362465764));
#32102=CARTESIAN_POINT('Ctrl Pts',(-18.9304980414881,64.6053612933314,34.9278918739126));
#32103=CARTESIAN_POINT('Ctrl Pts',(-19.4512779429618,64.4240355048654,34.8908475012488));
#32104=CARTESIAN_POINT('Ctrl Pts',(-19.9720578444354,64.2427097163994,34.8538031285849));
#32105=CARTESIAN_POINT('Ctrl Pts',(-20.5916052942391,64.3450514363422,34.8167587559211));
#32106=CARTESIAN_POINT('Ctrl Pts',(-21.0264038579191,64.6842279188592,34.7797143832572));
#32107=CARTESIAN_POINT('Ctrl Pts',(-21.4223194165699,64.9930726524306,34.7459828010414));
#32108=CARTESIAN_POINT('Ctrl Pts',(-21.6650519066689,65.4982870444721,34.7122512188256));
#32109=CARTESIAN_POINT('Ctrl Pts',(-21.6682089013646,66.0008588710179,34.6785196366098));
#32110=CARTESIAN_POINT('Ctrl Pts',(-20.5301702171886,64.0148256743283,36.));
#32111=CARTESIAN_POINT('Ctrl Pts',(-20.5988349732706,64.0402496877953,36.));
#32112=CARTESIAN_POINT('Ctrl Pts',(-20.6657963847736,64.069563384374,36.));
#32113=CARTESIAN_POINT('Ctrl Pts',(-20.730865515262,64.1024727373112,36.));
#32114=CARTESIAN_POINT('Ctrl Pts',(-20.7977456115802,64.1362980040343,36.));
#32115=CARTESIAN_POINT('Ctrl Pts',(-20.8626274029816,64.1739225452161,36.));
#32116=CARTESIAN_POINT('Ctrl Pts',(-20.9252745196845,64.2150717403274,36.));
#32117=CARTESIAN_POINT('Ctrl Pts',(-20.9782072426395,64.2498401232839,36.));
#32118=CARTESIAN_POINT('Ctrl Pts',(-21.0295442643604,64.2871258592549,36.));
#32119=CARTESIAN_POINT('Ctrl Pts',(-21.0791202642708,64.3267813067489,36.));
#32120=CARTESIAN_POINT('Ctrl Pts',(-21.101149928935,64.3444026600646,36.));
#32121=CARTESIAN_POINT('Ctrl Pts',(-21.1228315640659,64.3624921087365,36.));
#32122=CARTESIAN_POINT('Ctrl Pts',(-21.1441491105767,64.3810374223025,36.));
#32123=CARTESIAN_POINT('Ctrl Pts',(-21.1558616839704,64.3912268381502,36.));
#32124=CARTESIAN_POINT('Ctrl Pts',(-21.1674643296591,64.4015538757899,36.));
#32125=CARTESIAN_POINT('Ctrl Pts',(-21.1789542498192,64.4120165483206,36.));
#32126=CARTESIAN_POINT('Ctrl Pts',(-21.1895478048553,64.421662994574,36.));
#32127=CARTESIAN_POINT('Ctrl Pts',(-21.2000469702932,64.4314262540256,36.));
#32128=CARTESIAN_POINT('Ctrl Pts',(-21.2104336655795,64.4412893138512,36.));
#32129=CARTESIAN_POINT('Ctrl Pts',(-21.2635184366823,64.4916978662139,36.));
#32130=CARTESIAN_POINT('Ctrl Pts',(-21.3137632137796,64.5447948198095,36.));
#32131=CARTESIAN_POINT('Ctrl Pts',(-21.3609493297492,64.6003207092003,36.));
#32132=CARTESIAN_POINT('Ctrl Pts',(-21.4077692882983,64.6554157257375,36.));
#32133=CARTESIAN_POINT('Ctrl Pts',(-21.4515783794455,64.7129030113309,36.));
#32134=CARTESIAN_POINT('Ctrl Pts',(-21.4921181954482,64.772553333862,36.));
#32135=CARTESIAN_POINT('Ctrl Pts',(-21.525806627261,64.8221225233982,36.));
#32136=CARTESIAN_POINT('Ctrl Pts',(-21.5572368021225,64.8731860598217,36.));
#32137=CARTESIAN_POINT('Ctrl Pts',(-21.5862328303999,64.9256188737153,36.));
#32138=CARTESIAN_POINT('Ctrl Pts',(-21.5983389970515,64.9475101609266,36.));
#32139=CARTESIAN_POINT('Ctrl Pts',(-21.6100205322312,64.9696401736576,36.));
#32140=CARTESIAN_POINT('Ctrl Pts',(-21.6212631934191,64.9919998924642,36.));
#32141=CARTESIAN_POINT('Ctrl Pts',(-21.6264640159837,65.0023434337455,36.));
#32142=CARTESIAN_POINT('Ctrl Pts',(-21.6315709088334,65.0127361311819,36.));
#32143=CARTESIAN_POINT('Ctrl Pts',(-21.6365823968231,65.0231770899229,36.));
#32144=CARTESIAN_POINT('Ctrl Pts',(-21.6418143886053,65.0340774473501,36.));
#32145=CARTESIAN_POINT('Ctrl Pts',(-21.6469387858192,65.0450229538182,36.));
#32146=CARTESIAN_POINT('Ctrl Pts',(-21.6519525299279,65.0560083018318,36.));
#32147=CARTESIAN_POINT('Ctrl Pts',(-21.6804929294147,65.1185416529592,36.));
#32148=CARTESIAN_POINT('Ctrl Pts',(-21.7054723575398,65.1824080698791,36.));
#32149=CARTESIAN_POINT('Ctrl Pts',(-21.7266673544266,65.2474030994014,36.));
#32150=CARTESIAN_POINT('Ctrl Pts',(-21.7458698278921,65.3062880021194,36.));
#32151=CARTESIAN_POINT('Ctrl Pts',(-21.7619656445149,65.3660998899564,36.));
#32152=CARTESIAN_POINT('Ctrl Pts',(-21.7747519290966,65.4266915444502,36.));
#32153=CARTESIAN_POINT('Ctrl Pts',(-21.7898844361711,65.498401479766,36.));
#32154=CARTESIAN_POINT('Ctrl Pts',(-21.800382014036,65.5712051224472,36.));
#32155=CARTESIAN_POINT('Ctrl Pts',(-21.8063198015774,65.6446793714796,36.));
#32156=CARTESIAN_POINT('Ctrl Pts',(-21.8076266251147,65.6608500204544,36.));
#32157=CARTESIAN_POINT('Ctrl Pts',(-21.8087123585312,65.6770530703594,36.));
#32158=CARTESIAN_POINT('Ctrl Pts',(-21.8095774335713,65.6932838463402,36.));
#32159=CARTESIAN_POINT('Ctrl Pts',(-21.8104727633698,65.7100822704259,36.));
#32160=CARTESIAN_POINT('Ctrl Pts',(-21.8111317404483,65.726916588365,36.));
#32161=CARTESIAN_POINT('Ctrl Pts',(-21.8115542824738,65.7437473430029,36.));
#32162=CARTESIAN_POINT('Ctrl Pts',(-21.8132755281181,65.8123082466785,36.));
#32163=CARTESIAN_POINT('Ctrl Pts',(-21.8110851681684,65.880896724124,36.));
#32164=CARTESIAN_POINT('Ctrl Pts',(-21.805103786848,65.9491744499936,36.));
#32165=CARTESIAN_POINT('Ctrl Pts',(-21.7991236414508,66.0174380677464,36.));
#32166=CARTESIAN_POINT('Ctrl Pts',(-21.7893535875248,66.0853921339257,36.));
#32167=CARTESIAN_POINT('Ctrl Pts',(-21.7758645295054,66.1526834998075,36.));
#32168=CARTESIAN_POINT('Ctrl Pts',(-21.7661045372626,66.2013720893343,36.));
#32169=CARTESIAN_POINT('Ctrl Pts',(-21.754396511133,66.2497134745457,36.));
#32170=CARTESIAN_POINT('Ctrl Pts',(-21.7407531062633,66.2975642349732,36.));
#32171=CARTESIAN_POINT('Ctrl Pts',(-21.7305167536077,66.3334656293283,36.));
#32172=CARTESIAN_POINT('Ctrl Pts',(-21.7191906927092,66.3690906873999,36.));
#32173=CARTESIAN_POINT('Ctrl Pts',(-21.7067763533949,66.4043746598269,36.));
#32174=CARTESIAN_POINT('Ctrl Pts',(-21.7026468248699,66.4161115849203,36.));
#32175=CARTESIAN_POINT('Ctrl Pts',(-21.6984000721287,66.4278015750603,36.));
#32176=CARTESIAN_POINT('Ctrl Pts',(-21.6940367401084,66.4394420694249,36.));
#32177=CARTESIAN_POINT('Ctrl Pts',(-21.6709127910537,66.5011321258786,36.));
#32178=CARTESIAN_POINT('Ctrl Pts',(-21.6445162548684,66.5614386479359,36.));
#32179=CARTESIAN_POINT('Ctrl Pts',(-21.6148971262233,66.6200275442078,36.));
#32180=CARTESIAN_POINT('Ctrl Pts',(-21.5940647936945,66.6612354873671,36.));
#32181=CARTESIAN_POINT('Ctrl Pts',(-21.5716374289325,66.701593212762,36.));
#32182=CARTESIAN_POINT('Ctrl Pts',(-21.5476220256553,66.7409731314567,36.));
#32183=CARTESIAN_POINT('Ctrl Pts',(-21.5399090083264,66.7536207639698,36.));
#32184=CARTESIAN_POINT('Ctrl Pts',(-21.5320310277768,66.7661691422738,36.));
#32185=CARTESIAN_POINT('Ctrl Pts',(-21.5239916401704,66.7786084047584,36.));
#32186=CARTESIAN_POINT('Ctrl Pts',(-21.4897471261491,66.8315945921934,36.));
#32187=CARTESIAN_POINT('Ctrl Pts',(-21.4526468486123,66.8824969904464,36.));
#32188=CARTESIAN_POINT('Ctrl Pts',(-21.4127250449828,66.9310003772166,36.));
#32189=CARTESIAN_POINT('Ctrl Pts',(-21.375938254522,66.9756948489973,36.));
#32190=CARTESIAN_POINT('Ctrl Pts',(-21.3367550941085,67.018352392206,36.));
#32191=CARTESIAN_POINT('Ctrl Pts',(-21.2951809127703,67.0586934718916,36.));
#32192=CARTESIAN_POINT('Ctrl Pts',(-21.287362563767,67.0662799265132,36.));
#32193=CARTESIAN_POINT('Ctrl Pts',(-21.2794596015101,67.0737843544158,36.));
#32194=CARTESIAN_POINT('Ctrl Pts',(-21.2714736181291,67.081206089647,36.));
#32195=CARTESIAN_POINT('Origin',(-20.,66.,30.));
#32196=CARTESIAN_POINT('Origin',(20.,-66.,25.));
#32197=CARTESIAN_POINT('Ctrl Pts',(19.2300979593296,-67.4774325188554,25.));
#32198=CARTESIAN_POINT('Ctrl Pts',(19.2818392509066,-67.5125051802703,25.));
#32199=CARTESIAN_POINT('Ctrl Pts',(19.3355570235436,-67.5443227583893,25.));
#32200=CARTESIAN_POINT('Ctrl Pts',(19.3909199784615,-67.5729492931195,25.));
#32201=CARTESIAN_POINT('Ctrl Pts',(19.4260302284271,-67.5911037574452,25.));
#32202=CARTESIAN_POINT('Ctrl Pts',(19.4618030444597,-67.6079741743555,25.));
#32203=CARTESIAN_POINT('Ctrl Pts',(19.4981615280073,-67.6235696646503,25.));
#32204=CARTESIAN_POINT('Ctrl Pts',(19.5229478187718,-67.6342014160147,25.));
#32205=CARTESIAN_POINT('Ctrl Pts',(19.5480064116943,-67.6442405386499,25.));
#32206=CARTESIAN_POINT('Ctrl Pts',(19.5733141854998,-67.6536883376551,25.));
#32207=CARTESIAN_POINT('Ctrl Pts',(19.5868028134417,-67.6587238594133,25.));
#32208=CARTESIAN_POINT('Ctrl Pts',(19.600362177991,-67.6635912278487,25.));
#32209=CARTESIAN_POINT('Ctrl Pts',(19.6139750771008,-67.6682861195686,25.));
#32210=CARTESIAN_POINT('Ctrl Pts',(19.6763395178067,-67.6897947118182,25.));
#32211=CARTESIAN_POINT('Ctrl Pts',(19.7398952542217,-67.7077136324119,25.));
#32212=CARTESIAN_POINT('Ctrl Pts',(19.8042923951479,-67.7220894217911,25.));
#32213=CARTESIAN_POINT('Ctrl Pts',(19.8507447452963,-67.7324592797118,25.));
#32214=CARTESIAN_POINT('Ctrl Pts',(19.8976358065701,-67.7409846995403,25.));
#32215=CARTESIAN_POINT('Ctrl Pts',(19.9448433633825,-67.7476691194456,25.));
#32216=CARTESIAN_POINT('Ctrl Pts',(19.9577433322521,-67.7494957085452,25.));
#32217=CARTESIAN_POINT('Ctrl Pts',(19.9706669674625,-67.7511847572499,25.));
#32218=CARTESIAN_POINT('Ctrl Pts',(19.9836118418914,-67.7527361749649,25.));
#32219=CARTESIAN_POINT('Ctrl Pts',(19.9969414186446,-67.754333698496,25.));
#32220=CARTESIAN_POINT('Ctrl Pts',(20.0102855922404,-67.755784299122,25.));
#32221=CARTESIAN_POINT('Ctrl Pts',(20.0236361127826,-67.7570879007368,25.));
#32222=CARTESIAN_POINT('Ctrl Pts',(20.0911672976909,-67.7636819328885,25.));
#32223=CARTESIAN_POINT('Ctrl Pts',(20.1589021638891,-67.7665235696462,25.));
#32224=CARTESIAN_POINT('Ctrl Pts',(20.2264860370306,-67.7656607588407,25.));
#32225=CARTESIAN_POINT('Ctrl Pts',(20.2950484463622,-67.7647854555343,25.));
#32226=CARTESIAN_POINT('Ctrl Pts',(20.3634564684948,-67.7600979895892,25.));
#32227=CARTESIAN_POINT('Ctrl Pts',(20.4313612906511,-67.7516001272965,25.));
#32228=CARTESIAN_POINT('Ctrl Pts',(20.4734291139411,-67.7463356032476,25.));
#32229=CARTESIAN_POINT('Ctrl Pts',(20.5153041791594,-67.739607699183,25.));
#32230=CARTESIAN_POINT('Ctrl Pts',(20.5569049276303,-67.731406890815,25.));
#32231=CARTESIAN_POINT('Ctrl Pts',(20.5909685558849,-67.7246918845254,25.));
#32232=CARTESIAN_POINT('Ctrl Pts',(20.6248483029251,-67.7169892041243,25.));
#32233=CARTESIAN_POINT('Ctrl Pts',(20.6584990498341,-67.7082896385505,25.));
#32234=CARTESIAN_POINT('Ctrl Pts',(20.6722821167333,-67.704726368629,25.));
#32235=CARTESIAN_POINT('Ctrl Pts',(20.6860292290737,-67.7009949721105,25.));
#32236=CARTESIAN_POINT('Ctrl Pts',(20.6997140296679,-67.6971016570004,25.));
#32237=CARTESIAN_POINT('Ctrl Pts',(20.7675093077033,-67.6778139532044,25.));
#32238=CARTESIAN_POINT('Ctrl Pts',(20.8338949911143,-67.6545270467904,25.));
#32239=CARTESIAN_POINT('Ctrl Pts',(20.898508351168,-67.6272596461893,25.));
#32240=CARTESIAN_POINT('Ctrl Pts',(20.9056750502645,-67.6242352367624,25.));
#32241=CARTESIAN_POINT('Ctrl Pts',(20.9128199532954,-67.6211618050839,25.));
#32242=CARTESIAN_POINT('Ctrl Pts',(20.9199425694434,-67.6180393373165,25.));
#32243=CARTESIAN_POINT('Ctrl Pts',(20.9816951205624,-67.5909677745065,25.));
#32244=CARTESIAN_POINT('Ctrl Pts',(21.0417732412363,-67.5602146096881,25.));
#32245=CARTESIAN_POINT('Ctrl Pts',(21.1000349944499,-67.5260900451755,25.));
#32246=CARTESIAN_POINT('Ctrl Pts',(21.162710887036,-67.4893800695575,25.));
#32247=CARTESIAN_POINT('Ctrl Pts',(21.2232857612189,-67.4487684714382,25.));
#32248=CARTESIAN_POINT('Ctrl Pts',(21.281563029017,-67.4045803567109,25.));
#32249=CARTESIAN_POINT('Ctrl Pts',(21.2920881592725,-67.3965997893161,25.));
#32250=CARTESIAN_POINT('Ctrl Pts',(21.3025382728815,-67.3885024149022,25.));
#32251=CARTESIAN_POINT('Ctrl Pts',(21.3129121067363,-67.3802899597523,25.));
#32252=CARTESIAN_POINT('Ctrl Pts',(21.3220882756753,-67.3730256371388,25.));
#32253=CARTESIAN_POINT('Ctrl Pts',(21.3311977619232,-67.3656767917098,25.));
#32254=CARTESIAN_POINT('Ctrl Pts',(21.340237913509,-67.3582467210556,25.));
#32255=CARTESIAN_POINT('Ctrl Pts',(21.3951411261676,-67.31312195237,25.));
#32256=CARTESIAN_POINT('Ctrl Pts',(21.4475122197521,-67.2649864357061,25.));
#32257=CARTESIAN_POINT('Ctrl Pts',(21.4972011756428,-67.2141901758274,25.));
#32258=CARTESIAN_POINT('Ctrl Pts',(21.5479379013916,-67.1623227968428,25.));
#32259=CARTESIAN_POINT('Ctrl Pts',(21.5958789474072,-67.1076807385324,25.));
#32260=CARTESIAN_POINT('Ctrl Pts',(21.6408443956269,-67.0505853273705,25.));
#32261=CARTESIAN_POINT('Ctrl Pts',(21.6860826148688,-66.9931435619682,25.));
#32262=CARTESIAN_POINT('Ctrl Pts',(21.7283098131003,-66.9332178592765,25.));
#32263=CARTESIAN_POINT('Ctrl Pts',(21.7673108256436,-66.8710938870854,25.));
#32264=CARTESIAN_POINT('Ctrl Pts',(21.7769378410941,-66.855759197006,25.));
#32265=CARTESIAN_POINT('Ctrl Pts',(21.7863681009519,-66.8402903992017,25.));
#32266=CARTESIAN_POINT('Ctrl Pts',(21.7955979845278,-66.8246914847445,25.));
#32267=CARTESIAN_POINT('Ctrl Pts',(21.8028476850435,-66.8124391678809,25.));
#32268=CARTESIAN_POINT('Ctrl Pts',(21.8099745027199,-66.8001050249419,25.));
#32269=CARTESIAN_POINT('Ctrl Pts',(21.8169662172758,-66.7877100692794,25.));
#32270=CARTESIAN_POINT('Ctrl Pts',(21.8539814596018,-66.722089214223,25.));
#32271=CARTESIAN_POINT('Ctrl Pts',(21.8872826215013,-66.6546514104225,25.));
#32272=CARTESIAN_POINT('Ctrl Pts',(21.9166889688907,-66.5857429831168,25.));
#32273=CARTESIAN_POINT('Ctrl Pts',(21.9461273939939,-66.5167593875222,25.));
#32274=CARTESIAN_POINT('Ctrl Pts',(21.9716632676734,-66.4463011289855,25.));
#32275=CARTESIAN_POINT('Ctrl Pts',(21.9930795264615,-66.3746779559458,25.));
#32276=CARTESIAN_POINT('Ctrl Pts',(22.0140085505991,-66.3046842594656,25.));
#32277=CARTESIAN_POINT('Ctrl Pts',(22.0310038329003,-66.2335771734604,25.));
#32278=CARTESIAN_POINT('Ctrl Pts',(22.0438191861901,-66.1616225716972,25.));
#32279=CARTESIAN_POINT('Ctrl Pts',(22.0465680471256,-66.1461884912282,25.));
#32280=CARTESIAN_POINT('Ctrl Pts',(22.0491244126747,-66.1307153578235,25.));
#32281=CARTESIAN_POINT('Ctrl Pts',(22.0514855454828,-66.1152057111006,25.));
#32282=CARTESIAN_POINT('Ctrl Pts',(22.0534987389493,-66.1019815843837,25.));
#32283=CARTESIAN_POINT('Ctrl Pts',(22.0553699972796,-66.0887309121952,25.));
#32284=CARTESIAN_POINT('Ctrl Pts',(22.0571001480269,-66.0754553928761,25.));
#32285=CARTESIAN_POINT('Ctrl Pts',(21.8174278887595,-65.0413794120408,25.));
#32286=CARTESIAN_POINT('Ctrl Pts',(21.776581404545,-64.9788996392346,25.));
#32287=CARTESIAN_POINT('Ctrl Pts',(21.7321382352854,-64.9189705873501,25.));
#32288=CARTESIAN_POINT('Ctrl Pts',(21.6844272287858,-64.8617420298968,25.));
#32289=CARTESIAN_POINT('Ctrl Pts',(21.6379676706942,-64.8060145639606,25.));
#32290=CARTESIAN_POINT('Ctrl Pts',(21.5884084602278,-64.7528475767717,25.));
#32291=CARTESIAN_POINT('Ctrl Pts',(21.5360271780281,-64.7024170328902,25.));
#32292=CARTESIAN_POINT('Ctrl Pts',(21.5243355070385,-64.6911607729796,25.));
#32293=CARTESIAN_POINT('Ctrl Pts',(21.5125015752233,-64.6800395435489,25.));
#32294=CARTESIAN_POINT('Ctrl Pts',(21.500533454458,-64.6690602418449,25.));
#32295=CARTESIAN_POINT('Ctrl Pts',(21.4456122822129,-64.6186767161566,25.));
#32296=CARTESIAN_POINT('Ctrl Pts',(21.3879773812488,-64.5713776698141,25.));
#32297=CARTESIAN_POINT('Ctrl Pts',(21.3279448973862,-64.5273355904878,25.));
#32298=CARTESIAN_POINT('Ctrl Pts',(21.285800416715,-64.4964168204909,25.));
#32299=CARTESIAN_POINT('Ctrl Pts',(21.2424736210485,-64.4671041191484,25.));
#32300=CARTESIAN_POINT('Ctrl Pts',(21.1980685681425,-64.439471567851,25.));
#32301=CARTESIAN_POINT('Ctrl Pts',(21.1811931522648,-64.4289702675622,25.));
#32302=CARTESIAN_POINT('Ctrl Pts',(21.1641619799486,-64.4187117531234,25.));
#32303=CARTESIAN_POINT('Ctrl Pts',(21.1469806872212,-64.4087005778126,25.));
#32304=CARTESIAN_POINT('Ctrl Pts',(21.1305959674615,-64.3991535486957,25.));
#32305=CARTESIAN_POINT('Ctrl Pts',(21.1140694086939,-64.3898287196359,25.));
#32306=CARTESIAN_POINT('Ctrl Pts',(21.0974354907253,-64.380745947404,25.));
#32307=CARTESIAN_POINT('Ctrl Pts',(21.0337185410866,-64.3459539914757,25.));
#32308=CARTESIAN_POINT('Ctrl Pts',(20.9683626351681,-64.3146691870302,25.));
#32309=CARTESIAN_POINT('Ctrl Pts',(20.9016594733476,-64.2870531698814,25.));
#32310=CARTESIAN_POINT('Ctrl Pts',(20.8363886507365,-64.2600301606663,25.));
#32311=CARTESIAN_POINT('Ctrl Pts',(20.7698268866709,-64.2365199143679,25.));
#32312=CARTESIAN_POINT('Ctrl Pts',(20.7022388874947,-64.216722135039,25.));
#32313=CARTESIAN_POINT('Ctrl Pts',(20.6361332105615,-64.1973585554056,25.));
#32314=CARTESIAN_POINT('Ctrl Pts',(20.5690450572908,-64.1815462756357,25.));
#32315=CARTESIAN_POINT('Ctrl Pts',(20.5012260301962,-64.1695207315524,25.));
#32316=CARTESIAN_POINT('Ctrl Pts',(20.4791658489428,-64.1656090611331,25.));
#32317=CARTESIAN_POINT('Ctrl Pts',(20.4570284148415,-64.1620984514521,25.));
#32318=CARTESIAN_POINT('Ctrl Pts',(20.4348226814172,-64.158998178911,25.));
#32319=CARTESIAN_POINT('Ctrl Pts',(20.4223381809779,-64.1572551446612,25.));
#32320=CARTESIAN_POINT('Ctrl Pts',(20.4098308067038,-64.155641770794,25.));
#32321=CARTESIAN_POINT('Ctrl Pts',(20.3973198538599,-64.1541615852412,25.));
#32322=CARTESIAN_POINT('Ctrl Pts',(20.3294892107318,-64.1461364620353,25.));
#32323=CARTESIAN_POINT('Ctrl Pts',(20.2614350334953,-64.1420045587359,25.));
#32324=CARTESIAN_POINT('Ctrl Pts',(20.1934030453685,-64.1419439160697,25.));
#32325=CARTESIAN_POINT('Ctrl Pts',(20.1836061137927,-64.1419351832358,25.));
#32326=CARTESIAN_POINT('Ctrl Pts',(20.1738096485656,-64.1420109658147,25.));
#32327=CARTESIAN_POINT('Ctrl Pts',(20.1640143929054,-64.1421718854656,25.));
#32328=CARTESIAN_POINT('Ctrl Pts',(20.094650154852,-64.1433114237648,25.));
#32329=CARTESIAN_POINT('Ctrl Pts',(20.0253451150382,-64.1487162439491,25.));
#32330=CARTESIAN_POINT('Ctrl Pts',(19.9564242806281,-64.1582131178836,25.));
#32331=CARTESIAN_POINT('Ctrl Pts',(19.8921290095081,-64.1670726171864,25.));
#32332=CARTESIAN_POINT('Ctrl Pts',(19.8281675897192,-64.1794942557964,25.));
#32333=CARTESIAN_POINT('Ctrl Pts',(19.7648243951104,-64.1953718384076,25.));
#32334=CARTESIAN_POINT('Ctrl Pts',(19.7509597565193,-64.1988471437813,25.));
#32335=CARTESIAN_POINT('Ctrl Pts',(19.7371248349099,-64.2024881308436,25.));
#32336=CARTESIAN_POINT('Ctrl Pts',(19.7233227901375,-64.2062938641054,25.));
#32337=CARTESIAN_POINT('Ctrl Pts',(19.7122623666812,-64.2093436311602,25.));
#32338=CARTESIAN_POINT('Ctrl Pts',(19.7012236018487,-64.2124991342566,25.));
#32339=CARTESIAN_POINT('Ctrl Pts',(19.6902211768855,-64.215755766339,25.));
#32340=CARTESIAN_POINT('Ctrl Pts',(19.6246589511318,-64.2351616744452,25.));
#32341=CARTESIAN_POINT('Ctrl Pts',(19.5602630981036,-64.2581875826496,25.));
#32342=CARTESIAN_POINT('Ctrl Pts',(19.4973360772709,-64.2846514713848,25.));
#32343=CARTESIAN_POINT('Ctrl Pts',(19.4347004138036,-64.3109928301035,25.));
#32344=CARTESIAN_POINT('Ctrl Pts',(19.3735191200478,-64.3407411090656,25.));
#32345=CARTESIAN_POINT('Ctrl Pts',(19.31412026665,-64.3737583558761,25.));
#32346=CARTESIAN_POINT('Ctrl Pts',(19.2559941313215,-64.4060681539024,25.));
#32347=CARTESIAN_POINT('Ctrl Pts',(19.1995741988762,-64.4415090370213,25.));
#32348=CARTESIAN_POINT('Ctrl Pts',(19.1452078375279,-64.4799811312036,25.));
#32349=CARTESIAN_POINT('Ctrl Pts',(19.1337113467811,-64.4881165675986,25.));
#32350=CARTESIAN_POINT('Ctrl Pts',(19.1223068502292,-64.4963876354851,25.));
#32351=CARTESIAN_POINT('Ctrl Pts',(19.1109979108722,-64.5047935191582,25.));
#32352=CARTESIAN_POINT('Ctrl Pts',(19.1003667878726,-64.5126955849869,25.));
#32353=CARTESIAN_POINT('Ctrl Pts',(19.0898188788728,-64.5207179018802,25.));
#32354=CARTESIAN_POINT('Ctrl Pts',(19.0793737230102,-64.5288465311509,25.));
#32355=CARTESIAN_POINT('Ctrl Pts',(19.0278062973887,-64.5689773334901,25.));
#32356=CARTESIAN_POINT('Ctrl Pts',(18.9786454464034,-64.6117656226463,25.));
#32357=CARTESIAN_POINT('Ctrl Pts',(18.9321822501578,-64.6570793867845,25.));
#32358=CARTESIAN_POINT('Ctrl Pts',(18.8866027003471,-64.7015313646193,25.));
#32359=CARTESIAN_POINT('Ctrl Pts',(18.8436185894728,-64.7484143331547,25.));
#32360=CARTESIAN_POINT('Ctrl Pts',(18.803547221108,-64.7976294314002,25.));
#32361=CARTESIAN_POINT('Ctrl Pts',(18.7647769773783,-64.8452465064347,25.));
#32362=CARTESIAN_POINT('Ctrl Pts',(18.7287330514718,-64.8950472934368,25.));
#32363=CARTESIAN_POINT('Ctrl Pts',(18.6957494965908,-64.9469576149125,25.));
#32364=CARTESIAN_POINT('Ctrl Pts',(18.6902971623536,-64.9555386312423,25.));
#32365=CARTESIAN_POINT('Ctrl Pts',(18.6849285675962,-64.9641773162184,25.));
#32366=CARTESIAN_POINT('Ctrl Pts',(18.6796453590658,-64.9728733607135,25.));
#32367=CARTESIAN_POINT('Ctrl Pts',(18.6739897755669,-64.9821823261781,25.));
#32368=CARTESIAN_POINT('Ctrl Pts',(18.6684320396214,-64.9915570228288,25.));
#32369=CARTESIAN_POINT('Ctrl Pts',(18.6629725546622,-65.0009957901906,25.));
#32370=CARTESIAN_POINT('Origin',(20.,-66.,37.5459252805377));
#32371=CARTESIAN_POINT('Ctrl Pts',(17.9434279331127,-65.9985037039655,35.7959252805377));
#32372=CARTESIAN_POINT('Ctrl Pts',(17.9426109898666,-65.9003307306121,35.7905876687522));
#32373=CARTESIAN_POINT('Ctrl Pts',(17.9936360911193,-65.1216409581897,35.7482056843029));
#32374=CARTESIAN_POINT('Ctrl Pts',(18.9885907005499,-63.7918186870749,35.6687793271897));
#32375=CARTESIAN_POINT('Ctrl Pts',(21.3064559759895,-63.9528111531126,35.5576462091981));
#32376=CARTESIAN_POINT('Ctrl Pts',(22.4285781341657,-65.9871398034319,35.4465130912066));
#32377=CARTESIAN_POINT('Ctrl Pts',(21.3279816257553,-68.0334049278494,35.335379973215));
#32378=CARTESIAN_POINT('Ctrl Pts',(19.0119582319098,-68.2185344164948,35.2242468552235));
#32379=CARTESIAN_POINT('Ctrl Pts',(17.9980259839472,-66.8931862532338,35.144428624331));
#32380=CARTESIAN_POINT('Ctrl Pts',(17.9427193968075,-66.1070372217313,35.1016547661024));
#32381=CARTESIAN_POINT('Ctrl Pts',(17.9436250231948,-66.0016062109329,35.0959252805377));
#32382=CARTESIAN_POINT('Ctrl Pts',(17.9473272127329,-66.0023217579764,35.8540747194623));
#32383=CARTESIAN_POINT('Ctrl Pts',(17.9508754656456,-65.5321727435478,35.8286277343139));
#32384=CARTESIAN_POINT('Ctrl Pts',(18.3433679905248,-64.3705970778618,35.7661363765015));
#32385=CARTESIAN_POINT('Ctrl Pts',(20.2718170744413,-63.5871690673869,35.6666006460253));
#32386=CARTESIAN_POINT('Ctrl Pts',(22.1745314797546,-64.9187024309931,35.5554675280338));
#32387=CARTESIAN_POINT('Ctrl Pts',(22.0878551535464,-67.240916575683,35.4443344100422));
#32388=CARTESIAN_POINT('Ctrl Pts',(20.0898773540102,-68.4268764895147,35.3332012920506));
#32389=CARTESIAN_POINT('Ctrl Pts',(18.2789900436016,-67.5258396316566,35.2364480618574));
#32390=CARTESIAN_POINT('Ctrl Pts',(17.950084108963,-66.4181209144086,35.1767392043279));
#32391=CARTESIAN_POINT('Ctrl Pts',(17.9479090675131,-65.9988355335402,35.1540747194623));
#32392=CARTESIAN_POINT('Ctrl Pts',(21.2690708798524,-64.9206413469514,36.));
#32393=CARTESIAN_POINT('Ctrl Pts',(21.627967898288,-65.3426194852432,35.9629556273362));
#32394=CARTESIAN_POINT('Ctrl Pts',(21.8852406895061,-66.5657423547737,35.8888668820085));
#32395=CARTESIAN_POINT('Ctrl Pts',(20.5452621419689,-67.8933537625408,35.7777337640169));
#32396=CARTESIAN_POINT('Ctrl Pts',(18.7059925990704,-67.4836984587995,35.6666006460253));
#32397=CARTESIAN_POINT('Ctrl Pts',(18.0511941008261,-65.7182471306277,35.5554675280338));
#32398=CARTESIAN_POINT('Ctrl Pts',(19.1799450576061,-64.2095972418381,35.4443344100422));
#32399=CARTESIAN_POINT('Ctrl Pts',(21.0592800369867,-64.3401306149583,35.3332012920507));
#32400=CARTESIAN_POINT('Ctrl Pts',(21.9691014340041,-65.9895728981713,35.2220681740591));
#32401=CARTESIAN_POINT('Ctrl Pts',(21.0767331249584,-67.6486933251233,35.1109350560675));
#32402=CARTESIAN_POINT('Ctrl Pts',(19.198891550973,-67.7987970983723,34.999801938076));
#32403=CARTESIAN_POINT('Ctrl Pts',(18.0542583326729,-66.302604885796,34.8886688200844));
#32404=CARTESIAN_POINT('Ctrl Pts',(18.6904432824267,-64.5294397602479,34.7775357020929));
#32405=CARTESIAN_POINT('Ctrl Pts',(20.525186680335,-64.1021977783242,34.6664025841013));
#32406=CARTESIAN_POINT('Ctrl Pts',(21.8792582580528,-65.4118948076596,34.5552694661098));
#32407=CARTESIAN_POINT('Ctrl Pts',(21.513358861174,-67.2598510025468,34.4441363481182));
#32408=CARTESIAN_POINT('Ctrl Pts',(19.7623737940666,-67.9547408964103,34.3330032301266));
#32409=CARTESIAN_POINT('Ctrl Pts',(18.2288736212496,-66.860575523791,34.2218701121351));
#32410=CARTESIAN_POINT('Ctrl Pts',(18.3163780021904,-64.9787772891694,34.1107369941435));
#32411=CARTESIAN_POINT('Ctrl Pts',(19.9447995117363,-64.0316424102007,33.999603876152));
#32412=CARTESIAN_POINT('Ctrl Pts',(21.6237426760499,-64.8860258031255,33.8884707581604));
#32413=CARTESIAN_POINT('Ctrl Pts',(21.8165726357416,-66.7599622607762,33.7773376401688));
#32414=CARTESIAN_POINT('Ctrl Pts',(20.3468038184027,-67.9383513284147,33.6662045221772));
#32415=CARTESIAN_POINT('Ctrl Pts',(18.5596264969971,-67.3426849761128,33.5550714041857));
#32416=CARTESIAN_POINT('Ctrl Pts',(18.0907356977871,-65.5181404817989,33.4439382861942));
#32417=CARTESIAN_POINT('Ctrl Pts',(19.3692787360241,-64.1346127865089,33.3328051682026));
#32418=CARTESIAN_POINT('Ctrl Pts',(21.2250826999231,-64.4583608888479,33.2216720502111));
#32419=CARTESIAN_POINT('Ctrl Pts',(21.9596427581053,-66.1930777845806,33.1105389322195));
#32420=CARTESIAN_POINT('Ctrl Pts',(20.9006606332631,-67.7510822921252,32.9994058142279));
#32421=CARTESIAN_POINT('Ctrl Pts',(19.017358447211,-67.7064273641261,32.8882726962364));
#32422=CARTESIAN_POINT('Ctrl Pts',(18.0334084866612,-66.0999829480836,32.7771395782448));
#32423=CARTESIAN_POINT('Ctrl Pts',(18.8493604834091,-64.4020302026989,32.6660064602532));
#32424=CARTESIAN_POINT('Ctrl Pts',(20.7184230544699,-64.1666023112654,32.5548733422617));
#32425=CARTESIAN_POINT('Ctrl Pts',(21.9299565692245,-65.6091721464001,32.4437402242701));
#32426=CARTESIAN_POINT('Ctrl Pts',(21.3751178694742,-67.4094430159797,32.3326071062786));
#32427=CARTESIAN_POINT('Ctrl Pts',(19.5617171714693,-67.9197361622001,32.221473988287));
#32428=CARTESIAN_POINT('Ctrl Pts',(18.1494501687797,-66.6730112126951,32.1103408702954));
#32429=CARTESIAN_POINT('Ctrl Pts',(18.4308792085545,-64.8103199118686,31.9992077523039));
#32430=CARTESIAN_POINT('Ctrl Pts',(20.1484293566527,-64.0364706530518,31.8880746343123));
#32431=CARTESIAN_POINT('Ctrl Pts',(21.7301311154199,-65.0597207363241,31.7769415163208));
#32432=CARTESIAN_POINT('Ctrl Pts',(21.7283487800576,-66.9435514107436,31.6658083983292));
#32433=CARTESIAN_POINT('Ctrl Pts',(20.1447136140416,-67.963806696229,31.5546752803377));
#32434=CARTESIAN_POINT('Ctrl Pts',(18.4286308525823,-67.1867087986473,31.4435421623461));
#32435=CARTESIAN_POINT('Ctrl Pts',(18.1507269833267,-65.3234883001403,31.3324090443545));
#32436=CARTESIAN_POINT('Ctrl Pts',(19.5653505656071,-64.079437936586,31.221275926363));
#32437=CARTESIAN_POINT('Ctrl Pts',(21.377782417879,-64.5931615660544,31.1101428083714));
#32438=CARTESIAN_POINT('Ctrl Pts',(21.9292135723205,-66.394479102891,30.9990096903798));
#32439=CARTESIAN_POINT('Ctrl Pts',(20.7149525322679,-67.8347538382155,30.8878765723883));
#32440=CARTESIAN_POINT('Ctrl Pts',(18.8463387944264,-67.5957896455979,30.7767434543967));
#32441=CARTESIAN_POINT('Ctrl Pts',(18.0336011995884,-65.8962959596606,30.6656103364052));
#32442=CARTESIAN_POINT('Ctrl Pts',(19.0205891835897,-64.2917162931933,30.5544772184136));
#32443=CARTESIAN_POINT('Ctrl Pts',(20.9039724960038,-64.2506251125867,30.443344100422));
#32444=CARTESIAN_POINT('Ctrl Pts',(21.9600046000645,-65.8106306836656,30.3322109824305));
#32445=CARTESIAN_POINT('Ctrl Pts',(21.2221633491169,-67.5439545065572,30.2210778644389));
#32446=CARTESIAN_POINT('Ctrl Pts',(19.3657500971768,-67.8641903955905,30.1099447464474));
#32447=CARTESIAN_POINT('Ctrl Pts',(18.0898273201334,-66.4782458607604,29.9988116284558));
#32448=CARTESIAN_POINT('Ctrl Pts',(18.562169763368,-64.6545918905887,29.8876785104643));
#32449=CARTESIAN_POINT('Ctrl Pts',(20.3504710316148,-64.0623083768974,29.7765453924727));
#32450=CARTESIAN_POINT('Ctrl Pts',(21.8180074173223,-65.2434765034687,29.6654122744811));
#32451=CARTESIAN_POINT('Ctrl Pts',(21.6216318586219,-67.1170447105401,29.5542791564896));
#32452=CARTESIAN_POINT('Ctrl Pts',(19.9410749961026,-67.9682496320738,29.443146038498));
#32453=CARTESIAN_POINT('Ctrl Pts',(18.3144486164159,-67.018035020783,29.3320129205064));
#32454=CARTESIAN_POINT('Ctrl Pts',(18.2305052056412,-65.1360746890036,29.2208798025149));
#32455=CARTESIAN_POINT('Ctrl Pts',(19.7660730773002,-64.044812805617,29.1097466845233));
#32456=CARTESIAN_POINT('Ctrl Pts',(21.515740075888,-64.7430151979478,28.9986135665318));
#32457=CARTESIAN_POINT('Ctrl Pts',(21.8781420980751,-66.5916595555565,28.8874804485402));
#32458=CARTESIAN_POINT('Ctrl Pts',(20.5215945491511,-67.8987938004266,28.7763473305487));
#32459=CARTESIAN_POINT('Ctrl Pts',(18.6876631390829,-67.4680772233507,28.6652142125571));
#32460=CARTESIAN_POINT('Ctrl Pts',(18.054834077201,-65.6937185885076,28.5540810945655));
#32461=CARTESIAN_POINT('Ctrl Pts',(19.2022974288504,-64.1996807565816,28.442947976574));
#32462=CARTESIAN_POINT('Ctrl Pts',(21.0798495708812,-64.3533659561062,28.3318148585824));
#32463=CARTESIAN_POINT('Ctrl Pts',(21.9690808831804,-66.0141154434886,28.2206817405909));
#32464=CARTESIAN_POINT('Ctrl Pts',(21.0561318689169,-67.6619459214081,28.1095486225993));
#32465=CARTESIAN_POINT('Ctrl Pts',(19.1765693992908,-67.7886980785084,27.9984155046078));
#32466=CARTESIAN_POINT('Ctrl Pts',(18.0506430253154,-66.2783633516724,27.8872823866161));
#32467=CARTESIAN_POINT('Ctrl Pts',(18.7088448805761,-64.5132595291411,27.7761492686247));
#32468=CARTESIAN_POINT('Ctrl Pts',(20.5487627203804,-64.1088791030149,27.665016150633));
#32469=CARTESIAN_POINT('Ctrl Pts',(21.8864313196484,-65.4353269557215,27.5538830326415));
#32470=CARTESIAN_POINT('Ctrl Pts',(21.4975637254705,-67.2785858036292,27.4427499146499));
#32471=CARTESIAN_POINT('Ctrl Pts',(19.738066867186,-67.9516325998814,27.3316167966584));
#32472=CARTESIAN_POINT('Ctrl Pts',(18.2183015196908,-66.8384684242688,27.2204836786668));
#32473=CARTESIAN_POINT('Ctrl Pts',(18.329216752231,-64.9579049468497,27.1093505606753));
#32474=CARTESIAN_POINT('Ctrl Pts',(19.9692985667656,-64.0311078747868,26.9982174426837));
#32475=CARTESIAN_POINT('Ctrl Pts',(21.637479556849,-64.9063183780325,26.8870843246922));
#32476=CARTESIAN_POINT('Ctrl Pts',(21.8069747751189,-66.7825093336883,26.7759512067006));
#32477=CARTESIAN_POINT('Ctrl Pts',(20.3226556188142,-67.942516977602,26.6648180887091));
#32478=CARTESIAN_POINT('Ctrl Pts',(18.5430292180468,-67.3246565676388,26.5536849707175));
#32479=CARTESIAN_POINT('Ctrl Pts',(18.0968800670332,-65.4944184471421,26.4425518527259));
#32480=CARTESIAN_POINT('Ctrl Pts',(19.3925406976308,-64.1269082277483,26.3314187347344));
#32481=CARTESIAN_POINT('Ctrl Pts',(21.2441729623769,-64.473725792196,26.2202856167428));
#32482=CARTESIAN_POINT('Ctrl Pts',(21.9570872251895,-66.2174486486474,26.1091524987512));
#32483=CARTESIAN_POINT('Ctrl Pts',(20.878802090704,-67.7621558105501,25.9980193807597));
#32484=CARTESIAN_POINT('Ctrl Pts',(18.9961949942118,-67.6940648934545,25.8868862627682));
#32485=CARTESIAN_POINT('Ctrl Pts',(18.0323251000736,-66.0755065322627,25.7757531447765));
#32486=CARTESIAN_POINT('Ctrl Pts',(18.8693181114084,-64.3878268177706,25.664620026785));
#32487=CARTESIAN_POINT('Ctrl Pts',(20.7412167237518,-64.1757009701585,25.5534869087934));
#32488=CARTESIAN_POINT('Ctrl Pts',(21.9346029210715,-65.6331865461314,25.4423537908019));
#32489=CARTESIAN_POINT('Ctrl Pts',(21.3576070345443,-67.4265115788993,25.3312206728103));
#32490=CARTESIAN_POINT('Ctrl Pts',(19.5375918595496,-67.9140030887383,25.2200875548188));
#32491=CARTESIAN_POINT('Ctrl Pts',(18.1417564769822,-66.6501901871505,25.1089544368272));
#32492=CARTESIAN_POINT('Ctrl Pts',(18.4447225902452,-64.7903672241964,24.9978213188356));
#32493=CARTESIAN_POINT('Ctrl Pts',(20.1751288422123,-64.0395085417223,24.8866882008441));
#32494=CARTESIAN_POINT('Ctrl Pts',(21.2151340020225,-64.7327675918889,24.8125994555164));
#32495=CARTESIAN_POINT('Ctrl Pts',(21.4735782273626,-65.2227463683951,24.7755550828525));
#32496=CARTESIAN_POINT('Ctrl Pts',(21.3677806246588,-64.8366876301902,36.0748149723825));
#32497=CARTESIAN_POINT('Ctrl Pts',(21.7545930524416,-65.2914876975058,36.0377705997186));
#32498=CARTESIAN_POINT('Ctrl Pts',(22.0318768075623,-66.6097464244853,35.9636818543909));
#32499=CARTESIAN_POINT('Ctrl Pts',(20.5876732379454,-68.0406209244431,35.8525487363994));
#32500=CARTESIAN_POINT('Ctrl Pts',(18.6053432639141,-67.5991021754578,35.7414156184078));
#32501=CARTESIAN_POINT('Ctrl Pts',(17.899613810049,-65.6963320790133,35.6302825004163));
#32502=CARTESIAN_POINT('Ctrl Pts',(19.1161602719207,-64.0703377235837,35.5191493824247));
#32503=CARTESIAN_POINT('Ctrl Pts',(21.1416720166543,-64.2110241276764,35.4080162644332));
#32504=CARTESIAN_POINT('Ctrl Pts',(22.122260334058,-65.9887618665916,35.2968831464416));
#32505=CARTESIAN_POINT('Ctrl Pts',(21.1604826252241,-67.776930526032,35.18575002845));
#32506=CARTESIAN_POINT('Ctrl Pts',(19.1365804446186,-67.9387095377464,35.0746169104585));
#32507=CARTESIAN_POINT('Ctrl Pts',(17.9029163812577,-66.3261418304446,34.9634837924669));
#32508=CARTESIAN_POINT('Ctrl Pts',(18.5885845041241,-64.4150579488825,34.8523506744754));
#32509=CARTESIAN_POINT('Ctrl Pts',(20.5660362845728,-63.9545846103219,34.7412175564838));
#32510=CARTESIAN_POINT('Ctrl Pts',(22.0254290559355,-65.3661513315646,34.6300844384922));
#32511=CARTESIAN_POINT('Ctrl Pts',(21.6310695969247,-67.3578436150398,34.5189513205007));
#32512=CARTESIAN_POINT('Ctrl Pts',(19.7438909634229,-68.1067828178749,34.4078182025091));
#32513=CARTESIAN_POINT('Ctrl Pts',(18.0911134412297,-66.9275120453744,34.2966850845175));
#32514=CARTESIAN_POINT('Ctrl Pts',(18.1854240102639,-64.899345450667,34.185551966526));
#32515=CARTESIAN_POINT('Ctrl Pts',(19.9405059563517,-63.8785413671765,34.0744188485344));
#32516=CARTESIAN_POINT('Ctrl Pts',(21.7500391877175,-64.7993796508576,33.9632857305429));
#32517=CARTESIAN_POINT('Ctrl Pts',(21.9578676761867,-66.8190729708356,33.8521526125513));
#32518=CARTESIAN_POINT('Ctrl Pts',(20.3737786051983,-68.089118451048,33.7410194945598));
#32519=CARTESIAN_POINT('Ctrl Pts',(18.4475926435972,-67.447120507218,33.6298863765682));
#32520=CARTESIAN_POINT('Ctrl Pts',(17.9422309964094,-65.480660912431,33.5187532585767));
#32521=CARTESIAN_POINT('Ctrl Pts',(19.3202205344693,-63.989520893903,33.407620140585));
#32522=CARTESIAN_POINT('Ctrl Pts',(21.3203709951603,-64.3384504837937,33.2964870225936));
#32523=CARTESIAN_POINT('Ctrl Pts',(22.1120659518255,-66.2080955894538,33.1853539046019));
#32524=CARTESIAN_POINT('Ctrl Pts',(20.9707150192538,-67.8872834207894,33.0742207866104));
#32525=CARTESIAN_POINT('Ctrl Pts',(18.9409274941004,-67.8391551828144,32.9630876686188));
#32526=CARTESIAN_POINT('Ctrl Pts',(17.8804448110288,-66.1077597330111,32.8519545506273));
#32527=CARTESIAN_POINT('Ctrl Pts',(18.7598624617856,-64.2777383342113,32.7408214326357));
#32528=CARTESIAN_POINT('Ctrl Pts',(20.7743027988527,-64.0239985994815,32.6296883146442));
#32529=CARTESIAN_POINT('Ctrl Pts',(22.0800707381493,-65.5787731211726,32.5185551966526));
#32530=CARTESIAN_POINT('Ctrl Pts',(21.4820760671049,-67.5190710616904,32.4074220786611));
#32531=CARTESIAN_POINT('Ctrl Pts',(19.5276270455007,-68.069055376497,32.2962889606695));
#32532=CARTESIAN_POINT('Ctrl Pts',(18.0055123442725,-66.7253587735064,32.1851558426779));
#32533=CARTESIAN_POINT('Ctrl Pts',(18.3088312478353,-64.7177852711602,32.0740227246864));
#32534=CARTESIAN_POINT('Ctrl Pts',(20.1599743571327,-63.8837451561277,31.9628896066947));
#32535=CARTESIAN_POINT('Ctrl Pts',(21.8647026382529,-64.9865847691865,31.8517564887033));
#32536=CARTESIAN_POINT('Ctrl Pts',(21.8627816708634,-67.0169418891202,31.7406233707116));
#32537=CARTESIAN_POINT('Ctrl Pts',(20.1559695999277,-68.1165537656887,31.6294902527202));
#32538=CARTESIAN_POINT('Ctrl Pts',(18.3064080122344,-67.2790123291542,31.5183571347285));
#32539=CARTESIAN_POINT('Ctrl Pts',(18.0068884708754,-65.2708684675433,31.407224016737));
#32540=CARTESIAN_POINT('Ctrl Pts',(19.5315430490765,-63.930054482774,31.2960908987454));
#32541=CARTESIAN_POINT('Ctrl Pts',(21.4849478670487,-64.4837361076318,31.1849577807539));
#32542=CARTESIAN_POINT('Ctrl Pts',(22.0792699501195,-66.4251621263501,31.0738246627623));
#32543=CARTESIAN_POINT('Ctrl Pts',(20.7705623355731,-67.9774630328147,30.9626915447708));
#32544=CARTESIAN_POINT('Ctrl Pts',(18.7566057424723,-67.7199119394606,30.8515584267792));
#32545=CARTESIAN_POINT('Ctrl Pts',(17.8806525133819,-65.8882297440381,30.7404253087877));
#32546=CARTESIAN_POINT('Ctrl Pts',(18.9444095207486,-64.1588440861061,30.6292921907961));
#32547=CARTESIAN_POINT('Ctrl Pts',(20.9742844823626,-64.1145567877606,30.5181590728046));
#32548=CARTESIAN_POINT('Ctrl Pts',(22.1124559382548,-65.7959013275781,30.4070259548129));
#32549=CARTESIAN_POINT('Ctrl Pts',(21.3172245740007,-67.6640450056417,30.2958928368214));
#32550=CARTESIAN_POINT('Ctrl Pts',(19.3164174341671,-68.0091891983687,30.1847597188298));
#32551=CARTESIAN_POINT('Ctrl Pts',(17.9412519641314,-66.5154443558325,30.0736266008383));
#32552=CARTESIAN_POINT('Ctrl Pts',(18.4503337280557,-64.5499445511462,29.9624934828467));
#32553=CARTESIAN_POINT('Ctrl Pts',(20.3777310583335,-63.9115925668773,29.8513603648552));
#32554=CARTESIAN_POINT('Ctrl Pts',(21.9594140566749,-65.1846332643177,29.7402272468636));
#32555=CARTESIAN_POINT('Ctrl Pts',(21.7477641885617,-67.2039296907767,29.6290941288721));
#32556=CARTESIAN_POINT('Ctrl Pts',(19.9364917437487,-68.1213422780259,29.5179610108805));
#32557=CARTESIAN_POINT('Ctrl Pts',(18.1833445547175,-67.0972189172074,29.4068278928889));
#32558=CARTESIAN_POINT('Ctrl Pts',(18.0928719320704,-65.0688776172449,29.2956947748974));
#32559=CARTESIAN_POINT('Ctrl Pts',(19.7478779810218,-63.8927361705997,29.1845616569058));
#32560=CARTESIAN_POINT('Ctrl Pts',(21.6336360251679,-64.6452455217178,29.0734285389143));
#32561=CARTESIAN_POINT('Ctrl Pts',(22.0242260797931,-66.6376794939764,28.9622954209227));
#32562=CARTESIAN_POINT('Ctrl Pts',(20.5621647534294,-68.0464840945274,28.8511623029311));
#32563=CARTESIAN_POINT('Ctrl Pts',(18.5855881181383,-67.5822659029381,28.7400291849396));
#32564=CARTESIAN_POINT('Ctrl Pts',(17.9035369078357,-65.6698956796004,28.628896066948));
#32565=CARTESIAN_POINT('Ctrl Pts',(19.1402512354662,-64.0596499230725,28.5177629489565));
#32566=CARTESIAN_POINT('Ctrl Pts',(21.1638414717776,-64.2252889283823,28.4066298309649));
#32567=CARTESIAN_POINT('Ctrl Pts',(22.1222381847684,-66.0152133583859,28.2954967129734));
#32568=CARTESIAN_POINT('Ctrl Pts',(21.1382789805698,-67.7912139239986,28.1843635949818));
#32569=CARTESIAN_POINT('Ctrl Pts',(19.1125220511464,-67.927825004883,28.0732304769903));
#32570=CARTESIAN_POINT('Ctrl Pts',(17.8990198712721,-66.3000147628294,27.9620973589986));
#32571=CARTESIAN_POINT('Ctrl Pts',(18.6084173990482,-64.3976192014007,27.8509642410071));
#32572=CARTESIAN_POINT('Ctrl Pts',(20.5914460952399,-63.9617856158794,27.7398311230156));
#32573=CARTESIAN_POINT('Ctrl Pts',(22.0331600462417,-65.3914060581699,27.628698005024));
#32574=CARTESIAN_POINT('Ctrl Pts',(21.6140458979948,-67.3780356297918,27.5175648870324));
#32575=CARTESIAN_POINT('Ctrl Pts',(19.7176934167296,-68.1034327545841,27.4064317690409));
#32576=CARTESIAN_POINT('Ctrl Pts',(18.0797190298508,-66.9036854310583,27.2952986510493));
#32577=CARTESIAN_POINT('Ctrl Pts',(18.1992613725651,-64.8768496343423,27.1841655330578));
#32578=CARTESIAN_POINT('Ctrl Pts',(19.966910575135,-63.8779652550036,27.0730324150662));
#32579=CARTESIAN_POINT('Ctrl Pts',(21.7648445383867,-64.8212506048152,26.9618992970747));
#32580=CARTESIAN_POINT('Ctrl Pts',(21.9475232832876,-66.8433737801612,26.8507661790831));
#32581=CARTESIAN_POINT('Ctrl Pts',(20.3477521317823,-68.0936081090632,26.7396330610915));
#32582=CARTESIAN_POINT('Ctrl Pts',(18.4297044098267,-67.4276898290772,26.6284999431));
#32583=CARTESIAN_POINT('Ctrl Pts',(17.9488532815309,-65.4550937515292,26.5173668251084));
#32584=CARTESIAN_POINT('Ctrl Pts',(19.3452918373275,-63.981217065991,26.4062337071169));
#32585=CARTESIAN_POINT('Ctrl Pts',(21.3409461194645,-64.355010486417,26.2951005891253));
#32586=CARTESIAN_POINT('Ctrl Pts',(22.1093116467166,-66.2343620464388,26.1839674711338));
#32587=CARTESIAN_POINT('Ctrl Pts',(20.947156294938,-67.8992182497961,26.0728343531421));
#32588=CARTESIAN_POINT('Ctrl Pts',(18.9181179241837,-67.8258311454213,25.9617012351507));
#32589=CARTESIAN_POINT('Ctrl Pts',(17.8792771574272,-66.0813795143389,25.850568117159));
#32590=CARTESIAN_POINT('Ctrl Pts',(18.7813724162924,-64.2624301942028,25.7394349991675));
#32591=CARTESIAN_POINT('Ctrl Pts',(20.798869385088,-64.0338049621852,25.6283018811759));
#32592=CARTESIAN_POINT('Ctrl Pts',(22.0850784884117,-65.6046553876296,25.5171687631844));
#32593=CARTESIAN_POINT('Ctrl Pts',(21.4632032199543,-67.5374672364217,25.4060356451928));
#32594=CARTESIAN_POINT('Ctrl Pts',(19.5016252399817,-68.0628763782035,25.2949025272013));
#32595=CARTESIAN_POINT('Ctrl Pts',(17.9972202285682,-66.7007627032078,25.1837694092097));
#32596=CARTESIAN_POINT('Ctrl Pts',(18.3237513831539,-64.6962806412445,25.0726362912182));
#32597=CARTESIAN_POINT('Ctrl Pts',(20.1887505583808,-63.8870193351586,24.9615031732266));
#32598=CARTESIAN_POINT('Ctrl Pts',(21.3096484764695,-64.6342008454597,24.8874144278989));
#32599=CARTESIAN_POINT('Ctrl Pts',(21.5881947811615,-65.162290716277,24.850370055235));
#32600=CARTESIAN_POINT('Ctrl Pts',(21.4664903694652,-64.752733913429,36.149629944765));
#32601=CARTESIAN_POINT('Ctrl Pts',(21.8812182065951,-65.2403559097683,36.1125855721011));
#32602=CARTESIAN_POINT('Ctrl Pts',(22.1785129256187,-66.6537504941968,36.0384968267734));
#32603=CARTESIAN_POINT('Ctrl Pts',(20.6300843339218,-68.1878880863455,35.9273637087819));
#32604=CARTESIAN_POINT('Ctrl Pts',(18.5046939287577,-67.7145058921161,35.8162305907903));
#32605=CARTESIAN_POINT('Ctrl Pts',(17.748033519272,-65.674417027399,35.7050974727988));
#32606=CARTESIAN_POINT('Ctrl Pts',(19.0523754862353,-63.9310782053294,35.5939643548071));
#32607=CARTESIAN_POINT('Ctrl Pts',(21.2240639963219,-64.0819176403945,35.4828312368157));
#32608=CARTESIAN_POINT('Ctrl Pts',(22.2754192341118,-65.9879508350117,35.371698118824));
#32609=CARTESIAN_POINT('Ctrl Pts',(21.2442321254897,-67.9051677269406,35.2605650008325));
#32610=CARTESIAN_POINT('Ctrl Pts',(19.0742693382642,-68.0786219771207,35.1494318828409));
#32611=CARTESIAN_POINT('Ctrl Pts',(17.7515744298424,-66.3496787750931,35.0382987648494));
#32612=CARTESIAN_POINT('Ctrl Pts',(18.4867257258214,-64.3006761375172,34.9271656468578));
#32613=CARTESIAN_POINT('Ctrl Pts',(20.6068858888105,-63.8069714423194,34.8160325288663));
#32614=CARTESIAN_POINT('Ctrl Pts',(22.1715998538182,-65.3204078554697,34.7048994108747));
#32615=CARTESIAN_POINT('Ctrl Pts',(21.7487803326752,-67.4558362275328,34.5937662928832));
#32616=CARTESIAN_POINT('Ctrl Pts',(19.7254081327793,-68.2588247393393,34.4826331748916));
#32617=CARTESIAN_POINT('Ctrl Pts',(17.9533532612099,-66.9944485669578,34.3715000569001));
#32618=CARTESIAN_POINT('Ctrl Pts',(18.0544700183374,-64.8199136121645,34.2603669389084));
#32619=CARTESIAN_POINT('Ctrl Pts',(19.936212400967,-63.7254403241524,34.1492338209169));
#32620=CARTESIAN_POINT('Ctrl Pts',(21.876335699385,-64.7127334985896,34.0381007029253));
#32621=CARTESIAN_POINT('Ctrl Pts',(22.0991627166318,-66.878183680895,33.9269675849338));
#32622=CARTESIAN_POINT('Ctrl Pts',(20.4007533919938,-68.2398855736812,33.8158344669422));
#32623=CARTESIAN_POINT('Ctrl Pts',(18.3355587901974,-67.5515560383232,33.7047013489507));
#32624=CARTESIAN_POINT('Ctrl Pts',(17.7937262950319,-65.443181343063,33.5935682309591));
#32625=CARTESIAN_POINT('Ctrl Pts',(19.2711623329145,-63.844429001297,33.4824351129676));
#32626=CARTESIAN_POINT('Ctrl Pts',(21.4156592903974,-64.2185400787396,33.371301994976));
#32627=CARTESIAN_POINT('Ctrl Pts',(22.2644891455457,-66.2231133943269,33.2601688769845));
#32628=CARTESIAN_POINT('Ctrl Pts',(21.0407694052443,-68.0234845494536,33.1490357589929));
#32629=CARTESIAN_POINT('Ctrl Pts',(18.8644965409898,-67.9718830015026,33.0379026410013));
#32630=CARTESIAN_POINT('Ctrl Pts',(17.7274811353965,-66.1155365179385,32.9267695230098));
#32631=CARTESIAN_POINT('Ctrl Pts',(18.670364440162,-64.1534464657238,32.8156364050182));
#32632=CARTESIAN_POINT('Ctrl Pts',(20.8301825432355,-63.8813948876976,32.7045032870266));
#32633=CARTESIAN_POINT('Ctrl Pts',(22.230184907074,-65.5483740959451,32.5933701690351));
#32634=CARTESIAN_POINT('Ctrl Pts',(21.5890342647356,-67.6286991074011,32.4822370510435));
#32635=CARTESIAN_POINT('Ctrl Pts',(19.493536919532,-68.2183745907937,32.371103933052));
#32636=CARTESIAN_POINT('Ctrl Pts',(17.8615745197653,-66.7777063343178,32.2599708150604));
#32637=CARTESIAN_POINT('Ctrl Pts',(18.1867832871161,-64.6252506304517,32.1488376970689));
#32638=CARTESIAN_POINT('Ctrl Pts',(20.1715193576126,-63.7310196592038,32.0377045790772));
#32639=CARTESIAN_POINT('Ctrl Pts',(21.9992741610859,-64.9134488020487,31.9265714610858));
#32640=CARTESIAN_POINT('Ctrl Pts',(21.9972145616692,-67.090332367497,31.8154383430941));
#32641=CARTESIAN_POINT('Ctrl Pts',(20.1672255858137,-68.2693008351482,31.7043052251026));
#32642=CARTESIAN_POINT('Ctrl Pts',(18.1841851718866,-67.3713158596613,31.593172107111));
#32643=CARTESIAN_POINT('Ctrl Pts',(17.863049958424,-65.218248634946,31.4820389891195));
#32644=CARTESIAN_POINT('Ctrl Pts',(19.4977355325458,-63.7806710289621,31.3709058711279));
#32645=CARTESIAN_POINT('Ctrl Pts',(21.5921133162185,-64.3743106492091,31.2597727531364));
#32646=CARTESIAN_POINT('Ctrl Pts',(22.2293263279185,-66.4558451498092,31.1486396351448));
#32647=CARTESIAN_POINT('Ctrl Pts',(20.8261721388783,-68.1201722274138,31.0375065171533));
#32648=CARTESIAN_POINT('Ctrl Pts',(18.6668726905181,-67.8440342333234,30.9263733991617));
#32649=CARTESIAN_POINT('Ctrl Pts',(17.7277038271754,-65.8801635284154,30.8152402811702));
#32650=CARTESIAN_POINT('Ctrl Pts',(18.8682298579076,-64.0259718790191,30.7041071631786));
#32651=CARTESIAN_POINT('Ctrl Pts',(21.0445964687214,-63.9784884629342,30.592974045187));
#32652=CARTESIAN_POINT('Ctrl Pts',(22.2649072764451,-65.7811719714907,30.4818409271955));
#32653=CARTESIAN_POINT('Ctrl Pts',(21.4122857988845,-67.7841355047261,30.3707078092039));
#32654=CARTESIAN_POINT('Ctrl Pts',(19.2670847711574,-68.154188001147,30.2595746912124));
#32655=CARTESIAN_POINT('Ctrl Pts',(17.7926766081294,-66.5526428509046,30.1484415732208));
#32656=CARTESIAN_POINT('Ctrl Pts',(18.3384976927434,-64.4452972117037,30.0373084552292));
#32657=CARTESIAN_POINT('Ctrl Pts',(20.4049910850522,-63.760876756857,29.9261753372377));
#32658=CARTESIAN_POINT('Ctrl Pts',(22.1008206960275,-65.1257900251668,29.8150422192461));
#32659=CARTESIAN_POINT('Ctrl Pts',(21.8738965185015,-67.2908146710133,29.7039091012545));
#32660=CARTESIAN_POINT('Ctrl Pts',(19.9319084913948,-68.2744349239781,29.592775983263));
#32661=CARTESIAN_POINT('Ctrl Pts',(18.0522404930191,-67.1764028136319,29.4816428652714));
#32662=CARTESIAN_POINT('Ctrl Pts',(17.9552386584996,-65.0016805454862,29.3705097472799));
#32663=CARTESIAN_POINT('Ctrl Pts',(19.7296828847433,-63.7406595355825,29.2593766292883));
#32664=CARTESIAN_POINT('Ctrl Pts',(21.7515319744479,-64.5474758454877,29.1482435112967));
#32665=CARTESIAN_POINT('Ctrl Pts',(22.1703100615111,-66.6836994323963,29.0371103933052));
#32666=CARTESIAN_POINT('Ctrl Pts',(20.6027349577076,-68.1941743886282,28.9259772753136));
#32667=CARTESIAN_POINT('Ctrl Pts',(18.4835130971936,-67.6964545825255,28.8148441573221));
#32668=CARTESIAN_POINT('Ctrl Pts',(17.7522397384703,-65.6460727706933,28.7037110393305));
#32669=CARTESIAN_POINT('Ctrl Pts',(19.0782050420819,-63.9196190895633,28.592577921339));
#32670=CARTESIAN_POINT('Ctrl Pts',(21.2478333726739,-64.0972119006585,28.4814448033474));
#32671=CARTESIAN_POINT('Ctrl Pts',(22.2753954863563,-66.0163112732831,28.3703116853558));
#32672=CARTESIAN_POINT('Ctrl Pts',(21.2204260922228,-67.9204819265891,28.2591785673643));
#32673=CARTESIAN_POINT('Ctrl Pts',(19.048474703002,-68.0669519312575,28.1480454493727));
#32674=CARTESIAN_POINT('Ctrl Pts',(17.7473967172287,-66.3216661739864,28.0369123313812));
#32675=CARTESIAN_POINT('Ctrl Pts',(18.5079899175204,-64.2819788736603,27.9257792133896));
#32676=CARTESIAN_POINT('Ctrl Pts',(20.6341294700995,-63.8146921287439,27.8146460953981));
#32677=CARTESIAN_POINT('Ctrl Pts',(22.179888772835,-65.3474851606182,27.7035129774065));
#32678=CARTESIAN_POINT('Ctrl Pts',(21.7305280705192,-67.4774854559544,27.5923798594149));
#32679=CARTESIAN_POINT('Ctrl Pts',(19.6973199662731,-68.2552329092867,27.4812467414234));
#32680=CARTESIAN_POINT('Ctrl Pts',(17.9411365400108,-66.968902437848,27.3701136234318));
#32681=CARTESIAN_POINT('Ctrl Pts',(18.0693059928992,-64.7957943218349,27.2589805054402));
#32682=CARTESIAN_POINT('Ctrl Pts',(19.9645225835043,-63.7248226352203,27.1478473874487));
#32683=CARTESIAN_POINT('Ctrl Pts',(21.8922095199243,-64.736182831598,27.0367142694572));
#32684=CARTESIAN_POINT('Ctrl Pts',(22.0880717914564,-66.904238226634,26.9255811514656));
#32685=CARTESIAN_POINT('Ctrl Pts',(20.3728486447502,-68.2446992405243,26.814448033474));
#32686=CARTESIAN_POINT('Ctrl Pts',(18.3163796016065,-67.5307230905157,26.7033149154825));
#32687=CARTESIAN_POINT('Ctrl Pts',(17.8008264960285,-65.4157690559163,26.5921817974909));
#32688=CARTESIAN_POINT('Ctrl Pts',(19.2980429770242,-63.8355259042336,26.4810486794994));
#32689=CARTESIAN_POINT('Ctrl Pts',(21.4377192765522,-64.2362951806379,26.3699155615078));
#32690=CARTESIAN_POINT('Ctrl Pts',(22.2615360682436,-66.2512754442303,26.2587824435162));
#32691=CARTESIAN_POINT('Ctrl Pts',(21.0155104991719,-68.0362806890421,26.1476493255246));
#32692=CARTESIAN_POINT('Ctrl Pts',(18.8400408541557,-67.9575973973882,26.0365162075331));
#32693=CARTESIAN_POINT('Ctrl Pts',(17.7262292147809,-66.0872524964152,25.9253830895415));
#32694=CARTESIAN_POINT('Ctrl Pts',(18.6934267211763,-64.1370335706351,25.81424997155));
#32695=CARTESIAN_POINT('Ctrl Pts',(20.8565220464243,-63.8919089542118,25.7031168535584));
#32696=CARTESIAN_POINT('Ctrl Pts',(22.235554055752,-65.576124229128,25.5919837355669));
#32697=CARTESIAN_POINT('Ctrl Pts',(21.5687994053643,-67.6484228939442,25.4808506175753));
#32698=CARTESIAN_POINT('Ctrl Pts',(19.4656586204139,-68.2117496676687,25.3697174995837));
#32699=CARTESIAN_POINT('Ctrl Pts',(17.8526839801542,-66.7513352192652,25.2585843815922));
#32700=CARTESIAN_POINT('Ctrl Pts',(18.2027801760626,-64.6021940582926,25.1474512636006));
#32701=CARTESIAN_POINT('Ctrl Pts',(20.2023722745493,-63.7345301285949,25.0363181456091));
#32702=CARTESIAN_POINT('Ctrl Pts',(21.4041629509165,-64.5356340990305,24.9622294002814));
#32703=CARTESIAN_POINT('Ctrl Pts',(21.7028113349605,-65.1018350641589,24.9251850276175));
#32704=CARTESIAN_POINT('Ctrl Pts',(21.5652001142717,-64.6687801966678,36.2244449171475));
#32705=CARTESIAN_POINT('Ctrl Pts',(22.0078433607487,-65.1892241220309,36.1874005444836));
#32706=CARTESIAN_POINT('Ctrl Pts',(22.325149043675,-66.6977545639082,36.1133117991559));
#32707=CARTESIAN_POINT('Ctrl Pts',(20.6724954298983,-68.3351552482478,36.0021786811644));
#32708=CARTESIAN_POINT('Ctrl Pts',(18.4040445936014,-67.8299096087744,35.8910455631728));
#32709=CARTESIAN_POINT('Ctrl Pts',(17.5964532284949,-65.6525019757846,35.7799124451812));
#32710=CARTESIAN_POINT('Ctrl Pts',(18.9885907005499,-63.7918186870749,35.6687793271897));
#32711=CARTESIAN_POINT('Ctrl Pts',(21.3064559759895,-63.9528111531126,35.5576462091981));
#32712=CARTESIAN_POINT('Ctrl Pts',(22.4285781341657,-65.9871398034319,35.4465130912066));
#32713=CARTESIAN_POINT('Ctrl Pts',(21.3279816257553,-68.0334049278494,35.335379973215));
#32714=CARTESIAN_POINT('Ctrl Pts',(19.0119582319098,-68.2185344164948,35.2242468552235));
#32715=CARTESIAN_POINT('Ctrl Pts',(17.6002324784272,-66.3732157197415,35.1131137372319));
#32716=CARTESIAN_POINT('Ctrl Pts',(18.3848669475188,-64.186294326152,35.0019806192404));
#32717=CARTESIAN_POINT('Ctrl Pts',(20.6477354930483,-63.6593582743169,34.8908475012487));
#32718=CARTESIAN_POINT('Ctrl Pts',(22.317770651701,-65.2746643793748,34.7797143832572));
#32719=CARTESIAN_POINT('Ctrl Pts',(21.8664910684258,-67.5538288400258,34.6685812652657));
#32720=CARTESIAN_POINT('Ctrl Pts',(19.7069253021358,-68.4108666608038,34.5574481472741));
#32721=CARTESIAN_POINT('Ctrl Pts',(17.81559308119,-67.0613850885411,34.4463150292825));
#32722=CARTESIAN_POINT('Ctrl Pts',(17.923516026411,-64.740481773662,34.335181911291));
#32723=CARTESIAN_POINT('Ctrl Pts',(19.9319188455824,-63.5723392811283,34.2240487932994));
#32724=CARTESIAN_POINT('Ctrl Pts',(22.0026322110525,-64.6260873463218,34.1129156753078));
#32725=CARTESIAN_POINT('Ctrl Pts',(22.2404577570769,-66.9372943909543,34.0017825573163));
#32726=CARTESIAN_POINT('Ctrl Pts',(20.4277281787894,-68.3906526963146,33.8906494393247));
#32727=CARTESIAN_POINT('Ctrl Pts',(18.2235249367975,-67.6559915694283,33.7795163213332));
#32728=CARTESIAN_POINT('Ctrl Pts',(17.6452215936543,-65.4057017736952,33.6683832033416));
#32729=CARTESIAN_POINT('Ctrl Pts',(19.2221041313598,-63.699337108691,33.55725008535));
#32730=CARTESIAN_POINT('Ctrl Pts',(21.5109475856345,-64.0986296736855,33.4461169673585));
#32731=CARTESIAN_POINT('Ctrl Pts',(22.4169123392658,-66.2381311992,33.3349838493669));
#32732=CARTESIAN_POINT('Ctrl Pts',(21.110823791235,-68.1596856781178,33.2238507313754));
#32733=CARTESIAN_POINT('Ctrl Pts',(18.7880655878792,-68.1046108201909,33.1127176133838));
#32734=CARTESIAN_POINT('Ctrl Pts',(17.5745174597642,-66.123313302866,33.0015844953923));
#32735=CARTESIAN_POINT('Ctrl Pts',(18.5808664185384,-64.0291545972363,32.8904513774007));
#32736=CARTESIAN_POINT('Ctrl Pts',(20.8860622876183,-63.7387911759138,32.7793182594092));
#32737=CARTESIAN_POINT('Ctrl Pts',(22.3802990759988,-65.5179750707177,32.6681851414176));
#32738=CARTESIAN_POINT('Ctrl Pts',(21.6959924623663,-67.7383271531118,32.5570520234261));
#32739=CARTESIAN_POINT('Ctrl Pts',(19.4594467935634,-68.3676938050906,32.4459189054344));
#32740=CARTESIAN_POINT('Ctrl Pts',(17.7176366952581,-66.8300538951291,32.3347857874429));
#32741=CARTESIAN_POINT('Ctrl Pts',(18.0647353263969,-64.5327159897432,32.2236526694514));
#32742=CARTESIAN_POINT('Ctrl Pts',(20.1830643580926,-63.5782941622798,32.1125195514598));
#32743=CARTESIAN_POINT('Ctrl Pts',(22.1338456839189,-64.8403128349112,32.0013864334682));
#32744=CARTESIAN_POINT('Ctrl Pts',(22.131647452475,-67.1637228458735,31.8902533154766));
#32745=CARTESIAN_POINT('Ctrl Pts',(20.1784815716998,-68.4220479046079,31.7791201974851));
#32746=CARTESIAN_POINT('Ctrl Pts',(18.0619623315387,-67.4636193901682,31.6679870794935));
#32747=CARTESIAN_POINT('Ctrl Pts',(17.7192114459727,-65.165628802349,31.556853961502));
#32748=CARTESIAN_POINT('Ctrl Pts',(19.4639280160152,-63.6312875751501,31.4457208435104));
#32749=CARTESIAN_POINT('Ctrl Pts',(21.6992787653883,-64.2648851907865,31.3345877255189));
#32750=CARTESIAN_POINT('Ctrl Pts',(22.3793827057175,-66.4865281732684,31.2234546075273));
#32751=CARTESIAN_POINT('Ctrl Pts',(20.8817819421834,-68.2628814220129,31.1123214895357));
#32752=CARTESIAN_POINT('Ctrl Pts',(18.577139638564,-67.9681565271862,31.0011883715442));
#32753=CARTESIAN_POINT('Ctrl Pts',(17.5747551409689,-65.8720973127928,30.8900552535526));
#32754=CARTESIAN_POINT('Ctrl Pts',(18.7920501950665,-63.8930996719321,30.7789221355611));
#32755=CARTESIAN_POINT('Ctrl Pts',(21.1149084550803,-63.8424201381079,30.6677890175695));
#32756=CARTESIAN_POINT('Ctrl Pts',(22.4173586146354,-65.7664426154033,30.556655899578));
#32757=CARTESIAN_POINT('Ctrl Pts',(21.5073470237683,-67.9042260038106,30.4455227815864));
#32758=CARTESIAN_POINT('Ctrl Pts',(19.2177521081477,-68.2991868039253,30.3343896635948));
#32759=CARTESIAN_POINT('Ctrl Pts',(17.6441012521274,-66.5898413459768,30.2232565456033));
#32760=CARTESIAN_POINT('Ctrl Pts',(18.2266616574312,-64.3406498722612,30.1121234276117));
#32761=CARTESIAN_POINT('Ctrl Pts',(20.432251111771,-63.6101609468367,30.0009903096202));
#32762=CARTESIAN_POINT('Ctrl Pts',(22.24222733538,-65.0669467860159,29.8898571916286));
#32763=CARTESIAN_POINT('Ctrl Pts',(22.0000288484413,-67.3776996512498,29.7787240736371));
#32764=CARTESIAN_POINT('Ctrl Pts',(19.9273252390408,-68.4275275699302,29.6675909556455));
#32765=CARTESIAN_POINT('Ctrl Pts',(17.9211364313208,-67.2555867100563,29.5564578376539));
#32766=CARTESIAN_POINT('Ctrl Pts',(17.8176053849288,-64.9344834737275,29.4453247196624));
#32767=CARTESIAN_POINT('Ctrl Pts',(19.7114877884649,-63.5885829005652,29.3341916016708));
#32768=CARTESIAN_POINT('Ctrl Pts',(21.869427923728,-64.4497061692577,29.2230584836792));
#32769=CARTESIAN_POINT('Ctrl Pts',(22.3163940432292,-66.7297193708161,29.1119253656877));
#32770=CARTESIAN_POINT('Ctrl Pts',(20.6433051619858,-68.3418646827291,29.0007922476961));
#32771=CARTESIAN_POINT('Ctrl Pts',(18.3814380762489,-67.8106432621128,28.8896591297046));
#32772=CARTESIAN_POINT('Ctrl Pts',(17.6009425691049,-65.6222498617862,28.778526011713));
#32773=CARTESIAN_POINT('Ctrl Pts',(19.0161588486977,-63.7795882560541,28.6673928937214));
#32774=CARTESIAN_POINT('Ctrl Pts',(21.3318252735703,-63.9691348729347,28.5562597757299));
#32775=CARTESIAN_POINT('Ctrl Pts',(22.4285527879442,-66.0174091881803,28.4451266577383));
#32776=CARTESIAN_POINT('Ctrl Pts',(21.3025732038757,-68.0497499291796,28.3339935397468));
#32777=CARTESIAN_POINT('Ctrl Pts',(18.9844273548577,-68.2060788576321,28.2228604217552));
#32778=CARTESIAN_POINT('Ctrl Pts',(17.5957735631854,-66.3433175851434,28.1117273037636));
#32779=CARTESIAN_POINT('Ctrl Pts',(18.4075624359926,-64.16633854592,28.0005941857721));
#32780=CARTESIAN_POINT('Ctrl Pts',(20.676812844959,-63.6675986416085,27.8894610677805));
#32781=CARTESIAN_POINT('Ctrl Pts',(22.3266174994283,-65.3035642630666,27.778327949789));
#32782=CARTESIAN_POINT('Ctrl Pts',(21.8470102430435,-67.576935282117,27.6671948317974));
#32783=CARTESIAN_POINT('Ctrl Pts',(19.6769465158166,-68.4070330639894,27.5560617138059));
#32784=CARTESIAN_POINT('Ctrl Pts',(17.8025540501709,-67.0341194446376,27.4449285958143));
#32785=CARTESIAN_POINT('Ctrl Pts',(17.9393506132333,-64.7147390093274,27.3337954778228));
#32786=CARTESIAN_POINT('Ctrl Pts',(19.9621345918737,-63.5716800154371,27.2226623598312));
#32787=CARTESIAN_POINT('Ctrl Pts',(22.0195745014619,-64.6511150583807,27.1115292418397));
#32788=CARTESIAN_POINT('Ctrl Pts',(22.2286202996251,-66.9651026731069,27.000396123848));
#32789=CARTESIAN_POINT('Ctrl Pts',(20.3979451577182,-68.3957903719854,26.8892630058565));
#32790=CARTESIAN_POINT('Ctrl Pts',(18.2030547933863,-67.6337563519543,26.7781298878649));
#32791=CARTESIAN_POINT('Ctrl Pts',(17.6527997105261,-65.3764443603032,26.6669967698734));
#32792=CARTESIAN_POINT('Ctrl Pts',(19.2507941167209,-63.6898347424764,26.5558636518818));
#32793=CARTESIAN_POINT('Ctrl Pts',(21.5344924336398,-64.1175798748589,26.4447305338903));
#32794=CARTESIAN_POINT('Ctrl Pts',(22.4137604897707,-66.2681888420218,26.3335974158987));
#32795=CARTESIAN_POINT('Ctrl Pts',(21.0838647034058,-68.1733431282881,26.2224642979072));
#32796=CARTESIAN_POINT('Ctrl Pts',(18.7619637841276,-68.0893636493551,26.1113311799156));
#32797=CARTESIAN_POINT('Ctrl Pts',(17.5731812721346,-66.0931254784914,26.000198061924));
#32798=CARTESIAN_POINT('Ctrl Pts',(18.6054810260603,-64.0116369470673,25.8890649439325));
#32799=CARTESIAN_POINT('Ctrl Pts',(20.9141747077605,-63.7500129462385,25.7779318259409));
#32800=CARTESIAN_POINT('Ctrl Pts',(22.3860296230922,-65.5475930706263,25.6667987079494));
#32801=CARTESIAN_POINT('Ctrl Pts',(21.6743955907743,-67.7593785514666,25.5556655899578));
#32802=CARTESIAN_POINT('Ctrl Pts',(19.429692000846,-68.3606229571339,25.4445324719662));
#32803=CARTESIAN_POINT('Ctrl Pts',(17.7081477317402,-66.8019077353226,25.3333993539747));
#32804=CARTESIAN_POINT('Ctrl Pts',(18.0818089689714,-64.5081074753406,25.2222662359831));
#32805=CARTESIAN_POINT('Ctrl Pts',(20.2159939907177,-63.5820409220313,25.1111331179916));
#32806=CARTESIAN_POINT('Ctrl Pts',(21.4986774253636,-64.4370673526013,25.0370443726639));
#32807=CARTESIAN_POINT('Ctrl Pts',(21.8174278887595,-65.0413794120408,25.));
#32808=CARTESIAN_POINT('Ctrl Pts',(21.2690708798524,-64.9206413469514,36.));
#32809=CARTESIAN_POINT('Ctrl Pts',(21.3144000906036,-64.9629286896491,36.));
#32810=CARTESIAN_POINT('Ctrl Pts',(21.3569992965038,-65.00778514716,36.));
#32811=CARTESIAN_POINT('Ctrl Pts',(21.3968699769242,-65.0548656952241,36.));
#32812=CARTESIAN_POINT('Ctrl Pts',(21.4393722521919,-65.1050537128971,36.));
#32813=CARTESIAN_POINT('Ctrl Pts',(21.4787746568644,-65.1577693380806,36.));
#32814=CARTESIAN_POINT('Ctrl Pts',(21.5150501504783,-65.2126493353753,36.));
#32815=CARTESIAN_POINT('Ctrl Pts',(21.5467912073906,-65.2606693330081,36.));
#32816=CARTESIAN_POINT('Ctrl Pts',(21.576137979607,-65.3103476536427,36.));
#32817=CARTESIAN_POINT('Ctrl Pts',(21.6030494591265,-65.3614685121224,36.));
#32818=CARTESIAN_POINT('Ctrl Pts',(21.6165497288404,-65.3871135301522,36.));
#32819=CARTESIAN_POINT('Ctrl Pts',(21.6294367784251,-65.4131219292723,36.));
#32820=CARTESIAN_POINT('Ctrl Pts',(21.6417030895028,-65.4394683087242,36.));
#32821=CARTESIAN_POINT('Ctrl Pts',(21.6473120464069,-65.4515155905833,36.));
#32822=CARTESIAN_POINT('Ctrl Pts',(21.6527917902974,-65.4636352254459,36.));
#32823=CARTESIAN_POINT('Ctrl Pts',(21.6581330897624,-65.4758048257742,36.));
#32824=CARTESIAN_POINT('Ctrl Pts',(21.6850520365028,-65.5371368715128,36.));
#32825=CARTESIAN_POINT('Ctrl Pts',(21.7085098197287,-65.5998443796051,36.));
#32826=CARTESIAN_POINT('Ctrl Pts',(21.7284829341248,-65.6635695831573,36.));
#32827=CARTESIAN_POINT('Ctrl Pts',(21.748810363471,-65.728425245979,36.));
#32828=CARTESIAN_POINT('Ctrl Pts',(21.7655289516023,-65.794335872963,36.));
#32829=CARTESIAN_POINT('Ctrl Pts',(21.7785746037815,-65.8609608298779,36.));
#32830=CARTESIAN_POINT('Ctrl Pts',(21.7894858424902,-65.9166852044715,36.));
#32831=CARTESIAN_POINT('Ctrl Pts',(21.7978271370784,-65.9729102271441,36.));
#32832=CARTESIAN_POINT('Ctrl Pts',(21.8035361618645,-66.0294488809297,36.));
#32833=CARTESIAN_POINT('Ctrl Pts',(21.8061657868978,-66.0554910623717,36.));
#32834=CARTESIAN_POINT('Ctrl Pts',(21.8082366141026,-66.0815998969239,36.));
#32835=CARTESIAN_POINT('Ctrl Pts',(21.8097407511271,-66.1077575099097,36.));
#32836=CARTESIAN_POINT('Ctrl Pts',(21.8103981162414,-66.1191893821185,36.));
#32837=CARTESIAN_POINT('Ctrl Pts',(21.8109471251284,-66.1306303661247,36.));
#32838=CARTESIAN_POINT('Ctrl Pts',(21.8113867843205,-66.142064834931,36.));
#32839=CARTESIAN_POINT('Ctrl Pts',(21.8140831607178,-66.2121910425829,36.));
#32840=CARTESIAN_POINT('Ctrl Pts',(21.8126787994894,-66.2822035594926,36.));
#32841=CARTESIAN_POINT('Ctrl Pts',(21.807119070444,-66.3517415844535,36.));
#32842=CARTESIAN_POINT('Ctrl Pts',(21.8021495116634,-66.4138980851956,36.));
#32843=CARTESIAN_POINT('Ctrl Pts',(21.7938596040808,-66.4756764464129,36.));
#32844=CARTESIAN_POINT('Ctrl Pts',(21.7821772238541,-66.5368311292835,36.));
#32845=CARTESIAN_POINT('Ctrl Pts',(21.7694467741587,-66.6034722245754,36.));
#32846=CARTESIAN_POINT('Ctrl Pts',(21.7526889329907,-66.6693735500384,36.));
#32847=CARTESIAN_POINT('Ctrl Pts',(21.7321489317058,-66.7343215285417,36.));
#32848=CARTESIAN_POINT('Ctrl Pts',(21.7242195708332,-66.759394358497,36.));
#32849=CARTESIAN_POINT('Ctrl Pts',(21.7157259981709,-66.7843250634018,36.));
#32850=CARTESIAN_POINT('Ctrl Pts',(21.7066803125378,-66.8091010351353,36.));
#32851=CARTESIAN_POINT('Ctrl Pts',(21.7027129368494,-66.8199676064378,36.));
#32852=CARTESIAN_POINT('Ctrl Pts',(21.6986394561303,-66.8308038451866,36.));
#32853=CARTESIAN_POINT('Ctrl Pts',(21.6944659765069,-66.8415961511061,36.));
#32854=CARTESIAN_POINT('Ctrl Pts',(21.6692431579055,-66.9068204720712,36.));
#32855=CARTESIAN_POINT('Ctrl Pts',(21.6403295196211,-66.9705593823762,36.));
#32856=CARTESIAN_POINT('Ctrl Pts',(21.6080377187698,-67.0325940771992,36.));
#32857=CARTESIAN_POINT('Ctrl Pts',(21.5749979079346,-67.096065748897,36.));
#32858=CARTESIAN_POINT('Ctrl Pts',(21.5384213156165,-67.157754156812,36.));
#32859=CARTESIAN_POINT('Ctrl Pts',(21.4985866955678,-67.2174212222795,36.));
#32860=CARTESIAN_POINT('Ctrl Pts',(21.4680940165069,-67.2630952785546,36.));
#32861=CARTESIAN_POINT('Ctrl Pts',(21.4356910398801,-67.3075849362939,36.));
#32862=CARTESIAN_POINT('Ctrl Pts',(21.4014832506304,-67.3507773033314,36.));
#32863=CARTESIAN_POINT('Ctrl Pts',(21.3801866940076,-67.3776673395035,36.));
#32864=CARTESIAN_POINT('Ctrl Pts',(21.3581902924914,-67.4040544403295,36.));
#32865=CARTESIAN_POINT('Ctrl Pts',(21.3355165916172,-67.429909675599,36.));
#32866=CARTESIAN_POINT('Ctrl Pts',(21.3228385096308,-67.4443667240687,36.));
#32867=CARTESIAN_POINT('Ctrl Pts',(21.3099442020298,-67.4586620153457,36.));
#32868=CARTESIAN_POINT('Ctrl Pts',(21.2968612936531,-67.4727650868957,36.));
#32869=CARTESIAN_POINT('Ctrl Pts',(21.2459900429151,-67.5276031143693,36.));
#32870=CARTESIAN_POINT('Ctrl Pts',(21.1922222505013,-67.5795961990397,36.));
#32871=CARTESIAN_POINT('Ctrl Pts',(21.1358428630979,-67.6284804213933,36.));
#32872=CARTESIAN_POINT('Ctrl Pts',(21.0936832829337,-67.665035240202,36.));
#32873=CARTESIAN_POINT('Ctrl Pts',(21.0500621937908,-67.6998514460096,36.));
#32874=CARTESIAN_POINT('Ctrl Pts',(21.0050823566734,-67.7328089375165,36.));
#32875=CARTESIAN_POINT('Ctrl Pts',(20.9910187117724,-67.7431136092779,36.));
#32876=CARTESIAN_POINT('Ctrl Pts',(20.9768221434489,-67.7532364967075,36.));
#32877=CARTESIAN_POINT('Ctrl Pts',(20.9624955512963,-67.7631737019372,36.));
#32878=CARTESIAN_POINT('Ctrl Pts',(20.948706193103,-67.7727382711587,36.));
#32879=CARTESIAN_POINT('Ctrl Pts',(20.9348034207359,-67.7821258761528,36.));
#32880=CARTESIAN_POINT('Ctrl Pts',(20.9207951934865,-67.7913303004398,36.));
#32881=CARTESIAN_POINT('Ctrl Pts',(20.8578414918468,-67.8326954617846,36.));
#32882=CARTESIAN_POINT('Ctrl Pts',(20.7927303375038,-67.8703849464026,36.));
#32883=CARTESIAN_POINT('Ctrl Pts',(20.725723015022,-67.9041195865683,36.));
#32884=CARTESIAN_POINT('Ctrl Pts',(20.6744956038834,-67.9299098766049,36.));
#32885=CARTESIAN_POINT('Ctrl Pts',(20.6221589702671,-67.9533882814079,36.));
#32886=CARTESIAN_POINT('Ctrl Pts',(20.5688159963225,-67.9744148066548,36.));
#32887=CARTESIAN_POINT('Ctrl Pts',(20.5563687509165,-67.9793212132615,36.));
#32888=CARTESIAN_POINT('Ctrl Pts',(20.5438666667748,-67.9840940496098,36.));
#32889=CARTESIAN_POINT('Ctrl Pts',(20.5313116823135,-67.9887339044341,36.));
#32890=CARTESIAN_POINT('Ctrl Pts',(18.332682461926,-66.0013023226252,34.8714803633902));
#32891=CARTESIAN_POINT('Ctrl Pts',(18.3319481762167,-66.0867862325851,34.8772098489549));
#32892=CARTESIAN_POINT('Ctrl Pts',(18.3379547950258,-66.1721666149879,34.8829393345197));
#32893=CARTESIAN_POINT('Ctrl Pts',(18.3510613606819,-66.256442733634,34.8886688200844));
#32894=CARTESIAN_POINT('Ctrl Pts',(18.435802738773,-66.8013356233214,34.9257131927482));
#32895=CARTESIAN_POINT('Ctrl Pts',(18.817347144873,-67.3000663608468,34.9627575654121));
#32896=CARTESIAN_POINT('Ctrl Pts',(19.3210929435872,-67.5244144340681,34.999801938076));
#32897=CARTESIAN_POINT('Ctrl Pts',(19.8248387423015,-67.7487625072893,35.0368463107398));
#32898=CARTESIAN_POINT('Ctrl Pts',(20.45078593363,-67.6987279162063,35.0738906834037));
#32899=CARTESIAN_POINT('Ctrl Pts',(20.9124875808018,-67.3971905495061,35.1109350560675));
#32900=CARTESIAN_POINT('Ctrl Pts',(21.3741892279737,-67.095653182806,35.1479794287314));
#32901=CARTESIAN_POINT('Ctrl Pts',(21.6716453309889,-66.5426130404886,35.1850238013952));
#32902=CARTESIAN_POINT('Ctrl Pts',(21.6687364829936,-65.9911859221278,35.2220681740591));
#32903=CARTESIAN_POINT('Ctrl Pts',(21.6658276349983,-65.439758803767,35.2591125467229));
#32904=CARTESIAN_POINT('Ctrl Pts',(21.3625538359925,-64.8899447093626,35.2961569193868));
#32905=CARTESIAN_POINT('Ctrl Pts',(20.8976944399262,-64.5932820999738,35.3332012920506));
#32906=CARTESIAN_POINT('Ctrl Pts',(20.4328350438599,-64.2966194905849,35.3702456647145));
#32907=CARTESIAN_POINT('Ctrl Pts',(19.806390050733,-64.2531083662115,35.4072900373783));
#32908=CARTESIAN_POINT('Ctrl Pts',(19.3050423947062,-64.4827944521564,35.4443344100422));
#32909=CARTESIAN_POINT('Ctrl Pts',(18.8036947386794,-64.7124805381013,35.481378782706));
#32910=CARTESIAN_POINT('Ctrl Pts',(18.4274444197528,-65.2153638343645,35.5184231553699));
#32911=CARTESIAN_POINT('Ctrl Pts',(18.3484523433302,-65.7610473705247,35.5554675280338));
#32912=CARTESIAN_POINT('Ctrl Pts',(18.3370706135895,-65.8396732633204,35.5608051398192));
#32913=CARTESIAN_POINT('Ctrl Pts',(18.3318602794101,-65.9191877343715,35.5661427516047));
#32914=CARTESIAN_POINT('Ctrl Pts',(18.3325226604529,-65.9987867968397,35.5714803633902));
#32915=CARTESIAN_POINT('Ctrl Pts',(19.4698297828114,-67.9851743256717,36.));
#32916=CARTESIAN_POINT('Ctrl Pts',(18.8097404375819,-67.8088876857537,35.9629556273362));
#32917=CARTESIAN_POINT('Ctrl Pts',(17.6907269068218,-66.7486281566044,35.8888668820084));
#32918=CARTESIAN_POINT('Ctrl Pts',(18.1186750965977,-64.4618780498746,35.7777337640169));
#32919=CARTESIAN_POINT('Ctrl Pts',(20.2718170744413,-63.5871690673869,35.6666006460253));
#32920=CARTESIAN_POINT('Ctrl Pts',(22.1745314797546,-64.9187024309931,35.5554675280338));
#32921=CARTESIAN_POINT('Ctrl Pts',(22.0878551535464,-67.240916575683,35.4443344100422));
#32922=CARTESIAN_POINT('Ctrl Pts',(20.0898773540102,-68.4268764895147,35.3332012920506));
#32923=CARTESIAN_POINT('Ctrl Pts',(18.0098480595359,-67.3919235970992,35.2220681740591));
#32924=CARTESIAN_POINT('Ctrl Pts',(17.751179915361,-65.0828969822093,35.1109350560676));
#32925=CARTESIAN_POINT('Ctrl Pts',(19.5507727141961,-63.6133045893429,34.9998019380759));
#32926=CARTESIAN_POINT('Ctrl Pts',(21.761489776565,-64.3280769471683,34.8886688200845));
#32927=CARTESIAN_POINT('Ctrl Pts',(22.3600352216356,-66.5730755571057,34.7775357020928));
#32928=CARTESIAN_POINT('Ctrl Pts',(20.7985769413999,-68.2935646002867,34.6664025841013));
#32929=CARTESIAN_POINT('Ctrl Pts',(18.5062329236883,-67.9148971913879,34.5552694661097));
#32930=CARTESIAN_POINT('Ctrl Pts',(17.5810416674194,-65.7836384245792,34.4441363481182));
#32931=CARTESIAN_POINT('Ctrl Pts',(18.8697771195624,-63.8504033302666,34.3330032301266));
#32932=CARTESIAN_POINT('Ctrl Pts',(21.1929366190789,-63.8845631923098,34.2218701121351));
#32933=CARTESIAN_POINT('Ctrl Pts',(22.4242737809404,-65.8548543459294,34.1107369941435));
#32934=CARTESIAN_POINT('Ctrl Pts',(21.4368200548297,-67.9579883834045,33.9996038761519));
#32935=CARTESIAN_POINT('Ctrl Pts',(19.134332114609,-68.2690944527448,33.8884707581604));
#32936=CARTESIAN_POINT('Ctrl Pts',(17.6241374689897,-66.5034359351233,33.7773376401688));
#32937=CARTESIAN_POINT('Ctrl Pts',(18.2884257380644,-64.2770130512471,33.6662045221773));
#32938=CARTESIAN_POINT('Ctrl Pts',(20.5192141319096,-63.6275356306401,33.5550714041857));
#32939=CARTESIAN_POINT('Ctrl Pts',(22.2747973195027,-65.14943098434,33.4439382861942));
#32940=CARTESIAN_POINT('Ctrl Pts',(21.9483964634611,-67.4498005771448,33.3328051682026));
#32941=CARTESIAN_POINT('Ctrl Pts',(19.838746476763,-68.4232556192041,33.221672050211));
#32942=CARTESIAN_POINT('Ctrl Pts',(17.8766820609866,-67.1788517396284,33.1105389322195));
#32943=CARTESIAN_POINT('Ctrl Pts',(17.8579617961865,-64.855516349057,32.9994058142279));
#32944=CARTESIAN_POINT('Ctrl Pts',(19.7997192052125,-63.5796574421335,32.8882726962363));
#32945=CARTESIAN_POINT('Ctrl Pts',(21.9247814806566,-64.5189913079908,32.7771395782448));
#32946=CARTESIAN_POINT('Ctrl Pts',(22.2882079863162,-66.8138026206755,32.6660064602532));
#32947=CARTESIAN_POINT('Ctrl Pts',(20.5573764799239,-68.3637897439758,32.5548733422617));
#32948=CARTESIAN_POINT('Ctrl Pts',(18.3164120809741,-67.7503434557233,32.4437402242701));
#32949=CARTESIAN_POINT('Ctrl Pts',(17.6163336108949,-65.53491394395,32.3326071062785));
#32950=CARTESIAN_POINT('Ctrl Pts',(19.0978804403178,-63.7451494962803,32.221473988287));
#32951=CARTESIAN_POINT('Ctrl Pts',(21.4050825978426,-64.0191129796669,32.1103408702954));
#32952=CARTESIAN_POINT('Ctrl Pts',(22.4262978583092,-66.1060622310153,31.9992077523039));
#32953=CARTESIAN_POINT('Ctrl Pts',(21.2268698206984,-68.0959391539699,31.8880746343123));
#32954=CARTESIAN_POINT('Ctrl Pts',(18.9045622340586,-68.16753006785,31.7769415163208));
#32955=CARTESIAN_POINT('Ctrl Pts',(17.5848424068188,-66.2553121504816,31.6658083983292));
#32956=CARTESIAN_POINT('Ctrl Pts',(18.4755698685349,-64.1094225040042,31.5546752803376));
#32957=CARTESIAN_POINT('Ctrl Pts',(20.7615157875532,-63.6938637942672,31.4435421623461));
#32958=CARTESIAN_POINT('Ctrl Pts',(22.3504924848334,-65.3889717086535,31.3324090443545));
#32959=CARTESIAN_POINT('Ctrl Pts',(21.7882059455114,-67.6433167651191,31.221275926363));
#32960=CARTESIAN_POINT('Ctrl Pts',(19.5892829417572,-68.3936336378304,31.1101428083714));
#32961=CARTESIAN_POINT('Ctrl Pts',(17.7662643553727,-66.9532027926971,30.9990096903798));
#32962=CARTESIAN_POINT('Ctrl Pts',(17.9876485499293,-64.6403632339913,30.8878765723883));
#32963=CARTESIAN_POINT('Ctrl Pts',(20.0508159969719,-63.5719167583182,30.7767434543967));
#32964=CARTESIAN_POINT('Ctrl Pts',(22.0674746434876,-64.7257476338574,30.6656103364051));
#32965=CARTESIAN_POINT('Ctrl Pts',(22.1918991212745,-67.0458244289748,30.5544772184136));
#32966=CARTESIAN_POINT('Ctrl Pts',(20.3102112509622,-68.4087215434459,30.443344100422));
#32967=CARTESIAN_POINT('Ctrl Pts',(18.1446058339735,-67.5670618949994,30.3322109824305));
#32968=CARTESIAN_POINT('Ctrl Pts',(17.6771301853349,-65.2911655212942,30.2210778644389));
#32969=CARTESIAN_POINT('Ctrl Pts',(19.3356364183429,-63.6640223619538,30.1099447464474));
#32970=CARTESIAN_POINT('Ctrl Pts',(21.6021943503792,-64.1748578801372,29.9988116284558));
#32971=CARTESIAN_POINT('Ctrl Pts',(22.4023609511933,-66.3561353033128,29.8876785104642));
#32972=CARTESIAN_POINT('Ctrl Pts',(21.0037922534698,-68.2114636795477,29.7765453924727));
#32973=CARTESIAN_POINT('Ctrl Pts',(18.6865133764925,-68.0427734538981,29.6654122744811));
#32974=CARTESIAN_POINT('Ctrl Pts',(17.5713891556791,-66.0044565604616,29.5542791564896));
#32975=CARTESIAN_POINT('Ctrl Pts',(18.6790251687795,-63.9620608474818,29.443146038498));
#32976=CARTESIAN_POINT('Ctrl Pts',(20.9956693404756,-63.7848672593903,29.3320129205065));
#32977=CARTESIAN_POINT('Ctrl Pts',(22.4010377426051,-65.6350503422798,29.2208798025149));
#32978=CARTESIAN_POINT('Ctrl Pts',(21.6088818987778,-67.8192497161933,29.1097466845234));
#32979=CARTESIAN_POINT('Ctrl Pts',(19.3442140162146,-68.3384001448757,28.9986135665318));
#32980=CARTESIAN_POINT('Ctrl Pts',(17.6797472774965,-66.717354722435,28.8874804485402));
#32981=CARTESIAN_POINT('Ctrl Pts',(18.1388671546711,-64.439758023215,28.7763473305486));
#32982=CARTESIAN_POINT('Ctrl Pts',(20.3013690653653,-63.5901561916745,28.6652142125571));
#32983=CARTESIAN_POINT('Ctrl Pts',(22.188046145667,-64.9461382640413,28.5540810945655));
#32984=CARTESIAN_POINT('Ctrl Pts',(22.0721372727958,-67.2666560767515,28.442947976574));
#32985=CARTESIAN_POINT('Ctrl Pts',(20.0597268093363,-68.4278803929209,28.3318148585824));
#32986=CARTESIAN_POINT('Ctrl Pts',(17.9926520191425,-67.3670130130489,28.2206817405909));
#32987=CARTESIAN_POINT('Ctrl Pts',(17.7627811094867,-65.0550015185249,28.1095486225993));
#32988=CARTESIAN_POINT('Ctrl Pts',(19.580500984485,-63.6078898290281,27.9984155046077));
#32989=CARTESIAN_POINT('Ctrl Pts',(21.7821628698452,-64.3501315205369,27.8872823866162));
#32990=CARTESIAN_POINT('Ctrl Pts',(22.3527191513918,-66.6023977826542,27.7761492686246));
#32991=CARTESIAN_POINT('Ctrl Pts',(20.7699742636292,-68.3033258839143,27.6650161506331));
#32992=CARTESIAN_POINT('Ctrl Pts',(18.4825186235667,-67.896159478245,27.5538830326415));
#32993=CARTESIAN_POINT('Ctrl Pts',(17.5839216673683,-65.7535532858717,27.44274991465));
#32994=CARTESIAN_POINT('Ctrl Pts',(18.8966146957805,-63.836504826525,27.3316167966584));
#32995=CARTESIAN_POINT('Ctrl Pts',(21.219169386089,-63.8995723038675,27.2204836786668));
#32996=CARTESIAN_POINT('Ctrl Pts',(22.4258922629222,-65.8850338815669,27.1093505606752));
#32997=CARTESIAN_POINT('Ctrl Pts',(21.41234306908,-67.9757169742283,26.9982174426837));
#32998=CARTESIAN_POINT('Ctrl Pts',(19.1061618881228,-68.2581461319033,26.8870843246921));
#32999=CARTESIAN_POINT('Ctrl Pts',(17.6180565701669,-66.4738310633369,26.7759512067006));
#33000=CARTESIAN_POINT('Ctrl Pts',(18.3099995480748,-64.2558471688686,26.664818088709));
#33001=CARTESIAN_POINT('Ctrl Pts',(20.5486976238089,-63.6341805685774,26.5536849707175));
#33002=CARTESIAN_POINT('Ctrl Pts',(22.2852057058799,-65.1778050816215,26.4425518527259));
#33003=CARTESIAN_POINT('Ctrl Pts',(21.9302042425984,-67.4739346416768,26.3314187347344));
#33004=CARTESIAN_POINT('Ctrl Pts',(19.8086025657231,-68.4210614106236,26.2202856167428));
#33005=CARTESIAN_POINT('Ctrl Pts',(17.8621779827765,-67.1523370729513,26.1091524987513));
#33006=CARTESIAN_POINT('Ctrl Pts',(17.8723670134724,-64.8289493110236,25.9980193807597));
#33007=CARTESIAN_POINT('Ctrl Pts',(19.829859942873,-63.5773515961876,25.8868862627681));
#33008=CARTESIAN_POINT('Ctrl Pts',(21.9430509240163,-64.5430603155101,25.7757531447765));
#33009=CARTESIAN_POINT('Ctrl Pts',(22.2779267364902,-66.8422110789462,25.664620026785));
#33010=CARTESIAN_POINT('Ctrl Pts',(20.5278715823273,-68.3705500709468,25.5534869087934));
#33011=CARTESIAN_POINT('Ctrl Pts',(18.2948525586908,-67.7292425039652,25.4423537908019));
#33012=CARTESIAN_POINT('Ctrl Pts',(17.6221226977641,-65.5053156304209,25.3312206728103));
#33013=CARTESIAN_POINT('Ctrl Pts',(19.1263754391461,-63.7340406632385,25.2200875548188));
#33014=CARTESIAN_POINT('Ctrl Pts',(21.4288957812291,-64.0368661589902,25.1089544368272));
#33015=CARTESIAN_POINT('Ctrl Pts',(22.4262529035541,-66.1360124024293,24.9978213188356));
#33016=CARTESIAN_POINT('Ctrl Pts',(21.1976530167761,-68.1115902981272,24.8866882008441));
#33017=CARTESIAN_POINT('Ctrl Pts',(19.656339145916,-68.1379171412778,24.8125994555164));
#33018=CARTESIAN_POINT('Ctrl Pts',(19.0504464477384,-67.8221815534923,24.7755550828525));
#33019=CARTESIAN_POINT('Ctrl Pts',(19.5032651029123,-67.8599788000028,36.0748149723825));
#33020=CARTESIAN_POINT('Ctrl Pts',(18.8848044607623,-67.6948097220376,36.0377705997186));
#33021=CARTESIAN_POINT('Ctrl Pts',(17.8363618040069,-66.7014157307813,35.963681854391));
#33022=CARTESIAN_POINT('Ctrl Pts',(18.2373213319382,-64.558880103346,35.8525487363994));
#33023=CARTESIAN_POINT('Ctrl Pts',(20.254674861246,-63.7393348661546,35.7414156184078));
#33024=CARTESIAN_POINT('Ctrl Pts',(22.03739409682,-64.9868947382407,35.6302825004162));
#33025=CARTESIAN_POINT('Ctrl Pts',(21.9561840352528,-67.1626578550281,35.5191493824247));
#33026=CARTESIAN_POINT('Ctrl Pts',(20.0842092157336,-68.2738249041152,35.4080162644331));
#33027=CARTESIAN_POINT('Ctrl Pts',(18.1353574997526,-67.3041415800863,35.2968831464416));
#33028=CARTESIAN_POINT('Ctrl Pts',(17.8930023281287,-65.1407343181651,35.18575002845));
#33029=CARTESIAN_POINT('Ctrl Pts',(19.5791033476643,-63.763822144746,35.0746169104584));
#33030=CARTESIAN_POINT('Ctrl Pts',(21.6504009740928,-64.4335172013417,34.9634837924669));
#33031=CARTESIAN_POINT('Ctrl Pts',(22.2111989978597,-66.536934400789,34.8523506744753));
#33032=CARTESIAN_POINT('Ctrl Pts',(20.7482144827116,-68.1489203632162,34.7412175564838));
#33033=CARTESIAN_POINT('Ctrl Pts',(18.6004377257187,-67.7941337111346,34.6300844384922));
#33034=CARTESIAN_POINT('Ctrl Pts',(17.7335938922303,-65.7972833225707,34.5189513205007));
#33035=CARTESIAN_POINT('Ctrl Pts',(18.9410549140662,-63.9859681930413,34.4078182025091));
#33036=CARTESIAN_POINT('Ctrl Pts',(21.1177037666367,-64.0179737546636,34.2966850845176));
#33037=CARTESIAN_POINT('Ctrl Pts',(22.2713863360217,-65.8640079936593,34.185551966526));
#33038=CARTESIAN_POINT('Ctrl Pts',(21.3462066312477,-67.8345073461254,34.0744188485344));
#33039=CARTESIAN_POINT('Ctrl Pts',(19.1889256808086,-68.1259934317763,33.9632857305429));
#33040=CARTESIAN_POINT('Ctrl Pts',(17.7739718460721,-66.4716866193462,33.8521526125513));
#33041=CARTESIAN_POINT('Ctrl Pts',(18.3963666058631,-64.3856736630535,33.7410194945598));
#33042=CARTESIAN_POINT('Ctrl Pts',(20.486469760124,-63.7771557017904,33.6298863765682));
#33043=CARTESIAN_POINT('Ctrl Pts',(22.1313366457862,-65.2030723364652,33.5187532585766));
#33044=CARTESIAN_POINT('Ctrl Pts',(21.8255203430619,-67.3583685336091,33.4076201405851));
#33045=CARTESIAN_POINT('Ctrl Pts',(19.8489159713744,-68.2704323849152,33.2964870225935));
#33046=CARTESIAN_POINT('Ctrl Pts',(18.0105896488994,-67.1045071537046,33.185353904602));
#33047=CARTESIAN_POINT('Ctrl Pts',(17.9930499823782,-64.9276935026936,33.0742207866103));
#33048=CARTESIAN_POINT('Ctrl Pts',(19.812349964668,-63.7322969634655,32.9630876686189));
#33049=CARTESIAN_POINT('Ctrl Pts',(21.803394645177,-64.612391499258,32.8519545506273));
#33050=CARTESIAN_POINT('Ctrl Pts',(22.1439015654733,-66.7624799506366,32.7408214326357));
#33051=CARTESIAN_POINT('Ctrl Pts',(20.5222253899178,-68.2147167402899,32.6296883146442));
#33052=CARTESIAN_POINT('Ctrl Pts',(18.4225879829121,-67.6399575988206,32.5185551966526));
#33053=CARTESIAN_POINT('Ctrl Pts',(17.7666601402804,-65.5642447148125,32.4074220786611));
#33054=CARTESIAN_POINT('Ctrl Pts',(19.1547728406628,-63.887352218967,32.2962889606695));
#33055=CARTESIAN_POINT('Ctrl Pts',(21.3164707050882,-64.1440381253301,32.185155842678));
#33056=CARTESIAN_POINT('Ctrl Pts',(22.2732827644345,-66.0993733893383,32.0740227246863));
#33057=CARTESIAN_POINT('Ctrl Pts',(21.1494969622328,-67.9637582161257,31.9628896066948));
#33058=CARTESIAN_POINT('Ctrl Pts',(18.973646296436,-68.0308342307446,31.8517564887032));
#33059=CARTESIAN_POINT('Ctrl Pts',(17.7371549370292,-66.2392108245296,31.7406233707117));
#33060=CARTESIAN_POINT('Ctrl Pts',(18.571708443967,-64.2286522564588,31.6294902527201));
#33061=CARTESIAN_POINT('Ctrl Pts',(20.7134905999941,-63.8393008628447,31.5183571347286));
#33062=CARTESIAN_POINT('Ctrl Pts',(22.2022580761902,-65.4275063638444,31.407224016737));
#33063=CARTESIAN_POINT('Ctrl Pts',(21.6754322810238,-67.5396805737836,31.2960908987455));
#33064=CARTESIAN_POINT('Ctrl Pts',(19.6151849178925,-68.2426785213593,31.1849577807539));
#33065=CARTESIAN_POINT('Ctrl Pts',(17.90713546408,-66.8930888152204,31.0738246627624));
#33066=CARTESIAN_POINT('Ctrl Pts',(18.1145580078869,-64.7261090737586,30.9626915447707));
#33067=CARTESIAN_POINT('Ctrl Pts',(20.0476112731494,-63.7250444478512,30.8515584267792));
#33068=CARTESIAN_POINT('Ctrl Pts',(21.9370888272641,-64.8061086846483,30.7404253087876));
#33069=CARTESIAN_POINT('Ctrl Pts',(22.0536664435935,-66.9798692443596,30.6292921907961));
#33070=CARTESIAN_POINT('Ctrl Pts',(20.2906476992225,-68.2568149043553,30.5181590728045));
#33071=CARTESIAN_POINT('Ctrl Pts',(18.2616167407412,-67.468234736516,30.407025954813));
#33072=CARTESIAN_POINT('Ctrl Pts',(17.8236225632318,-65.3358683486612,30.2958928368214));
#33073=CARTESIAN_POINT('Ctrl Pts',(19.377534677234,-63.8113413880787,30.1847597188299));
#33074=CARTESIAN_POINT('Ctrl Pts',(21.5011515546278,-64.2899609338901,30.0736266008383));
#33075=CARTESIAN_POINT('Ctrl Pts',(22.250855444477,-66.3336755394871,29.9624934828468));
#33076=CARTESIAN_POINT('Ctrl Pts',(20.9404878387337,-68.0719971580043,29.8513603648552));
#33077=CARTESIAN_POINT('Ctrl Pts',(18.7693487457408,-67.9139454245023,29.7402272468636));
#33078=CARTESIAN_POINT('Ctrl Pts',(17.7245501186072,-66.0041755063383,29.6290941288721));
#33079=CARTESIAN_POINT('Ctrl Pts',(18.7623327837589,-64.0905840004269,29.5179610108805));
#33080=CARTESIAN_POINT('Ctrl Pts',(20.9328771993214,-63.9245651712063,29.4068278928889));
#33081=CARTESIAN_POINT('Ctrl Pts',(22.2496156843762,-65.6580659856165,29.2956947748974));
#33082=CARTESIAN_POINT('Ctrl Pts',(21.5074173510794,-67.7045182683821,29.1845616569058));
#33083=CARTESIAN_POINT('Ctrl Pts',(19.385571326706,-68.1909283427392,29.0734285389143));
#33084=CARTESIAN_POINT('Ctrl Pts',(17.8260746078081,-66.6721145637219,28.9622954209227));
#33085=CARTESIAN_POINT('Ctrl Pts',(18.2562399727141,-64.5381550818151,28.8511623029312));
#33086=CARTESIAN_POINT('Ctrl Pts',(20.2823631483176,-63.7421336066862,28.7400291849396));
#33087=CARTESIAN_POINT('Ctrl Pts',(22.0500564568764,-65.0126003234735,28.6288960669481));
#33088=CARTESIAN_POINT('Ctrl Pts',(21.9414574066646,-67.1867740878903,28.5177629489565));
#33089=CARTESIAN_POINT('Ctrl Pts',(20.0559601228571,-68.2747654960968,28.4066298309649));
#33090=CARTESIAN_POINT('Ctrl Pts',(18.1192459320368,-67.2808019883787,28.2954967129734));
#33091=CARTESIAN_POINT('Ctrl Pts',(17.9038718899851,-65.1145980890199,28.1843635949818));
#33092=CARTESIAN_POINT('Ctrl Pts',(19.6069567969976,-63.7587488676727,28.0732304769902));
#33093=CARTESIAN_POINT('Ctrl Pts',(21.6697703134673,-64.4541808974103,27.9620973589987));
#33094=CARTESIAN_POINT('Ctrl Pts',(22.2043443174536,-66.5644074126972,27.8509642410071));
#33095=CARTESIAN_POINT('Ctrl Pts',(20.7214156401169,-68.1580660489999,27.7398311230156));
#33096=CARTESIAN_POINT('Ctrl Pts',(18.5782189739886,-67.7765776966548,27.628698005024));
#33097=CARTESIAN_POINT('Ctrl Pts',(17.7362922642471,-65.7690955108168,27.5175648870325));
#33098=CARTESIAN_POINT('Ctrl Pts',(18.9661999716884,-63.9729462019864,27.4064317690409));
#33099=CARTESIAN_POINT('Ctrl Pts',(21.142282157498,-64.0320363127692,27.2952986510493));
#33100=CARTESIAN_POINT('Ctrl Pts',(22.2729027480241,-65.892284249177,27.1841655330578));
#33101=CARTESIAN_POINT('Ctrl Pts',(21.3232732928534,-67.8511178788426,27.0730324150662));
#33102=CARTESIAN_POINT('Ctrl Pts',(19.1625320168477,-68.1157355695839,26.9618992970746));
#33103=CARTESIAN_POINT('Ctrl Pts',(17.7682744406861,-66.4439487863571,26.8507661790831));
#33104=CARTESIAN_POINT('Ctrl Pts',(18.4165798580372,-64.365842612451,26.7396330610915));
#33105=CARTESIAN_POINT('Ctrl Pts',(20.5140938680794,-63.7833815750203,26.6284999431));
#33106=CARTESIAN_POINT('Ctrl Pts',(22.1410886246193,-65.2296570140577,26.5173668251084));
#33107=CARTESIAN_POINT('Ctrl Pts',(21.8084754192525,-67.3809805771999,26.4062337071169));
#33108=CARTESIAN_POINT('Ctrl Pts',(19.82067309378,-68.2683765546589,26.2951005891253));
#33109=CARTESIAN_POINT('Ctrl Pts',(17.9970002740845,-67.0796646412509,26.1839674711337));
#33110=CARTESIAN_POINT('Ctrl Pts',(18.0065467309583,-64.9028019216962,26.0728343531422));
#33111=CARTESIAN_POINT('Ctrl Pts',(19.840589869013,-63.7301365362829,25.9617012351506));
#33112=CARTESIAN_POINT('Ctrl Pts',(21.8205119214269,-64.634942588673,25.850568117159));
#33113=CARTESIAN_POINT('Ctrl Pts',(22.1342687052924,-66.7890968222338,25.7394349991675));
#33114=CARTESIAN_POINT('Ctrl Pts',(20.4945812262208,-68.2210507255145,25.6283018811759));
#33115=CARTESIAN_POINT('Ctrl Pts',(18.4023881174058,-67.6201873839723,25.5171687631844));
#33116=CARTESIAN_POINT('Ctrl Pts',(17.7720841369082,-65.5365130264827,25.4060356451928));
#33117=CARTESIAN_POINT('Ctrl Pts',(19.1814707951151,-63.876943967317,25.2949025272013));
#33118=CARTESIAN_POINT('Ctrl Pts',(21.3387821039848,-64.1606716958669,25.1837694092097));
#33119=CARTESIAN_POINT('Ctrl Pts',(22.2732406447625,-66.1274347455458,25.0726362912181));
#33120=CARTESIAN_POINT('Ctrl Pts',(21.1221227235089,-67.9784223168809,24.9615031732266));
#33121=CARTESIAN_POINT('Ctrl Pts',(19.6780122054163,-68.003088850947,24.8874144278989));
#33122=CARTESIAN_POINT('Ctrl Pts',(19.1103302849355,-67.7072652086133,24.850370055235));
#33123=CARTESIAN_POINT('Ctrl Pts',(19.5367004230132,-67.7347832743338,36.149629944765));
#33124=CARTESIAN_POINT('Ctrl Pts',(18.9598684839428,-67.5807317583216,36.1125855721011));
#33125=CARTESIAN_POINT('Ctrl Pts',(17.981996701192,-66.6542033049582,36.0384968267734));
#33126=CARTESIAN_POINT('Ctrl Pts',(18.3559675672787,-64.6558821568174,35.9273637087819));
#33127=CARTESIAN_POINT('Ctrl Pts',(20.2375326480507,-63.8915006649221,35.8162305907903));
#33128=CARTESIAN_POINT('Ctrl Pts',(21.9002567138854,-65.0550870454884,35.7050974727987));
#33129=CARTESIAN_POINT('Ctrl Pts',(21.8245129169592,-67.0843991343733,35.5939643548072));
#33130=CARTESIAN_POINT('Ctrl Pts',(20.078541077457,-68.1207733187157,35.4828312368156));
#33131=CARTESIAN_POINT('Ctrl Pts',(18.2608669399692,-67.2163595630733,35.3716981188241));
#33132=CARTESIAN_POINT('Ctrl Pts',(18.0348247408964,-65.1985716541211,35.2605650008325));
#33133=CARTESIAN_POINT('Ctrl Pts',(19.6074339811324,-63.9143397001489,35.149431882841));
#33134=CARTESIAN_POINT('Ctrl Pts',(21.5393121716205,-64.5389574555151,35.0382987648494));
#33135=CARTESIAN_POINT('Ctrl Pts',(22.0623627740838,-66.5007932444724,34.9271656468579));
#33136=CARTESIAN_POINT('Ctrl Pts',(20.6978520240233,-68.0042761261457,34.8160325288663));
#33137=CARTESIAN_POINT('Ctrl Pts',(18.6946425277492,-67.6733702308812,34.7048994108747));
#33138=CARTESIAN_POINT('Ctrl Pts',(17.8861461170412,-65.8109282205623,34.5937662928832));
#33139=CARTESIAN_POINT('Ctrl Pts',(19.01233270857,-64.121533055816,34.4826331748916));
#33140=CARTESIAN_POINT('Ctrl Pts',(21.0424709141944,-64.1513843170174,34.3715000569001));
#33141=CARTESIAN_POINT('Ctrl Pts',(22.1184988911029,-65.8731616413895,34.2603669389085));
#33142=CARTESIAN_POINT('Ctrl Pts',(21.2555932076657,-67.7110263088461,34.1492338209169));
#33143=CARTESIAN_POINT('Ctrl Pts',(19.2435192470082,-67.9828924108079,34.0381007029253));
#33144=CARTESIAN_POINT('Ctrl Pts',(17.9238062231545,-66.4399373035691,33.9269675849338));
#33145=CARTESIAN_POINT('Ctrl Pts',(18.5043074736616,-64.4943342748599,33.8158344669423));
#33146=CARTESIAN_POINT('Ctrl Pts',(20.4537253883383,-63.9267757729409,33.7047013489506));
#33147=CARTESIAN_POINT('Ctrl Pts',(21.9878759720698,-65.2567136885904,33.5935682309591));
#33148=CARTESIAN_POINT('Ctrl Pts',(21.7026442226628,-67.2669364900734,33.4824351129675));
#33149=CARTESIAN_POINT('Ctrl Pts',(19.8590854659858,-68.1176091506262,33.371301994976));
#33150=CARTESIAN_POINT('Ctrl Pts',(18.1444972368122,-67.0301625677809,33.2601688769844));
#33151=CARTESIAN_POINT('Ctrl Pts',(18.12813816857,-64.9998706563301,33.1490357589929));
#33152=CARTESIAN_POINT('Ctrl Pts',(19.8249807241235,-63.8849364847975,33.0379026410013));
#33153=CARTESIAN_POINT('Ctrl Pts',(21.6820078096973,-64.7057916905251,32.9267695230098));
#33154=CARTESIAN_POINT('Ctrl Pts',(21.9995951446305,-66.7111572805976,32.8156364050182));
#33155=CARTESIAN_POINT('Ctrl Pts',(20.4870742999116,-68.0656437366041,32.7045032870267));
#33156=CARTESIAN_POINT('Ctrl Pts',(18.5287638848501,-67.5295717419178,32.5933701690351));
#33157=CARTESIAN_POINT('Ctrl Pts',(17.9169866696659,-65.5935754856751,32.4822370510435));
#33158=CARTESIAN_POINT('Ctrl Pts',(19.2116652410078,-64.0295549416535,32.371103933052));
#33159=CARTESIAN_POINT('Ctrl Pts',(21.2278588123338,-64.2689632709934,32.2599708150604));
#33160=CARTESIAN_POINT('Ctrl Pts',(22.1202676705596,-66.0926845476613,32.1488376970689));
#33161=CARTESIAN_POINT('Ctrl Pts',(21.0721241037672,-67.8315772782816,32.0377045790773));
#33162=CARTESIAN_POINT('Ctrl Pts',(19.0427303588134,-67.8941383936393,31.9265714610858));
#33163=CARTESIAN_POINT('Ctrl Pts',(17.8894674672395,-66.2231094985776,31.8154383430942));
#33164=CARTESIAN_POINT('Ctrl Pts',(18.667847019399,-64.3478820089134,31.7043052251026));
#33165=CARTESIAN_POINT('Ctrl Pts',(20.665465412435,-63.9847379314221,31.5931721071111));
#33166=CARTESIAN_POINT('Ctrl Pts',(22.054023667547,-65.4660410190354,31.4820389891195));
#33167=CARTESIAN_POINT('Ctrl Pts',(21.5626586165363,-67.4360443824481,31.3709058711279));
#33168=CARTESIAN_POINT('Ctrl Pts',(19.6410868940278,-68.0917234048882,31.2597727531364));
#33169=CARTESIAN_POINT('Ctrl Pts',(18.0480065727872,-66.8329748377437,31.1486396351448));
#33170=CARTESIAN_POINT('Ctrl Pts',(18.2414674658445,-64.8118549135259,31.0375065171533));
#33171=CARTESIAN_POINT('Ctrl Pts',(20.0444065493269,-63.8781721373842,30.9263733991617));
#33172=CARTESIAN_POINT('Ctrl Pts',(21.8067030110406,-64.8864697354392,30.8152402811701));
#33173=CARTESIAN_POINT('Ctrl Pts',(21.9154337659124,-66.9139140597444,30.7041071631786));
#33174=CARTESIAN_POINT('Ctrl Pts',(20.2710841474828,-68.1049082652647,30.592974045187));
#33175=CARTESIAN_POINT('Ctrl Pts',(18.3786276475089,-67.3694075780326,30.4818409271955));
#33176=CARTESIAN_POINT('Ctrl Pts',(17.9701149411287,-65.3805711760282,30.3707078092039));
#33177=CARTESIAN_POINT('Ctrl Pts',(19.419432936125,-63.9586604142035,30.2595746912124));
#33178=CARTESIAN_POINT('Ctrl Pts',(21.4001087588765,-64.4050639876431,30.1484415732208));
#33179=CARTESIAN_POINT('Ctrl Pts',(22.0993499377606,-66.3112157756614,30.0373084552292));
#33180=CARTESIAN_POINT('Ctrl Pts',(20.8771834239977,-67.9325306364607,29.9261753372377));
#33181=CARTESIAN_POINT('Ctrl Pts',(18.852184114989,-67.7851173951066,29.8150422192461));
#33182=CARTESIAN_POINT('Ctrl Pts',(17.8777110815354,-66.0038944522149,29.7039091012546));
#33183=CARTESIAN_POINT('Ctrl Pts',(18.8456403987383,-64.2191071533719,29.592775983263));
#33184=CARTESIAN_POINT('Ctrl Pts',(20.8700850581672,-64.0642630830224,29.4816428652715));
#33185=CARTESIAN_POINT('Ctrl Pts',(22.0981936261472,-65.6810816289533,29.3705097472799));
#33186=CARTESIAN_POINT('Ctrl Pts',(21.405952803381,-67.5897868205709,29.2593766292883));
#33187=CARTESIAN_POINT('Ctrl Pts',(19.4269286371974,-68.0434565406025,29.1482435112968));
#33188=CARTESIAN_POINT('Ctrl Pts',(17.9724019381197,-66.626874405009,29.0371103933052));
#33189=CARTESIAN_POINT('Ctrl Pts',(18.3736127907571,-64.636552140415,28.9259772753136));
#33190=CARTESIAN_POINT('Ctrl Pts',(20.26335723127,-63.8941110216982,28.8148441573221));
#33191=CARTESIAN_POINT('Ctrl Pts',(21.9120667680857,-65.0790623829053,28.7037110393305));
#33192=CARTESIAN_POINT('Ctrl Pts',(21.8107775405334,-67.1068920990293,28.592577921339));
#33193=CARTESIAN_POINT('Ctrl Pts',(20.0521934363779,-68.1216505992727,28.4814448033474));
#33194=CARTESIAN_POINT('Ctrl Pts',(18.245839844931,-67.1945909637086,28.3703116853559));
#33195=CARTESIAN_POINT('Ctrl Pts',(18.0449626704835,-65.1741946595148,28.2591785673642));
#33196=CARTESIAN_POINT('Ctrl Pts',(19.6334126095104,-63.9096079063174,28.1480454493728));
#33197=CARTESIAN_POINT('Ctrl Pts',(21.5573777570894,-64.5582302742836,28.0369123313811));
#33198=CARTESIAN_POINT('Ctrl Pts',(22.0559694835154,-66.5264170427403,27.9257792133896));
#33199=CARTESIAN_POINT('Ctrl Pts',(20.6728570166046,-68.0128062140853,27.8146460953981));
#33200=CARTESIAN_POINT('Ctrl Pts',(18.6739193244105,-67.6569959150645,27.7035129774065));
#33201=CARTESIAN_POINT('Ctrl Pts',(17.888662861126,-65.7846377357619,27.5923798594149));
#33202=CARTESIAN_POINT('Ctrl Pts',(19.0357852475963,-64.1093875774479,27.4812467414234));
#33203=CARTESIAN_POINT('Ctrl Pts',(21.065394928907,-64.1645003216707,27.3701136234318));
#33204=CARTESIAN_POINT('Ctrl Pts',(22.1199132331259,-65.8995346167871,27.2589805054402));
#33205=CARTESIAN_POINT('Ctrl Pts',(21.2342035166268,-67.726518783457,27.1478473874487));
#33206=CARTESIAN_POINT('Ctrl Pts',(19.2189021455725,-67.9733250072645,27.0367142694571));
#33207=CARTESIAN_POINT('Ctrl Pts',(17.9184923112052,-66.4140665093775,26.9255811514656));
#33208=CARTESIAN_POINT('Ctrl Pts',(18.5231601679997,-64.4758380560332,26.814448033474));
#33209=CARTESIAN_POINT('Ctrl Pts',(20.4794901123499,-63.9325825814632,26.7033149154825));
#33210=CARTESIAN_POINT('Ctrl Pts',(21.9969715433586,-65.2815089464938,26.5921817974909));
#33211=CARTESIAN_POINT('Ctrl Pts',(21.6867465959066,-67.288026512723,26.4810486794994));
#33212=CARTESIAN_POINT('Ctrl Pts',(19.832743621837,-68.1156916986943,26.3699155615077));
#33213=CARTESIAN_POINT('Ctrl Pts',(18.1318225653926,-67.0069922095504,26.2587824435162));
#33214=CARTESIAN_POINT('Ctrl Pts',(18.1407264484442,-64.9766545323691,26.1476493255247));
#33215=CARTESIAN_POINT('Ctrl Pts',(19.8513197951529,-63.8829214763781,26.0365162075331));
#33216=CARTESIAN_POINT('Ctrl Pts',(21.6979729188376,-64.7268248618362,25.9253830895415));
#33217=CARTESIAN_POINT('Ctrl Pts',(21.9906106740947,-66.7359825655211,25.81424997155));
#33218=CARTESIAN_POINT('Ctrl Pts',(20.4612908701142,-68.0715513800824,25.7031168535584));
#33219=CARTESIAN_POINT('Ctrl Pts',(18.5099236761208,-67.5111322639793,25.5919837355669));
#33220=CARTESIAN_POINT('Ctrl Pts',(17.9220455760523,-65.5677104225445,25.4808506175753));
#33221=CARTESIAN_POINT('Ctrl Pts',(19.2365661510841,-64.0198472713955,25.3697174995837));
#33222=CARTESIAN_POINT('Ctrl Pts',(21.2486684267406,-64.2844772327437,25.2585843815922));
#33223=CARTESIAN_POINT('Ctrl Pts',(22.1202283859708,-66.1188570886621,25.1474512636006));
#33224=CARTESIAN_POINT('Ctrl Pts',(21.0465924302418,-67.8452543356348,25.0363181456091));
#33225=CARTESIAN_POINT('Ctrl Pts',(19.6996852649167,-67.8682605606161,24.9622294002814));
#33226=CARTESIAN_POINT('Ctrl Pts',(19.1702141221325,-67.5923488637343,24.9251850276175));
#33227=CARTESIAN_POINT('Ctrl Pts',(19.5701357431141,-67.6095877486648,36.2244449171475));
#33228=CARTESIAN_POINT('Ctrl Pts',(19.0349325071232,-67.4666537946055,36.1874005444836));
#33229=CARTESIAN_POINT('Ctrl Pts',(18.127631598377,-66.6069908791351,36.1133117991559));
#33230=CARTESIAN_POINT('Ctrl Pts',(18.4746138026192,-64.7528842102888,36.0021786811644));
#33231=CARTESIAN_POINT('Ctrl Pts',(20.2203904348554,-64.0436664636898,35.8910455631728));
#33232=CARTESIAN_POINT('Ctrl Pts',(21.7631193309508,-65.1232793527361,35.7799124451812));
#33233=CARTESIAN_POINT('Ctrl Pts',(21.6928417986657,-67.0061404137184,35.6687793271897));
#33234=CARTESIAN_POINT('Ctrl Pts',(20.0728729391805,-67.9677217333163,35.5576462091981));
#33235=CARTESIAN_POINT('Ctrl Pts',(18.3863763801858,-67.1285775460602,35.4465130912066));
#33236=CARTESIAN_POINT('Ctrl Pts',(18.1766471536642,-65.256408990077,35.335379973215));
#33237=CARTESIAN_POINT('Ctrl Pts',(19.6357646146006,-64.0648572555519,35.2242468552234));
#33238=CARTESIAN_POINT('Ctrl Pts',(21.4282233691483,-64.6443977096884,35.1131137372319));
#33239=CARTESIAN_POINT('Ctrl Pts',(21.9135265503078,-66.4646520881558,35.0019806192403));
#33240=CARTESIAN_POINT('Ctrl Pts',(20.6474895653351,-67.8596318890753,34.8908475012488));
#33241=CARTESIAN_POINT('Ctrl Pts',(18.7888473297796,-67.5526067506278,34.7797143832572));
#33242=CARTESIAN_POINT('Ctrl Pts',(18.0386983418521,-65.8245731185539,34.6685812652657));
#33243=CARTESIAN_POINT('Ctrl Pts',(19.0836105030738,-64.2570979185908,34.5574481472741));
#33244=CARTESIAN_POINT('Ctrl Pts',(20.9672380617522,-64.2847948793711,34.4463150292825));
#33245=CARTESIAN_POINT('Ctrl Pts',(21.9656114461841,-65.8823152891195,34.335181911291));
#33246=CARTESIAN_POINT('Ctrl Pts',(21.1649797840838,-67.5875452715668,34.2240487932994));
#33247=CARTESIAN_POINT('Ctrl Pts',(19.2981128132078,-67.8397913898394,34.1129156753078));
#33248=CARTESIAN_POINT('Ctrl Pts',(18.0736406002369,-66.408187987792,34.0017825573163));
#33249=CARTESIAN_POINT('Ctrl Pts',(18.6122483414602,-64.6029948866662,33.8906494393248));
#33250=CARTESIAN_POINT('Ctrl Pts',(20.4209810165526,-64.0763958440913,33.7795163213331));
#33251=CARTESIAN_POINT('Ctrl Pts',(21.8444152983533,-65.3103550407155,33.6683832033416));
#33252=CARTESIAN_POINT('Ctrl Pts',(21.5797681022636,-67.1755044465377,33.55725008535));
#33253=CARTESIAN_POINT('Ctrl Pts',(19.8692549605973,-67.9647859163373,33.4461169673585));
#33254=CARTESIAN_POINT('Ctrl Pts',(18.278404824725,-66.9558179818571,33.3349838493669));
#33255=CARTESIAN_POINT('Ctrl Pts',(18.2632263547617,-65.0720478099667,33.2238507313754));
#33256=CARTESIAN_POINT('Ctrl Pts',(19.837611483579,-64.0375760061294,33.1127176133838));
#33257=CARTESIAN_POINT('Ctrl Pts',(21.5606209742177,-64.7991918817922,33.0015844953923));
#33258=CARTESIAN_POINT('Ctrl Pts',(21.8552887237877,-66.6598346105587,32.8904513774007));
#33259=CARTESIAN_POINT('Ctrl Pts',(20.4519232099055,-67.9165707329182,32.7793182594091));
#33260=CARTESIAN_POINT('Ctrl Pts',(18.6349397867881,-67.4191858850152,32.6681851414176));
#33261=CARTESIAN_POINT('Ctrl Pts',(18.0673131990514,-65.6229062565376,32.557052023426));
#33262=CARTESIAN_POINT('Ctrl Pts',(19.2685576413527,-64.1717576643402,32.4459189054344));
#33263=CARTESIAN_POINT('Ctrl Pts',(21.1392469195794,-64.3938884166567,32.3347857874429));
#33264=CARTESIAN_POINT('Ctrl Pts',(21.9672525766849,-66.0859957059843,32.2236526694513));
#33265=CARTESIAN_POINT('Ctrl Pts',(20.9947512453016,-67.6993963404374,32.1125195514598));
#33266=CARTESIAN_POINT('Ctrl Pts',(19.1118144211908,-67.757442556534,32.0013864334682));
#33267=CARTESIAN_POINT('Ctrl Pts',(18.0417799974499,-66.2070081726256,31.8902533154767));
#33268=CARTESIAN_POINT('Ctrl Pts',(18.7639855948311,-64.4671117613681,31.7791201974851));
#33269=CARTESIAN_POINT('Ctrl Pts',(20.6174402248758,-64.1301749999996,31.6679870794935));
#33270=CARTESIAN_POINT('Ctrl Pts',(21.9057892589038,-65.5045756742264,31.556853961502));
#33271=CARTESIAN_POINT('Ctrl Pts',(21.4498849520487,-67.3324081911126,31.4457208435104));
#33272=CARTESIAN_POINT('Ctrl Pts',(19.6669888701631,-67.9407682884172,31.3345877255189));
#33273=CARTESIAN_POINT('Ctrl Pts',(18.1888776814945,-66.7728608602669,31.2234546075273));
#33274=CARTESIAN_POINT('Ctrl Pts',(18.368376923802,-64.8976007532933,31.1123214895358));
#33275=CARTESIAN_POINT('Ctrl Pts',(20.0412018255044,-64.0312998269172,31.0011883715442));
#33276=CARTESIAN_POINT('Ctrl Pts',(21.6763171948171,-64.9668307862301,30.8900552535526));
#33277=CARTESIAN_POINT('Ctrl Pts',(21.7772010882313,-66.8479588751294,30.7789221355611));
#33278=CARTESIAN_POINT('Ctrl Pts',(20.2515205957431,-67.9530016261739,30.6677890175695));
#33279=CARTESIAN_POINT('Ctrl Pts',(18.4956385542766,-67.2705804195494,30.556655899578));
#33280=CARTESIAN_POINT('Ctrl Pts',(18.1166073190257,-65.425274003395,30.4455227815864));
#33281=CARTESIAN_POINT('Ctrl Pts',(19.4613311950161,-64.1059794403286,30.3343896635948));
#33282=CARTESIAN_POINT('Ctrl Pts',(21.2990659631253,-64.520167041396,30.2232565456033));
#33283=CARTESIAN_POINT('Ctrl Pts',(21.9478444310442,-66.2887560118356,30.1121234276117));
#33284=CARTESIAN_POINT('Ctrl Pts',(20.8138790092618,-67.7930641149174,30.0009903096202));
#33285=CARTESIAN_POINT('Ctrl Pts',(18.9350194842373,-67.6562893657108,29.8898571916286));
#33286=CARTESIAN_POINT('Ctrl Pts',(18.0308720444635,-66.0036133980917,29.778724073637));
#33287=CARTESIAN_POINT('Ctrl Pts',(18.9289480137178,-64.347630306317,29.6675909556455));
#33288=CARTESIAN_POINT('Ctrl Pts',(20.807292917013,-64.2039609948384,29.5564578376539));
#33289=CARTESIAN_POINT('Ctrl Pts',(21.9467715679183,-65.7040972722901,29.4453247196624));
#33290=CARTESIAN_POINT('Ctrl Pts',(21.3044882556826,-67.4750553727597,29.3341916016708));
#33291=CARTESIAN_POINT('Ctrl Pts',(19.4682859476888,-67.895984738466,29.2230584836793));
#33292=CARTESIAN_POINT('Ctrl Pts',(18.1187292684313,-66.581634246296,29.1119253656877));
#33293=CARTESIAN_POINT('Ctrl Pts',(18.4909856088001,-64.7349491990151,29.0007922476961));
#33294=CARTESIAN_POINT('Ctrl Pts',(20.2443513142224,-64.0460884367099,28.8896591297046));
#33295=CARTESIAN_POINT('Ctrl Pts',(21.774077079295,-65.1455244423375,28.778526011713));
#33296=CARTESIAN_POINT('Ctrl Pts',(21.6800976744022,-67.027010110168,28.6673928937214));
#33297=CARTESIAN_POINT('Ctrl Pts',(20.0484267498987,-67.9685357024486,28.5562597757299));
#33298=CARTESIAN_POINT('Ctrl Pts',(18.3724337578252,-67.1083799390385,28.4451266577383));
#33299=CARTESIAN_POINT('Ctrl Pts',(18.1860534509818,-65.2337912300098,28.3339935397468));
#33300=CARTESIAN_POINT('Ctrl Pts',(19.6598684220231,-64.060466944962,28.2228604217552));
#33301=CARTESIAN_POINT('Ctrl Pts',(21.4449852007115,-64.6622796511569,28.1117273037637));
#33302=CARTESIAN_POINT('Ctrl Pts',(21.9075946495772,-66.4884266727834,28.0005941857721));
#33303=CARTESIAN_POINT('Ctrl Pts',(20.6242983930922,-67.8675463791709,27.8894610677806));
#33304=CARTESIAN_POINT('Ctrl Pts',(18.7696196748325,-67.5374141334743,27.778327949789));
#33305=CARTESIAN_POINT('Ctrl Pts',(18.0410334580049,-65.8001799607068,27.6671948317975));
#33306=CARTESIAN_POINT('Ctrl Pts',(19.1053705235042,-64.2458289529094,27.5560617138058));
#33307=CARTESIAN_POINT('Ctrl Pts',(20.988507700316,-64.2969643305723,27.4449285958143));
#33308=CARTESIAN_POINT('Ctrl Pts',(21.9669237182277,-65.9067849843973,27.3337954778227));
#33309=CARTESIAN_POINT('Ctrl Pts',(21.1451337404002,-67.6019196880712,27.2226623598312));
#33310=CARTESIAN_POINT('Ctrl Pts',(19.2752722742974,-67.8309144449451,27.1115292418396));
#33311=CARTESIAN_POINT('Ctrl Pts',(18.0687101817244,-66.3841842323977,27.0003961238481));
#33312=CARTESIAN_POINT('Ctrl Pts',(18.6297404779621,-64.5858334996156,26.8892630058565));
#33313=CARTESIAN_POINT('Ctrl Pts',(20.4448863566203,-64.081783587906,26.7781298878649));
#33314=CARTESIAN_POINT('Ctrl Pts',(21.852854462098,-65.33336087893,26.6669967698734));
#33315=CARTESIAN_POINT('Ctrl Pts',(21.5650177725607,-67.195072448246,26.5558636518818));
#33316=CARTESIAN_POINT('Ctrl Pts',(19.844814149894,-67.9630068427298,26.4447305338903));
#33317=CARTESIAN_POINT('Ctrl Pts',(18.2666448567006,-66.9343197778498,26.3335974158987));
#33318=CARTESIAN_POINT('Ctrl Pts',(18.2749061659302,-65.0505071430419,26.2224642979072));
#33319=CARTESIAN_POINT('Ctrl Pts',(19.8620497212928,-64.0357064164734,26.1113311799156));
#33320=CARTESIAN_POINT('Ctrl Pts',(21.5754339162483,-64.8187071349992,26.000198061924));
#33321=CARTESIAN_POINT('Ctrl Pts',(21.846952642897,-66.6828683088086,25.8890649439325));
#33322=CARTESIAN_POINT('Ctrl Pts',(20.4280005140077,-67.9220520346501,25.7779318259409));
#33323=CARTESIAN_POINT('Ctrl Pts',(18.6174592348358,-67.4020771439864,25.6667987079494));
#33324=CARTESIAN_POINT('Ctrl Pts',(18.0720070151965,-65.5989078186063,25.5556655899578));
#33325=CARTESIAN_POINT('Ctrl Pts',(19.2916615070531,-64.162750575474,25.4445324719662));
#33326=CARTESIAN_POINT('Ctrl Pts',(21.1585547494963,-64.4082827696205,25.3333993539747));
#33327=CARTESIAN_POINT('Ctrl Pts',(21.9672161271791,-66.1102794317786,25.2222662359831));
#33328=CARTESIAN_POINT('Ctrl Pts',(20.9710621369748,-67.7120863543886,25.1111331179916));
#33329=CARTESIAN_POINT('Ctrl Pts',(19.7213583244171,-67.7334322702853,25.0370443726639));
#33330=CARTESIAN_POINT('Ctrl Pts',(19.2300979593295,-67.4774325188554,25.));
#33331=CARTESIAN_POINT('Ctrl Pts',(18.3361559831984,-65.999055845664,35.3785196366098));
#33332=CARTESIAN_POINT('Ctrl Pts',(18.3350370782603,-65.7833631823591,35.3641397488116));
#33333=CARTESIAN_POINT('Ctrl Pts',(18.3739569960147,-65.5680576617332,35.3497598610133));
#33334=CARTESIAN_POINT('Ctrl Pts',(18.4547882682405,-65.3698451269867,35.335379973215));
#33335=CARTESIAN_POINT('Ctrl Pts',(18.663019640643,-64.8592250785686,35.2983356005511));
#33336=CARTESIAN_POINT('Ctrl Pts',(19.1493921276218,-64.4620411670603,35.2612912278873));
#33337=CARTESIAN_POINT('Ctrl Pts',(19.6913214968691,-64.3600392869955,35.2242468552234));
#33338=CARTESIAN_POINT('Ctrl Pts',(20.2332508661165,-64.2580374069307,35.1872024825596));
#33339=CARTESIAN_POINT('Ctrl Pts',(20.8307371176324,-64.4512175583096,35.1501581098957));
#33340=CARTESIAN_POINT('Ctrl Pts',(21.2103641069169,-64.8511833637436,35.1131137372319));
#33341=CARTESIAN_POINT('Ctrl Pts',(21.5899910962014,-65.2511491691776,35.076069364568));
#33342=CARTESIAN_POINT('Ctrl Pts',(21.7517588232546,-65.8579006286667,35.0390249919042));
#33343=CARTESIAN_POINT('Ctrl Pts',(21.6216365226191,-66.3937729918978,35.0019806192403));
#33344=CARTESIAN_POINT('Ctrl Pts',(21.4915142219835,-66.929645355129,34.9649362465765));
#33345=CARTESIAN_POINT('Ctrl Pts',(21.0695018936593,-67.3946386221021,34.9278918739126));
#33346=CARTESIAN_POINT('Ctrl Pts',(20.5487220235713,-67.5759643991808,34.8908475012488));
#33347=CARTESIAN_POINT('Ctrl Pts',(20.0279421534833,-67.7572901762595,34.8538031285849));
#33348=CARTESIAN_POINT('Ctrl Pts',(19.4083947416314,-67.6549484634436,34.8167587559211));
#33349=CARTESIAN_POINT('Ctrl Pts',(18.9735962043843,-67.3157720016901,34.7797143832572));
#33350=CARTESIAN_POINT('Ctrl Pts',(18.5776806698023,-67.0069272870253,34.7459828010414));
#33351=CARTESIAN_POINT('Ctrl Pts',(18.3349481942213,-66.5017129251968,34.7122512188256));
#33352=CARTESIAN_POINT('Ctrl Pts',(18.3317911996431,-65.9991411289371,34.6785196366098));
#33353=CARTESIAN_POINT('Ctrl Pts',(19.4698297828114,-67.9851743256717,36.));
#33354=CARTESIAN_POINT('Ctrl Pts',(19.4011649893952,-67.9597502983812,36.));
#33355=CARTESIAN_POINT('Ctrl Pts',(19.3342035408141,-67.9304365939153,36.));
#33356=CARTESIAN_POINT('Ctrl Pts',(19.2691343741972,-67.8975272372444,36.));
#33357=CARTESIAN_POINT('Ctrl Pts',(19.2022542736866,-67.8637019833443,36.));
#33358=CARTESIAN_POINT('Ctrl Pts',(19.1373724771277,-67.8260774631159,36.));
#33359=CARTESIAN_POINT('Ctrl Pts',(19.0747253547554,-67.7849282947603,36.));
#33360=CARTESIAN_POINT('Ctrl Pts',(19.0217926342618,-67.7501599391738,36.));
#33361=CARTESIAN_POINT('Ctrl Pts',(18.9704556141999,-67.7128742354079,36.));
#33362=CARTESIAN_POINT('Ctrl Pts',(18.9208796153568,-67.6732188234994,36.));
#33363=CARTESIAN_POINT('Ctrl Pts',(18.8988499701712,-67.6555975011978,36.));
#33364=CARTESIAN_POINT('Ctrl Pts',(18.8771683538016,-67.6375080850151,36.));
#33365=CARTESIAN_POINT('Ctrl Pts',(18.8558508253114,-67.6189628052533,36.));
#33366=CARTESIAN_POINT('Ctrl Pts',(18.844138241103,-67.6087733899569,36.));
#33367=CARTESIAN_POINT('Ctrl Pts',(18.8325355847645,-67.5984463527787,36.));
#33368=CARTESIAN_POINT('Ctrl Pts',(18.8210456541305,-67.5879836806034,36.));
#33369=CARTESIAN_POINT('Ctrl Pts',(18.8104521112012,-67.5783372544957,36.));
#33370=CARTESIAN_POINT('Ctrl Pts',(18.7999529576494,-67.5685740155973,36.));
#33371=CARTESIAN_POINT('Ctrl Pts',(18.7895662739712,-67.5587109766458,36.));
#33372=CARTESIAN_POINT('Ctrl Pts',(18.736481497238,-67.5083024692848,36.));
#33373=CARTESIAN_POINT('Ctrl Pts',(18.6862367142759,-67.45520556261,36.));
#33374=CARTESIAN_POINT('Ctrl Pts',(18.6390505925823,-67.399679719805,36.));
#33375=CARTESIAN_POINT('Ctrl Pts',(18.5922306356017,-67.3445847580211,36.));
#33376=CARTESIAN_POINT('Ctrl Pts',(18.5484215452298,-67.2870975275965,36.));
#33377=CARTESIAN_POINT('Ctrl Pts',(18.507881729457,-67.2274472583178,36.));
#33378=CARTESIAN_POINT('Ctrl Pts',(18.4741932913828,-67.17787810354,36.));
#33379=CARTESIAN_POINT('Ctrl Pts',(18.442763110747,-67.1268145999806,36.));
#33380=CARTESIAN_POINT('Ctrl Pts',(18.4137670774186,-67.0743818157429,36.));
#33381=CARTESIAN_POINT('Ctrl Pts',(18.4016609056866,-67.0524905355397,36.));
#33382=CARTESIAN_POINT('Ctrl Pts',(18.3899793657611,-67.0303605291398,36.));
#33383=CARTESIAN_POINT('Ctrl Pts',(18.3787367001908,-67.0080008158944,36.));
#33384=CARTESIAN_POINT('Ctrl Pts',(18.3735358722236,-66.9976572704731,36.));
#33385=CARTESIAN_POINT('Ctrl Pts',(18.3684289741711,-66.987264568668,36.));
#33386=CARTESIAN_POINT('Ctrl Pts',(18.363417481184,-66.9768236053222,36.));
#33387=CARTESIAN_POINT('Ctrl Pts',(18.3581854927908,-66.9659232610176,36.));
#33388=CARTESIAN_POINT('Ctrl Pts',(18.3530610988599,-66.9549777676102,36.));
#33389=CARTESIAN_POINT('Ctrl Pts',(18.3480473578998,-66.9439924325212,36.));
#33390=CARTESIAN_POINT('Ctrl Pts',(18.3195069605931,-66.8814591204733,36.));
#33391=CARTESIAN_POINT('Ctrl Pts',(18.2945275345026,-66.8175927373651,36.));
#33392=CARTESIAN_POINT('Ctrl Pts',(18.2733325397259,-66.752597734286,36.));
#33393=CARTESIAN_POINT('Ctrl Pts',(18.2541300624259,-66.6937128379039,36.));
#33394=CARTESIAN_POINT('Ctrl Pts',(18.2380342438875,-66.6339009498019,36.));
#33395=CARTESIAN_POINT('Ctrl Pts',(18.2252479596501,-66.5733092869319,36.));
#33396=CARTESIAN_POINT('Ctrl Pts',(18.2101154548975,-66.5015993507748,36.));
#33397=CARTESIAN_POINT('Ctrl Pts',(18.1996178813496,-66.4287956961599,36.));
#33398=CARTESIAN_POINT('Ctrl Pts',(18.1936800996947,-66.3553214263371,36.));
#33399=CARTESIAN_POINT('Ctrl Pts',(18.1923732777051,-66.3391507759068,36.));
#33400=CARTESIAN_POINT('Ctrl Pts',(18.1912875458271,-66.3229477241296,36.));
#33401=CARTESIAN_POINT('Ctrl Pts',(18.1904224723119,-66.3067169458811,36.));
#33402=CARTESIAN_POINT('Ctrl Pts',(18.1895271437582,-66.2899185131946,36.));
#33403=CARTESIAN_POINT('Ctrl Pts',(18.1888681680866,-66.2730841862021,36.));
#33404=CARTESIAN_POINT('Ctrl Pts',(18.1884456276216,-66.256253422113,36.));
#33405=CARTESIAN_POINT('Ctrl Pts',(18.1867243886032,-66.1876924906622,36.));
#33406=CARTESIAN_POINT('Ctrl Pts',(18.1889147565045,-66.1191039788408,36.));
#33407=CARTESIAN_POINT('Ctrl Pts',(18.1948961467264,-66.0508262139634,36.));
#33408=CARTESIAN_POINT('Ctrl Pts',(18.2008763007651,-65.9825625601576,36.));
#33409=CARTESIAN_POINT('Ctrl Pts',(18.2106463639563,-65.9146084532637,36.));
#33410=CARTESIAN_POINT('Ctrl Pts',(18.2241354315071,-65.8473170438901,36.));
#33411=CARTESIAN_POINT('Ctrl Pts',(18.2338954237845,-65.7986284571252,36.));
#33412=CARTESIAN_POINT('Ctrl Pts',(18.2456034473503,-65.7502870727337,36.));
#33413=CARTESIAN_POINT('Ctrl Pts',(18.2592468469421,-65.7024363115996,36.));
#33414=CARTESIAN_POINT('Ctrl Pts',(18.2694831958018,-65.6665349161389,36.));
#33415=CARTESIAN_POINT('Ctrl Pts',(18.2808092514107,-65.630909856111,36.));
#33416=CARTESIAN_POINT('Ctrl Pts',(18.2932235838799,-65.5956258810508,36.));
#33417=CARTESIAN_POINT('Ctrl Pts',(18.297353127888,-65.5838889046042,36.));
#33418=CARTESIAN_POINT('Ctrl Pts',(18.3015998970195,-65.572198863249,36.));
#33419=CARTESIAN_POINT('Ctrl Pts',(18.3059632462308,-65.5605583181236,36.));
#33420=CARTESIAN_POINT('Ctrl Pts',(18.3290871983339,-65.4988682275758,36.));
#33421=CARTESIAN_POINT('Ctrl Pts',(18.3554837360288,-65.4385616710145,36.));
#33422=CARTESIAN_POINT('Ctrl Pts',(18.385102864326,-65.3799727413706,36.));
#33423=CARTESIAN_POINT('Ctrl Pts',(18.4059351916682,-65.338764784515,36.));
#33424=CARTESIAN_POINT('Ctrl Pts',(18.4283625495674,-65.2984070455804,36.));
#33425=CARTESIAN_POINT('Ctrl Pts',(18.4523779441861,-65.2590271139576,36.));
#33426=CARTESIAN_POINT('Ctrl Pts',(18.460090964352,-65.2463794680805,36.));
#33427=CARTESIAN_POINT('Ctrl Pts',(18.4679689477642,-65.233831076664,36.));
#33428=CARTESIAN_POINT('Ctrl Pts',(18.4760083383501,-65.2213918011997,36.));
#33429=CARTESIAN_POINT('Ctrl Pts',(18.5102528434667,-65.1684055918931,36.));
#33430=CARTESIAN_POINT('Ctrl Pts',(18.5473531093338,-65.1175031736617,36.));
#33431=CARTESIAN_POINT('Ctrl Pts',(18.5872748982222,-65.0689997700819,36.));
#33432=CARTESIAN_POINT('Ctrl Pts',(18.6240617329213,-65.0243052125604,36.));
#33433=CARTESIAN_POINT('Ctrl Pts',(18.6632449424928,-64.9816475926941,36.));
#33434=CARTESIAN_POINT('Ctrl Pts',(18.7048191776161,-64.9413064478025,36.));
#33435=CARTESIAN_POINT('Ctrl Pts',(18.7126375272136,-64.9337199901564,36.));
#33436=CARTESIAN_POINT('Ctrl Pts',(18.7205404900226,-64.9262155594354,36.));
#33437=CARTESIAN_POINT('Ctrl Pts',(18.7285264739143,-64.9187938215857,36.));
#33438=CARTESIAN_POINT('Origin',(20.,-66.,30.));
#33439=CARTESIAN_POINT('Origin',(-20.,-66.,25.));
#33440=CARTESIAN_POINT('Ctrl Pts',(-20.7699020406704,-67.4774325188554,
25.));
#33441=CARTESIAN_POINT('Ctrl Pts',(-20.7181608035629,-67.5125051433483,
25.));
#33442=CARTESIAN_POINT('Ctrl Pts',(-20.6644430822213,-67.5443226803472,
25.));
#33443=CARTESIAN_POINT('Ctrl Pts',(-20.6090801759931,-67.5729491720382,
25.));
#33444=CARTESIAN_POINT('Ctrl Pts',(-20.5739700098743,-67.5911035816807,
25.));
#33445=CARTESIAN_POINT('Ctrl Pts',(-20.5381972786393,-67.6079739470072,
25.));
#33446=CARTESIAN_POINT('Ctrl Pts',(-20.5018388806471,-67.6235693893572,
25.));
#33447=CARTESIAN_POINT('Ctrl Pts',(-20.477053808413,-67.6342006103821,25.));
#33448=CARTESIAN_POINT('Ctrl Pts',(-20.4519964598586,-67.6442392598381,
25.));
#33449=CARTESIAN_POINT('Ctrl Pts',(-20.4266899529795,-67.6536866428541,
25.));
#33450=CARTESIAN_POINT('Ctrl Pts',(-20.413200618616,-67.6587224587006,25.));
#33451=CARTESIAN_POINT('Ctrl Pts',(-20.3996405377501,-67.6635901036932,
25.));
#33452=CARTESIAN_POINT('Ctrl Pts',(-20.386026916268,-67.6682852533056,25.));
#33453=CARTESIAN_POINT('Ctrl Pts',(-20.3236625333886,-67.6897938657264,
25.));
#33454=CARTESIAN_POINT('Ctrl Pts',(-20.2601068487493,-67.7077128062917,
25.));
#33455=CARTESIAN_POINT('Ctrl Pts',(-20.1957097546859,-67.7220886184591,
25.));
#33456=CARTESIAN_POINT('Ctrl Pts',(-20.1492572977333,-67.7324585242068,
25.));
#33457=CARTESIAN_POINT('Ctrl Pts',(-20.1023661244431,-67.7409839821677,
25.));
#33458=CARTESIAN_POINT('Ctrl Pts',(-20.0551584518849,-67.7476684316844,
25.));
#33459=CARTESIAN_POINT('Ctrl Pts',(-20.0422593587017,-67.7494949004027,
25.));
#33460=CARTESIAN_POINT('Ctrl Pts',(-20.0293366022274,-67.7511838474356,
25.));
#33461=CARTESIAN_POINT('Ctrl Pts',(-20.0163926091019,-67.7527351822321,
25.));
#33462=CARTESIAN_POINT('Ctrl Pts',(-20.0030616559028,-67.7543328941104,
25.));
#33463=CARTESIAN_POINT('Ctrl Pts',(-19.9897160980323,-67.7557836532261,
25.));
#33464=CARTESIAN_POINT('Ctrl Pts',(-19.9763641937448,-67.7570873827579,
25.));
#33465=CARTESIAN_POINT('Ctrl Pts',(-19.9088330185891,-67.7636813775523,
25.));
#33466=CARTESIAN_POINT('Ctrl Pts',(-19.8410981608417,-67.7665229814955,
25.));
#33467=CARTESIAN_POINT('Ctrl Pts',(-19.7735142959518,-67.7656601451573,
25.));
#33468=CARTESIAN_POINT('Ctrl Pts',(-19.704951841588,-67.7647848152668,25.));
#33469=CARTESIAN_POINT('Ctrl Pts',(-19.63654377446,-67.7600973242924,25.));
#33470=CARTESIAN_POINT('Ctrl Pts',(-19.5686389092575,-67.7515994414432,
25.));
#33471=CARTESIAN_POINT('Ctrl Pts',(-19.5265710026273,-67.7463348975672,
25.));
#33472=CARTESIAN_POINT('Ctrl Pts',(-19.4846958553342,-67.7396069714499,
25.));
#33473=CARTESIAN_POINT('Ctrl Pts',(-19.4430950268279,-67.7314061394558,
25.));
#33474=CARTESIAN_POINT('Ctrl Pts',(-19.4090314673628,-67.7246911403001,
25.));
#33475=CARTESIAN_POINT('Ctrl Pts',(-19.3751517890293,-67.716988473764,25.));
#33476=CARTESIAN_POINT('Ctrl Pts',(-19.3415011106365,-67.7082889292452,
25.));
#33477=CARTESIAN_POINT('Ctrl Pts',(-19.3277178592572,-67.7047256129997,
25.));
#33478=CARTESIAN_POINT('Ctrl Pts',(-19.3139705632122,-67.7009941660984,
25.));
#33479=CARTESIAN_POINT('Ctrl Pts',(-19.3002855806312,-67.6971007967711,
25.));
#33480=CARTESIAN_POINT('Ctrl Pts',(-19.232490274151,-67.6778130727844,25.));
#33481=CARTESIAN_POINT('Ctrl Pts',(-19.1661045678635,-67.6545261552985,
25.));
#33482=CARTESIAN_POINT('Ctrl Pts',(-19.1014911923583,-67.6272587556,25.));
#33483=CARTESIAN_POINT('Ctrl Pts',(-19.0943244150679,-67.6242343139979,
25.));
#33484=CARTESIAN_POINT('Ctrl Pts',(-19.0871794343997,-67.6211608492454,
25.));
#33485=CARTESIAN_POINT('Ctrl Pts',(-19.0800567411892,-67.6180383475084,
25.));
#33486=CARTESIAN_POINT('Ctrl Pts',(-19.0183041427041,-67.5909667623182,
25.));
#33487=CARTESIAN_POINT('Ctrl Pts',(-18.958225984176,-67.5602135819053,25.));
#33488=CARTESIAN_POINT('Ctrl Pts',(-18.8999642015444,-67.5260890069827,
25.));
#33489=CARTESIAN_POINT('Ctrl Pts',(-18.8372883233669,-67.489379047141,25.));
#33490=CARTESIAN_POINT('Ctrl Pts',(-18.7767134702701,-67.4487674765275,
25.));
#33491=CARTESIAN_POINT('Ctrl Pts',(-18.7184362286254,-67.404579398372,25.));
#33492=CARTESIAN_POINT('Ctrl Pts',(-18.7079109252492,-67.3965987027338,
25.));
#33493=CARTESIAN_POINT('Ctrl Pts',(-18.69746064122,-67.3885011964254,25.));
#33494=CARTESIAN_POINT('Ctrl Pts',(-18.6870866397008,-67.3802886058017,
25.));
#33495=CARTESIAN_POINT('Ctrl Pts',(-18.6779106450409,-67.3730244187311,
25.));
#33496=CARTESIAN_POINT('Ctrl Pts',(-18.6688013314437,-67.3656757127138,
25.));
#33497=CARTESIAN_POINT('Ctrl Pts',(-18.6597613497716,-67.3582457843923,
25.));
#33498=CARTESIAN_POINT('Ctrl Pts',(-18.6048581342928,-67.3131210296724,
25.));
#33499=CARTESIAN_POINT('Ctrl Pts',(-18.5524870449414,-67.2649855309608,
25.));
#33500=CARTESIAN_POINT('Ctrl Pts',(-18.5027980990966,-67.2141892911126,
25.));
#33501=CARTESIAN_POINT('Ctrl Pts',(-18.4520613983228,-67.1623219476261,
25.));
#33502=CARTESIAN_POINT('Ctrl Pts',(-18.404120381723,-67.1076799285913,25.));
#33503=CARTESIAN_POINT('Ctrl Pts',(-18.3591549660204,-67.0505845582255,
25.));
#33504=CARTESIAN_POINT('Ctrl Pts',(-18.3139167893624,-66.9931428463985,
25.));
#33505=CARTESIAN_POINT('Ctrl Pts',(-18.2716896355437,-66.9332171999082,
25.));
#33506=CARTESIAN_POINT('Ctrl Pts',(-18.2326886678192,-66.8710932841069,
25.));
#33507=CARTESIAN_POINT('Ctrl Pts',(-18.2230616236579,-66.8557585445919,
25.));
#33508=CARTESIAN_POINT('Ctrl Pts',(-18.21363133674,-66.8402896962556,25.));
#33509=CARTESIAN_POINT('Ctrl Pts',(-18.2044014277785,-66.8246907301826,
25.));
#33510=CARTESIAN_POINT('Ctrl Pts',(-18.1971517956968,-66.8124385221321,
25.));
#33511=CARTESIAN_POINT('Ctrl Pts',(-18.1900250445996,-66.8001044895158,
25.));
#33512=CARTESIAN_POINT('Ctrl Pts',(-18.1830333944425,-66.7877096451503,
25.));
#33513=CARTESIAN_POINT('Ctrl Pts',(-18.1460181911873,-66.7220888441667,
25.));
#33514=CARTESIAN_POINT('Ctrl Pts',(-18.1127170684062,-66.6546510927272,
25.));
#33515=CARTESIAN_POINT('Ctrl Pts',(-18.0833107587068,-66.5857427136206,
25.));
#33516=CARTESIAN_POINT('Ctrl Pts',(-18.0538723748317,-66.5167591744726,
25.));
#33517=CARTESIAN_POINT('Ctrl Pts',(-18.0283365400255,-66.4463009685666,
25.));
#33518=CARTESIAN_POINT('Ctrl Pts',(-18.0069203162448,-66.3746778418095,
25.));
#33519=CARTESIAN_POINT('Ctrl Pts',(-17.9859913237923,-66.3046841821113,
25.));
#33520=CARTESIAN_POINT('Ctrl Pts',(-17.968996070436,-66.2335771265626,25.));
#33521=CARTESIAN_POINT('Ctrl Pts',(-17.956180742014,-66.1616225466294,25.));
#33522=CARTESIAN_POINT('Ctrl Pts',(-17.9534318997022,-66.1461885454602,
25.));
#33523=CARTESIAN_POINT('Ctrl Pts',(-17.9508755507278,-66.1307154913356,
25.));
#33524=CARTESIAN_POINT('Ctrl Pts',(-17.9485144323922,-66.1152059238131,
25.));
#33525=CARTESIAN_POINT('Ctrl Pts',(-17.94650124174,-66.101981802054,25.));
#33526=CARTESIAN_POINT('Ctrl Pts',(-17.9446299860387,-66.0887311345142,
25.));
#33527=CARTESIAN_POINT('Ctrl Pts',(-17.9428998377409,-66.0754556195432,
25.));
#33528=CARTESIAN_POINT('Ctrl Pts',(-18.1825721112406,-65.0413794120407,
25.));
#33529=CARTESIAN_POINT('Ctrl Pts',(-18.2234186022369,-64.9788996288608,
25.));
#33530=CARTESIAN_POINT('Ctrl Pts',(-18.2678617752615,-64.9189705657672,
25.));
#33531=CARTESIAN_POINT('Ctrl Pts',(-18.3155727832729,-64.8617419967287,
25.));
#33532=CARTESIAN_POINT('Ctrl Pts',(-18.3620323341325,-64.8060145299515,
25.));
#33533=CARTESIAN_POINT('Ctrl Pts',(-18.4115915340684,-64.7528475406059,
25.));
#33534=CARTESIAN_POINT('Ctrl Pts',(-18.4639728032933,-64.7024169935917,
25.));
#33535=CARTESIAN_POINT('Ctrl Pts',(-18.4756644727561,-64.6911607316637,
25.));
#33536=CARTESIAN_POINT('Ctrl Pts',(-18.4874984029645,-64.6800395001903,
25.));
#33537=CARTESIAN_POINT('Ctrl Pts',(-18.4994665220206,-64.6690601964525,
25.));
#33538=CARTESIAN_POINT('Ctrl Pts',(-18.5543876810387,-64.6186766663706,
25.));
#33539=CARTESIAN_POINT('Ctrl Pts',(-18.6120225665561,-64.5713776148131,
25.));
#33540=CARTESIAN_POINT('Ctrl Pts',(-18.6720550336875,-64.5273355298405,
25.));
#33541=CARTESIAN_POINT('Ctrl Pts',(-18.7141995014743,-64.4964167567151,
25.));
#33542=CARTESIAN_POINT('Ctrl Pts',(-18.7575262835589,-64.4671040519447,
25.));
#33543=CARTESIAN_POINT('Ctrl Pts',(-18.8019313225172,-64.4394714970494,
25.));
#33544=CARTESIAN_POINT('Ctrl Pts',(-18.8188067446915,-64.4289701881765,
25.));
#33545=CARTESIAN_POINT('Ctrl Pts',(-18.8358379234656,-64.4187116654628,
25.));
#33546=CARTESIAN_POINT('Ctrl Pts',(-18.853019222819,-64.4087004822027,25.));
#33547=CARTESIAN_POINT('Ctrl Pts',(-18.8694039161204,-64.3991534646037,
25.));
#33548=CARTESIAN_POINT('Ctrl Pts',(-18.8859304480109,-64.3898286464703,
25.));
#33549=CARTESIAN_POINT('Ctrl Pts',(-18.9025643388043,-64.3807458845255,
25.));
#33550=CARTESIAN_POINT('Ctrl Pts',(-18.9662812680801,-64.3459539222805,
25.));
#33551=CARTESIAN_POINT('Ctrl Pts',(-19.0316371535594,-64.3146691113732,
25.));
#33552=CARTESIAN_POINT('Ctrl Pts',(-19.0983402957666,-64.2870530879642,
25.));
#33553=CARTESIAN_POINT('Ctrl Pts',(-19.1636110961765,-64.2600300738692,
25.));
#33554=CARTESIAN_POINT('Ctrl Pts',(-19.2301728387105,-64.2365198225598,
25.));
#33555=CARTESIAN_POINT('Ctrl Pts',(-19.2977608179252,-64.216722038388,25.));
#33556=CARTESIAN_POINT('Ctrl Pts',(-19.3638664769608,-64.1973584535415,
25.));
#33557=CARTESIAN_POINT('Ctrl Pts',(-19.4309546138826,-64.1815461688934,
25.));
#33558=CARTESIAN_POINT('Ctrl Pts',(-19.4987736270454,-64.1695206205673,
25.));
#33559=CARTESIAN_POINT('Ctrl Pts',(-19.5208338248684,-64.1656089450263,
25.));
#33560=CARTESIAN_POINT('Ctrl Pts',(-19.5429712759434,-64.162098331058,25.));
#33561=CARTESIAN_POINT('Ctrl Pts',(-19.5651770267509,-64.1589980551018,
25.));
#33562=CARTESIAN_POINT('Ctrl Pts',(-19.5776615166783,-64.1572550217641,
25.));
#33563=CARTESIAN_POINT('Ctrl Pts',(-19.5901688804906,-64.155641648664,25.));
#33564=CARTESIAN_POINT('Ctrl Pts',(-19.6026798229647,-64.1541614637293,
25.));
#33565=CARTESIAN_POINT('Ctrl Pts',(-19.6705104535392,-64.1461363387077,
25.));
#33566=CARTESIAN_POINT('Ctrl Pts',(-19.7385646210674,-64.1420044342446,
25.));
#33567=CARTESIAN_POINT('Ctrl Pts',(-19.8065966031785,-64.1419437913522,
25.));
#33568=CARTESIAN_POINT('Ctrl Pts',(-19.8163935407639,-64.1419350584796,
25.));
#33569=CARTESIAN_POINT('Ctrl Pts',(-19.8261900120765,-64.1420108411578,
25.));
#33570=CARTESIAN_POINT('Ctrl Pts',(-19.8359852738992,-64.1421717610483,
25.));
#33571=CARTESIAN_POINT('Ctrl Pts',(-19.9053495120193,-64.1433113003285,
25.));
#33572=CARTESIAN_POINT('Ctrl Pts',(-19.9746545558373,-64.1487161231621,
25.));
#33573=CARTESIAN_POINT('Ctrl Pts',(-20.0435753974168,-64.1582130010768,
25.));
#33574=CARTESIAN_POINT('Ctrl Pts',(-20.107870675276,-64.1670725040998,25.));
#33575=CARTESIAN_POINT('Ctrl Pts',(-20.1718321045596,-64.1794941475947,
25.));
#33576=CARTESIAN_POINT('Ctrl Pts',(-20.2351753108018,-64.1953717359853,
25.));
#33577=CARTESIAN_POINT('Ctrl Pts',(-20.2490399437352,-64.1988470405675,
25.));
#33578=CARTESIAN_POINT('Ctrl Pts',(-20.2628748598245,-64.2024880266852,
25.));
#33579=CARTESIAN_POINT('Ctrl Pts',(-20.2766768992135,-64.2062937588479,
25.));
#33580=CARTESIAN_POINT('Ctrl Pts',(-20.2877373262727,-64.209343527205,25.));
#33581=CARTESIAN_POINT('Ctrl Pts',(-20.298776094781,-64.2124990316602,25.));
#33582=CARTESIAN_POINT('Ctrl Pts',(-20.309778523466,-64.2157556651497,25.));
#33583=CARTESIAN_POINT('Ctrl Pts',(-20.3753407640279,-64.2351615794598,
25.));
#33584=CARTESIAN_POINT('Ctrl Pts',(-20.4397366338522,-64.2581874947932,
25.));
#33585=CARTESIAN_POINT('Ctrl Pts',(-20.5026636727024,-64.2846513912406,
25.));
#33586=CARTESIAN_POINT('Ctrl Pts',(-20.5652993520049,-64.3109927567531,
25.));
#33587=CARTESIAN_POINT('Ctrl Pts',(-20.6264806629052,-64.3407410428595,
25.));
#33588=CARTESIAN_POINT('Ctrl Pts',(-20.6858795340413,-64.3737582968461,
25.));
#33589=CARTESIAN_POINT('Ctrl Pts',(-20.744005682146,-64.4060680993479,25.));
#33590=CARTESIAN_POINT('Ctrl Pts',(-20.800425628206,-64.4415089864798,25.));
#33591=CARTESIAN_POINT('Ctrl Pts',(-20.8547920034067,-64.4799810839263,
25.));
#33592=CARTESIAN_POINT('Ctrl Pts',(-20.8662884771014,-64.4881165068719,
25.));
#33593=CARTESIAN_POINT('Ctrl Pts',(-20.8776929569316,-64.4963875608038,
25.));
#33594=CARTESIAN_POINT('Ctrl Pts',(-20.8890018799099,-64.5047934300188,
25.));
#33595=CARTESIAN_POINT('Ctrl Pts',(-20.8996330286824,-64.5126955128571,
25.));
#33596=CARTESIAN_POINT('Ctrl Pts',(-20.9101809631529,-64.5207178472751,
25.));
#33597=CARTESIAN_POINT('Ctrl Pts',(-20.9206261440524,-64.5288464944984,
25.));
#33598=CARTESIAN_POINT('Ctrl Pts',(-20.9721935855059,-64.5689773015968,
25.));
#33599=CARTESIAN_POINT('Ctrl Pts',(-21.0213544520126,-64.6117655949196,
25.));
#33600=CARTESIAN_POINT('Ctrl Pts',(-21.067817662843,-64.6570793623473,25.));
#33601=CARTESIAN_POINT('Ctrl Pts',(-21.1133972238304,-64.7015313403558,
25.));
#33602=CARTESIAN_POINT('Ctrl Pts',(-21.1563813453372,-64.7484143078876,
25.));
#33603=CARTESIAN_POINT('Ctrl Pts',(-21.1964527232528,-64.7976294036877,
25.));
#33604=CARTESIAN_POINT('Ctrl Pts',(-21.2352229728486,-64.8452464722117,
25.));
#33605=CARTESIAN_POINT('Ctrl Pts',(-21.2712669040832,-64.8950472509739,
25.));
#33606=CARTESIAN_POINT('Ctrl Pts',(-21.3042504633418,-64.9469575622361,
25.));
#33607=CARTESIAN_POINT('Ctrl Pts',(-21.3097028197845,-64.9555386106862,
25.));
#33608=CARTESIAN_POINT('Ctrl Pts',(-21.3150714360615,-64.9641773281828,
25.));
#33609=CARTESIAN_POINT('Ctrl Pts',(-21.3203546654043,-64.9728734055941,
25.));
#33610=CARTESIAN_POINT('Ctrl Pts',(-21.3260102500976,-64.9821823715897,
25.));
#33611=CARTESIAN_POINT('Ctrl Pts',(-21.3315679871567,-64.9915570687347,
25.));
#33612=CARTESIAN_POINT('Ctrl Pts',(-21.3370274731509,-65.0009958365548,
25.));
#33613=CARTESIAN_POINT('Origin',(-20.,-66.,37.5459252805377));
#33614=CARTESIAN_POINT('Ctrl Pts',(-22.0565720193282,-65.9985037223956,
35.7959252805377));
#33615=CARTESIAN_POINT('Ctrl Pts',(-22.0573889661773,-65.9003307564159,
35.7905876687522));
#33616=CARTESIAN_POINT('Ctrl Pts',(-22.0063638909344,-65.1216410352954,
35.7482056843029));
#33617=CARTESIAN_POINT('Ctrl Pts',(-21.0114092448251,-63.7918186839967,
35.6687793271897));
#33618=CARTESIAN_POINT('Ctrl Pts',(-18.6935440716095,-63.9528112405962,
35.5576462091981));
#33619=CARTESIAN_POINT('Ctrl Pts',(-17.5714219214042,-65.9871397838458,
35.4465130912065));
#33620=CARTESIAN_POINT('Ctrl Pts',(-18.6720184117364,-68.0334048867885,
35.335379973215));
#33621=CARTESIAN_POINT('Ctrl Pts',(-20.9880417410518,-68.218534353231,35.2242468552234));
#33622=CARTESIAN_POINT('Ctrl Pts',(-22.0019739647035,-66.8931862309832,
35.144428624331));
#33623=CARTESIAN_POINT('Ctrl Pts',(-22.0572805505537,-66.1070372200823,
35.1016547661024));
#33624=CARTESIAN_POINT('Ctrl Pts',(-22.0563749241962,-66.0016062120012,
35.0959252805377));
#33625=CARTESIAN_POINT('Ctrl Pts',(-22.0526726878338,-66.0023207051531,
35.8540747194623));
#33626=CARTESIAN_POINT('Ctrl Pts',(-22.0491245215623,-65.5321720585535,
35.8286277343138));
#33627=CARTESIAN_POINT('Ctrl Pts',(-21.656632320464,-64.370597952911,35.7661363765015));
#33628=CARTESIAN_POINT('Ctrl Pts',(-19.7281828815708,-63.5871681688473,
35.6666006460254));
#33629=CARTESIAN_POINT('Ctrl Pts',(-17.825468300226,-64.9187027300962,35.5554675280337));
#33630=CARTESIAN_POINT('Ctrl Pts',(-17.9121446998427,-67.2409164611445,
35.4443344100422));
#33631=CARTESIAN_POINT('Ctrl Pts',(-19.9101226099192,-68.4268768260922,
35.3332012920507));
#33632=CARTESIAN_POINT('Ctrl Pts',(-21.7210101198393,-67.525839720907,35.2364480618573));
#33633=CARTESIAN_POINT('Ctrl Pts',(-22.0499160744514,-66.4181209330382,
35.1767392043279));
#33634=CARTESIAN_POINT('Ctrl Pts',(-22.0520911128174,-65.9988355264336,
35.1540747194623));
#33635=CARTESIAN_POINT('Ctrl Pts',(-18.7309291201477,-64.9206413469514,
36.));
#33636=CARTESIAN_POINT('Ctrl Pts',(-18.372032101712,-65.3426194852432,35.9629556273362));
#33637=CARTESIAN_POINT('Ctrl Pts',(-18.1147588818617,-66.5657419043161,
35.8888668820084));
#33638=CARTESIAN_POINT('Ctrl Pts',(-19.4547380737757,-67.893353926766,35.7777337640169));
#33639=CARTESIAN_POINT('Ctrl Pts',(-21.2940072704514,-67.4836982885462,
35.6666006460253));
#33640=CARTESIAN_POINT('Ctrl Pts',(-21.9488058964948,-65.7182472190985,
35.5554675280338));
#33641=CARTESIAN_POINT('Ctrl Pts',(-20.8200548981038,-64.2095972393422,
35.4443344100422));
#33642=CARTESIAN_POINT('Ctrl Pts',(-18.9407200016067,-64.3401306858903,
35.3332012920506));
#33643=CARTESIAN_POINT('Ctrl Pts',(-18.0308986110522,-65.9895728822909,
35.2220681740591));
#33644=CARTESIAN_POINT('Ctrl Pts',(-18.92326690544,-67.648693291831,35.1109350560675));
#33645=CARTESIAN_POINT('Ctrl Pts',(-20.8011084271042,-67.7987970470776,
34.999801938076));
#33646=CARTESIAN_POINT('Ctrl Pts',(-21.9457416179595,-66.3026048808017,
34.8886688200844));
#33647=CARTESIAN_POINT('Ctrl Pts',(-21.309556683593,-64.5294397965287,34.7775357020928));
#33648=CARTESIAN_POINT('Ctrl Pts',(-19.47481333332,-64.1021978279347,34.6664025841013));
#33649=CARTESIAN_POINT('Ctrl Pts',(-18.12074179018,-65.4118948223318,34.5552694661097));
#33650=CARTESIAN_POINT('Ctrl Pts',(-18.4866411777649,-67.2598509704003,
34.4441363481182));
#33651=CARTESIAN_POINT('Ctrl Pts',(-20.2376261998072,-67.9547408460341,
34.3330032301266));
#33652=CARTESIAN_POINT('Ctrl Pts',(-21.7711263332307,-66.8605755017373,
34.2218701121351));
#33653=CARTESIAN_POINT('Ctrl Pts',(-21.6836219545264,-64.9787773153848,
34.1107369941435));
#33654=CARTESIAN_POINT('Ctrl Pts',(-20.0552004868468,-64.0316424608183,
33.999603876152));
#33655=CARTESIAN_POINT('Ctrl Pts',(-18.3762573656889,-64.886025831751,33.8884707581604));
#33656=CARTESIAN_POINT('Ctrl Pts',(-18.1834274109556,-66.7599622412461,
33.7773376401689));
#33657=CARTESIAN_POINT('Ctrl Pts',(-19.6531961905118,-67.9383512785846,
33.6662045221772));
#33658=CARTESIAN_POINT('Ctrl Pts',(-21.4403734659769,-67.3426849415994,
33.5550714041857));
#33659=CARTESIAN_POINT('Ctrl Pts',(-21.9092642531335,-65.5181404941846,
33.4439382861941));
#33660=CARTESIAN_POINT('Ctrl Pts',(-20.6307212477628,-64.134612834461,33.3328051682026));
#33661=CARTESIAN_POINT('Ctrl Pts',(-18.7749173315688,-64.4583609284768,
33.221672050211));
#33662=CARTESIAN_POINT('Ctrl Pts',(-18.0403572922691,-66.1930777796175,
33.1105389322195));
#33663=CARTESIAN_POINT('Ctrl Pts',(-19.0993393898891,-67.751082247112,32.9994058142279));
#33664=CARTESIAN_POINT('Ctrl Pts',(-20.9826415275293,-67.7064273202608,
32.8882726962363));
#33665=CARTESIAN_POINT('Ctrl Pts',(-21.9665914627858,-66.0999829455134,
32.7771395782448));
#33666=CARTESIAN_POINT('Ctrl Pts',(-21.1506394870126,-64.4020302437763,
32.6660064602533));
#33667=CARTESIAN_POINT('Ctrl Pts',(-19.2815769639979,-64.1666023583945,
32.5548733422617));
#33668=CARTESIAN_POINT('Ctrl Pts',(-18.0700434803867,-65.6091721564467,
32.4437402242701));
#33669=CARTESIAN_POINT('Ctrl Pts',(-18.6248821658744,-67.4094429797487,
32.3326071062786));
#33670=CARTESIAN_POINT('Ctrl Pts',(-20.4382828172642,-67.9197361128516,
32.221473988287));
#33671=CARTESIAN_POINT('Ctrl Pts',(-21.8505497836503,-66.6730111953947,
32.1103408702955));
#33672=CARTESIAN_POINT('Ctrl Pts',(-21.5691207511098,-64.8103199424505,
31.9992077523039));
#33673=CARTESIAN_POINT('Ctrl Pts',(-19.8515706471628,-64.0364707035261,
31.8880746343123));
#33674=CARTESIAN_POINT('Ctrl Pts',(-18.2698689290547,-65.0597207604948,
31.7769415163207));
#33675=CARTESIAN_POINT('Ctrl Pts',(-18.2716512643712,-66.9435513864888,
31.6658083983292));
#33676=CARTESIAN_POINT('Ctrl Pts',(-19.8552863896784,-67.9638066457476,
31.5546752803376));
#33677=CARTESIAN_POINT('Ctrl Pts',(-21.5713691070242,-67.1867087681419,
31.4435421623461));
#33678=CARTESIAN_POINT('Ctrl Pts',(-21.8492729691361,-65.3234883175307,
31.3324090443545));
#33679=CARTESIAN_POINT('Ctrl Pts',(-20.4346494232198,-64.0794379859558,
31.221275926363));
#33680=CARTESIAN_POINT('Ctrl Pts',(-18.6222176175382,-64.5931616022184,
31.1101428083714));
#33681=CARTESIAN_POINT('Ctrl Pts',(-18.0707864772717,-66.3944790927504,
30.9990096903798));
#33682=CARTESIAN_POINT('Ctrl Pts',(-19.2850474861105,-67.8347537910515,
30.8878765723883));
#33683=CARTESIAN_POINT('Ctrl Pts',(-21.1536611759177,-67.5957896045767,
30.7767434543967));
#33684=CARTESIAN_POINT('Ctrl Pts',(-21.9663987498635,-65.8962959623265,
30.6656103364051));
#33685=CARTESIAN_POINT('Ctrl Pts',(-20.9794107912338,-64.2917163371063,
30.5544772184136));
#33686=CARTESIAN_POINT('Ctrl Pts',(-19.0960275272337,-64.2506251575561,
30.443344100422));
#33687=CARTESIAN_POINT('Ctrl Pts',(-18.0399954503192,-65.8106306885334,
30.3322109824305));
#33688=CARTESIAN_POINT('Ctrl Pts',(-18.7778366822999,-67.5439544668685,
30.2210778644389));
#33689=CARTESIAN_POINT('Ctrl Pts',(-20.6342498865192,-67.8641903476697,
30.1099447464474));
#33690=CARTESIAN_POINT('Ctrl Pts',(-21.9101726307638,-66.4782458484667,
29.9988116284558));
#33691=CARTESIAN_POINT('Ctrl Pts',(-21.4378301996713,-64.6545919251736,
29.8876785104643));
#33692=CARTESIAN_POINT('Ctrl Pts',(-19.6495289773944,-64.0623084267076,
29.7765453924727));
#33693=CARTESIAN_POINT('Ctrl Pts',(-18.1819926294112,-65.2434765229158,
29.6654122744811));
#33694=CARTESIAN_POINT('Ctrl Pts',(-18.3783681830636,-67.1170446818255,
29.5542791564896));
#33695=CARTESIAN_POINT('Ctrl Pts',(-20.0589250023826,-67.9682495814781,
29.443146038498));
#33696=CARTESIAN_POINT('Ctrl Pts',(-21.6855513402555,-67.0180349946135,
29.3320129205065));
#33697=CARTESIAN_POINT('Ctrl Pts',(-21.7694947488723,-65.1360747112116,
29.2208798025149));
#33698=CARTESIAN_POINT('Ctrl Pts',(-20.2339269166865,-64.0448128558769,
29.1097466845233));
#33699=CARTESIAN_POINT('Ctrl Pts',(-18.4842599630755,-64.7430152302597,
28.9986135665318));
#33700=CARTESIAN_POINT('Ctrl Pts',(-18.1218579502043,-66.5916595403474,
28.8874804485402));
#33701=CARTESIAN_POINT('Ctrl Pts',(-19.4784054642569,-67.8987937516163,
28.7763473305487));
#33702=CARTESIAN_POINT('Ctrl Pts',(-21.3123368271822,-67.4680771856126,
28.6652142125571));
#33703=CARTESIAN_POINT('Ctrl Pts',(-21.9451658727967,-65.6937185963808,
28.5540810945656));
#33704=CARTESIAN_POINT('Ctrl Pts',(-20.797702550644,-64.1996808028605,28.4429479765739));
#33705=CARTESIAN_POINT('Ctrl Pts',(-18.9201504568774,-64.3533659984344,
28.3318148585824));
#33706=CARTESIAN_POINT('Ctrl Pts',(-18.0309191674365,-66.0141154431258,
28.2206817405908));
#33707=CARTESIAN_POINT('Ctrl Pts',(-18.943868158232,-67.6619458786863,28.1095486225993));
#33708=CARTESIAN_POINT('Ctrl Pts',(-20.8234305795421,-67.7886980325282,
27.9984155046077));
#33709=CARTESIAN_POINT('Ctrl Pts',(-21.9493569245747,-66.278363344517,27.8872823866162));
#33710=CARTESIAN_POINT('Ctrl Pts',(-21.2911550862336,-64.513259567359,27.7761492686246));
#33711=CARTESIAN_POINT('Ctrl Pts',(-19.4512372937262,-64.1088791516278,
27.6650161506331));
#33712=CARTESIAN_POINT('Ctrl Pts',(-18.1135687288438,-65.4353269702371,
27.5538830326415));
#33713=CARTESIAN_POINT('Ctrl Pts',(-18.5024363130261,-67.2785857707618,
27.4427499146499));
#33714=CARTESIAN_POINT('Ctrl Pts',(-20.26193312608,-67.9516325497133,27.3316167966584));
#33715=CARTESIAN_POINT('Ctrl Pts',(-21.7816984345104,-66.8384684027146,
27.2204836786668));
#33716=CARTESIAN_POINT('Ctrl Pts',(-21.6707832048173,-64.9579049736386,
27.1093505606753));
#33717=CARTESIAN_POINT('Ctrl Pts',(-20.0307014324503,-64.0311079253974,
26.9982174426837));
#33718=CARTESIAN_POINT('Ctrl Pts',(-18.3625204852342,-64.9063184061494,
26.8870843246922));
#33719=CARTESIAN_POINT('Ctrl Pts',(-18.1930252713496,-66.782509313568,26.7759512067006));
#33720=CARTESIAN_POINT('Ctrl Pts',(-19.6773443894448,-67.9425169276774,
26.6648180887091));
#33721=CARTESIAN_POINT('Ctrl Pts',(-21.4569707445669,-67.32465653357,26.5536849707174));
#33722=CARTESIAN_POINT('Ctrl Pts',(-21.90311988392,-65.4944184601696,26.4425518527259));
#33723=CARTESIAN_POINT('Ctrl Pts',(-20.6074592869896,-64.1269082758429,
26.3314187347343));
#33724=CARTESIAN_POINT('Ctrl Pts',(-18.7558270691641,-64.473725831526,26.2202856167428));
#33725=CARTESIAN_POINT('Ctrl Pts',(-18.0429128259432,-66.2174486428944,
26.1091524987512));
#33726=CARTESIAN_POINT('Ctrl Pts',(-19.1211979303562,-67.7621557655232,
25.9980193807597));
#33727=CARTESIAN_POINT('Ctrl Pts',(-21.0038049828108,-67.6940648494755,
25.8868862627682));
#33728=CARTESIAN_POINT('Ctrl Pts',(-21.9676748441585,-66.0755065309653,
25.7757531447765));
#33729=CARTESIAN_POINT('Ctrl Pts',(-21.1306818689754,-64.3878268583619,
25.664620026785));
#33730=CARTESIAN_POINT('Ctrl Pts',(-19.2587832782431,-64.1757010178898,
25.5534869087934));
#33731=CARTESIAN_POINT('Ctrl Pts',(-18.0653971591218,-65.6331865556109,
25.4423537908019));
#33732=CARTESIAN_POINT('Ctrl Pts',(-18.6423929466843,-67.4265115387061,
25.3312206728103));
#33733=CARTESIAN_POINT('Ctrl Pts',(-20.4624082215941,-67.9140030533836,
25.2200875548188));
#33734=CARTESIAN_POINT('Ctrl Pts',(-21.8582433164759,-66.650190129261,25.1089544368272));
#33735=CARTESIAN_POINT('Ctrl Pts',(-21.5552776423771,-64.7903673634893,
24.9978213188357));
#33736=CARTESIAN_POINT('Ctrl Pts',(-19.8248705803293,-64.0395083111156,
24.8866882008441));
#33737=CARTESIAN_POINT('Ctrl Pts',(-18.7848659979775,-64.7327675918889,
24.8125994555164));
#33738=CARTESIAN_POINT('Ctrl Pts',(-18.5264217726374,-65.2227463683951,
24.7755550828525));
#33739=CARTESIAN_POINT('Ctrl Pts',(-18.6322193753412,-64.8366876301902,
36.0748149723825));
#33740=CARTESIAN_POINT('Ctrl Pts',(-18.2454069475584,-65.2914876975057,
36.0377705997186));
#33741=CARTESIAN_POINT('Ctrl Pts',(-17.9681227304658,-66.6097459389905,
35.9636818543909));
#33742=CARTESIAN_POINT('Ctrl Pts',(-19.4123269945801,-68.040621101442,35.8525487363994));
#33743=CARTESIAN_POINT('Ctrl Pts',(-21.3946565954591,-67.599101991962,35.7414156184078));
#33744=CARTESIAN_POINT('Ctrl Pts',(-22.1003861870635,-65.6963321743655,
35.6302825004162));
#33745=CARTESIAN_POINT('Ctrl Pts',(-20.8838396803442,-64.0703377208937,
35.5191493824247));
#33746=CARTESIAN_POINT('Ctrl Pts',(-18.858328024941,-64.2110242041256,35.4080162644331));
#33747=CARTESIAN_POINT('Ctrl Pts',(-17.8777397145028,-65.9887618494759,
35.2968831464416));
#33748=CARTESIAN_POINT('Ctrl Pts',(-18.8395174075388,-67.7769304901502,
35.18575002845));
#33749=CARTESIAN_POINT('Ctrl Pts',(-20.8634195317534,-67.9387094824621,
35.0746169104584));
#33750=CARTESIAN_POINT('Ctrl Pts',(-22.0970835655348,-66.3261418250617,
34.963483792467));
#33751=CARTESIAN_POINT('Ctrl Pts',(-21.4114154592526,-64.4150579879853,
34.8523506744753));
#33752=CARTESIAN_POINT('Ctrl Pts',(-19.4339637301444,-63.954584663791,34.7412175564838));
#33753=CARTESIAN_POINT('Ctrl Pts',(-17.9745709960488,-65.3661513473781,
34.6300844384922));
#33754=CARTESIAN_POINT('Ctrl Pts',(-18.368930445043,-67.3578435803929,34.5189513205007));
#33755=CARTESIAN_POINT('Ctrl Pts',(-20.2561090299742,-68.1067827635803,
34.4078182025091));
#33756=CARTESIAN_POINT('Ctrl Pts',(-21.90888650971,-66.9275120216053,34.2966850845175));
#33757=CARTESIAN_POINT('Ctrl Pts',(-21.8145759430863,-64.8993454789214,
34.185551966526));
#33758=CARTESIAN_POINT('Ctrl Pts',(-20.0594940421212,-63.8785414217313,
34.0744188485344));
#33759=CARTESIAN_POINT('Ctrl Pts',(-18.2499608572679,-64.7993796817096,
33.9632857305429));
#33760=CARTESIAN_POINT('Ctrl Pts',(-18.0421323741426,-66.8190729497863,
33.8521526125513));
#33761=CARTESIAN_POINT('Ctrl Pts',(-19.6262214044097,-68.0891183973422,
33.7410194945598));
#33762=CARTESIAN_POINT('Ctrl Pts',(-21.5524073164968,-67.44712047002,33.6298863765682));
#33763=CARTESIAN_POINT('Ctrl Pts',(-22.0577689506937,-65.4806609257802,
33.5187532585766));
#33764=CARTESIAN_POINT('Ctrl Pts',(-20.6797794480564,-63.9895209455846,
33.4076201405851));
#33765=CARTESIAN_POINT('Ctrl Pts',(-18.6796290387811,-64.3384505265051,
33.2964870225935));
#33766=CARTESIAN_POINT('Ctrl Pts',(-17.8879341024671,-66.2080955841046,
33.185353904602));
#33767=CARTESIAN_POINT('Ctrl Pts',(-19.0292850056993,-67.887283372275,33.0742207866104));
#33768=CARTESIAN_POINT('Ctrl Pts',(-21.0590724786751,-67.8391551355372,
32.9630876686189));
#33769=CARTESIAN_POINT('Ctrl Pts',(-22.1195551344861,-66.107759730241,32.8519545506273));
#33770=CARTESIAN_POINT('Ctrl Pts',(-21.2401375063356,-64.2777383784837,
32.7408214326358));
#33771=CARTESIAN_POINT('Ctrl Pts',(-19.2256972210515,-64.0239986502764,
32.6296883146441));
#33772=CARTESIAN_POINT('Ctrl Pts',(-17.9199293153208,-65.5787731320006,
32.5185551966526));
#33773=CARTESIAN_POINT('Ctrl Pts',(-18.5179239709932,-67.5190710226412,
32.407422078661));
#33774=CARTESIAN_POINT('Ctrl Pts',(-20.4723729423565,-68.06905532331,32.2962889606695));
#33775=CARTESIAN_POINT('Ctrl Pts',(-21.9944876044574,-66.7253587548605,
32.1851558426779));
#33776=CARTESIAN_POINT('Ctrl Pts',(-21.6911687086917,-64.7177853041207,
32.0740227246864));
#33777=CARTESIAN_POINT('Ctrl Pts',(-19.8400256469796,-63.883745210528,31.9628896066948));
#33778=CARTESIAN_POINT('Ctrl Pts',(-18.135297409681,-64.9865847952371,31.8517564887032));
#33779=CARTESIAN_POINT('Ctrl Pts',(-18.1372183770211,-67.0169418629789,
31.7406233707117));
#33780=CARTESIAN_POINT('Ctrl Pts',(-19.8440304040817,-68.1165537112807,
31.6294902527201));
#33781=CARTESIAN_POINT('Ctrl Pts',(-21.6935919442302,-67.2790122962762,
31.5183571347286));
#33782=CARTESIAN_POINT('Ctrl Pts',(-21.9931114778899,-65.2708684862861,
31.407224016737));
#33783=CARTESIAN_POINT('Ctrl Pts',(-20.4684569388814,-63.9300545359839,
31.2960908987454));
#33784=CARTESIAN_POINT('Ctrl Pts',(-18.5150521711233,-64.4837361466086,
31.1849577807539));
#33785=CARTESIAN_POINT('Ctrl Pts',(-17.92073010333,-66.4251621154209,31.0738246627623));
#33786=CARTESIAN_POINT('Ctrl Pts',(-19.2294376842349,-67.9774629819821,
30.9626915447708));
#33787=CARTESIAN_POINT('Ctrl Pts',(-21.2433942255651,-67.7199118952488,
30.8515584267792));
#33788=CARTESIAN_POINT('Ctrl Pts',(-22.1193474321384,-65.8882297469111,
30.7404253087876));
#33789=CARTESIAN_POINT('Ctrl Pts',(-21.0555904521165,-64.1588441334349,
30.6292921907961));
#33790=CARTESIAN_POINT('Ctrl Pts',(-19.0257155426823,-64.1145568362275,
30.5181590728046));
#33791=CARTESIAN_POINT('Ctrl Pts',(-17.8875441160478,-65.7959013328247,
30.407025954813));
#33792=CARTESIAN_POINT('Ctrl Pts',(-18.6827754598598,-67.6640449628659,
30.2958928368214));
#33793=CARTESIAN_POINT('Ctrl Pts',(-20.6835825482607,-68.0091891467207,
30.1847597188298));
#33794=CARTESIAN_POINT('Ctrl Pts',(-22.0587479829466,-66.5154443425826,
30.0736266008383));
#33795=CARTESIAN_POINT('Ctrl Pts',(-21.5496662321087,-64.5499445884212,
29.9624934828467));
#33796=CARTESIAN_POINT('Ctrl Pts',(-19.6222689513765,-63.9115926205616,
29.8513603648552));
#33797=CARTESIAN_POINT('Ctrl Pts',(-18.0405859936936,-65.1846332852775,
29.7402272468636));
#33798=CARTESIAN_POINT('Ctrl Pts',(-18.2522358563662,-67.2039296598285,
29.6290941288721));
#33799=CARTESIAN_POINT('Ctrl Pts',(-20.0635082546187,-68.1213422234949,
29.5179610108805));
#33800=CARTESIAN_POINT('Ctrl Pts',(-21.8166553985837,-67.0972188890024,
29.406827892889));
#33801=CARTESIAN_POINT('Ctrl Pts',(-21.9071280189051,-65.0688776411803,
29.2956947748974));
#33802=CARTESIAN_POINT('Ctrl Pts',(-20.2521220124972,-63.8927362247689,
29.1845616569058));
#33803=CARTESIAN_POINT('Ctrl Pts',(-18.3663640168262,-64.645245556543,29.0734285389143));
#33804=CARTESIAN_POINT('Ctrl Pts',(-17.9757739722415,-66.6376794775842,
28.9622954209227));
#33805=CARTESIAN_POINT('Ctrl Pts',(-19.4378352610216,-68.0464840419207,
28.8511623029311));
#33806=CARTESIAN_POINT('Ctrl Pts',(-21.414411845503,-67.5822658622644,28.7400291849396));
#33807=CARTESIAN_POINT('Ctrl Pts',(-22.0964630382728,-65.6698956880862,
28.628896066948));
#33808=CARTESIAN_POINT('Ctrl Pts',(-20.8597487424332,-64.0596499729509,
28.5177629489565));
#33809=CARTESIAN_POINT('Ctrl Pts',(-18.8361585581401,-64.225288974003,28.4066298309649));
#33810=CARTESIAN_POINT('Ctrl Pts',(-17.8777618697857,-66.0152133579947,
28.2954967129733));
#33811=CARTESIAN_POINT('Ctrl Pts',(-18.8617210486907,-67.7912138779539,
28.1843635949818));
#33812=CARTESIAN_POINT('Ctrl Pts',(-20.8874779260401,-67.9278249553264,
28.0732304769902));
#33813=CARTESIAN_POINT('Ctrl Pts',(-22.1009800747204,-66.3000147551173,
27.9620973589987));
#33814=CARTESIAN_POINT('Ctrl Pts',(-21.3915825651798,-64.3976192425913,
27.8509642410071));
#33815=CARTESIAN_POINT('Ctrl Pts',(-19.4085539199639,-63.9617856682735,
27.7398311230155));
#33816=CARTESIAN_POINT('Ctrl Pts',(-17.9668400060223,-65.3914060738144,
27.628698005024));
#33817=CARTESIAN_POINT('Ctrl Pts',(-18.3859541434961,-67.378035594368,27.5175648870324));
#33818=CARTESIAN_POINT('Ctrl Pts',(-20.2823065760127,-68.1034327005137,
27.4064317690409));
#33819=CARTESIAN_POINT('Ctrl Pts',(-21.9202809207881,-66.9036854078278,
27.2952986510493));
#33820=CARTESIAN_POINT('Ctrl Pts',(-21.8007385811424,-64.8768496632148,
27.1841655330578));
#33821=CARTESIAN_POINT('Ctrl Pts',(-20.0330894240199,-63.8779653095508,
27.0730324150662));
#33822=CARTESIAN_POINT('Ctrl Pts',(-18.2351555069698,-64.821250635119,26.9618992970747));
#33823=CARTESIAN_POINT('Ctrl Pts',(-18.0524767667952,-66.8433737584758,
26.8507661790831));
#33824=CARTESIAN_POINT('Ctrl Pts',(-19.6522478771192,-68.0936080552553,
26.7396330610915));
#33825=CARTESIAN_POINT('Ctrl Pts',(-21.5702955498791,-67.4276897923586,
26.6284999431));
#33826=CARTESIAN_POINT('Ctrl Pts',(-22.0511466656074,-65.4550937655699,
26.5173668251084));
#33827=CARTESIAN_POINT('Ctrl Pts',(-20.6547081460967,-63.9812171178266,
26.4062337071169));
#33828=CARTESIAN_POINT('Ctrl Pts',(-18.6590539145297,-64.3550105288059,
26.2951005891253));
#33829=CARTESIAN_POINT('Ctrl Pts',(-17.8906884083933,-66.2343620402385,
26.1839674711337));
#33830=CARTESIAN_POINT('Ctrl Pts',(-19.0528437277604,-67.8992182012669,
26.0728343531422));
#33831=CARTESIAN_POINT('Ctrl Pts',(-21.0818820510516,-67.8258310980217,
25.9617012351506));
#33832=CARTESIAN_POINT('Ctrl Pts',(-22.1207227824672,-66.0813795129406,
25.850568117159));
#33833=CARTESIAN_POINT('Ctrl Pts',(-21.2186275625656,-64.2624302379513,
25.7394349991675));
#33834=CARTESIAN_POINT('Ctrl Pts',(-19.201130617062,-64.033805013629,25.6283018811759));
#33835=CARTESIAN_POINT('Ctrl Pts',(-17.914921598019,-65.6046553978465,25.5171687631844));
#33836=CARTESIAN_POINT('Ctrl Pts',(-18.5367967598142,-67.5374671931023,
25.4060356451928));
#33837=CARTESIAN_POINT('Ctrl Pts',(-20.4983748474734,-68.0628763400987,
25.2949025272013));
#33838=CARTESIAN_POINT('Ctrl Pts',(-22.0027795488249,-66.7007626408157,
25.1837694092097));
#33839=CARTESIAN_POINT('Ctrl Pts',(-21.676248867562,-64.6962807913717,25.0726362912181));
#33840=CARTESIAN_POINT('Ctrl Pts',(-19.8112488192455,-63.8870190866151,
24.9615031732266));
#33841=CARTESIAN_POINT('Ctrl Pts',(-18.6903515235305,-64.6342008454597,
24.8874144278989));
#33842=CARTESIAN_POINT('Ctrl Pts',(-18.4118052188385,-65.162290716277,24.850370055235));
#33843=CARTESIAN_POINT('Ctrl Pts',(-18.5335096305348,-64.7527339134289,
36.149629944765));
#33844=CARTESIAN_POINT('Ctrl Pts',(-18.1187817934049,-65.2403559097683,
36.1125855721011));
#33845=CARTESIAN_POINT('Ctrl Pts',(-17.82148657907,-66.6537499736649,36.0384968267734));
#33846=CARTESIAN_POINT('Ctrl Pts',(-19.3699159153844,-68.1878882761179,
35.9273637087819));
#33847=CARTESIAN_POINT('Ctrl Pts',(-21.4953059204666,-67.7145056953778,
35.8162305907903));
#33848=CARTESIAN_POINT('Ctrl Pts',(-22.2519664776322,-65.6744171296325,
35.7050974727987));
#33849=CARTESIAN_POINT('Ctrl Pts',(-20.9476244625846,-63.9310782024452,
35.5939643548072));
#33850=CARTESIAN_POINT('Ctrl Pts',(-18.7759360482752,-64.0819177223609,
35.4828312368156));
#33851=CARTESIAN_POINT('Ctrl Pts',(-17.7245808179535,-65.9879508166608,
35.3716981188241));
#33852=CARTESIAN_POINT('Ctrl Pts',(-18.7557679096376,-67.9051676884693,
35.2605650008325));
#33853=CARTESIAN_POINT('Ctrl Pts',(-20.9257306364026,-68.0786219178465,
35.149431882841));
#33854=CARTESIAN_POINT('Ctrl Pts',(-22.2484255131102,-66.3496787693217,
35.0382987648494));
#33855=CARTESIAN_POINT('Ctrl Pts',(-21.5132742349122,-64.300676179442,34.9271656468578));
#33856=CARTESIAN_POINT('Ctrl Pts',(-19.3931141269688,-63.8069714996472,
34.8160325288663));
#33857=CARTESIAN_POINT('Ctrl Pts',(-17.8284002019177,-65.3204078724244,
34.7048994108747));
#33858=CARTESIAN_POINT('Ctrl Pts',(-18.2512197123211,-67.4558361903855,
34.5937662928832));
#33859=CARTESIAN_POINT('Ctrl Pts',(-20.2745918601413,-68.2588246811265,
34.4826331748916));
#33860=CARTESIAN_POINT('Ctrl Pts',(-22.0466466861892,-66.9944485414733,
34.3715000569001));
#33861=CARTESIAN_POINT('Ctrl Pts',(-21.9455299316461,-64.819913642458,34.2603669389084));
#33862=CARTESIAN_POINT('Ctrl Pts',(-20.0637875973957,-63.7254403826442,
34.149233820917));
#33863=CARTESIAN_POINT('Ctrl Pts',(-18.1236643488468,-64.7127335316683,
34.0381007029253));
#33864=CARTESIAN_POINT('Ctrl Pts',(-17.9008373373297,-66.8781836583265,
33.9269675849339));
#33865=CARTESIAN_POINT('Ctrl Pts',(-19.5992466183076,-68.2398855160997,
33.8158344669422));
#33866=CARTESIAN_POINT('Ctrl Pts',(-21.6644411670167,-67.5515559984407,
33.7047013489507));
#33867=CARTESIAN_POINT('Ctrl Pts',(-22.2062736482538,-65.4431813573757,
33.5935682309591));
#33868=CARTESIAN_POINT('Ctrl Pts',(-20.7288376483501,-63.8444290567085,
33.4824351129676));
#33869=CARTESIAN_POINT('Ctrl Pts',(-18.5843407459935,-64.2185401245333,
33.371301994976));
#33870=CARTESIAN_POINT('Ctrl Pts',(-17.7355109126651,-66.2231133885917,
33.2601688769844));
#33871=CARTESIAN_POINT('Ctrl Pts',(-18.9592306215095,-68.023484497438,33.1490357589929));
#33872=CARTESIAN_POINT('Ctrl Pts',(-21.135503429821,-67.9718829508136,33.0379026410013));
#33873=CARTESIAN_POINT('Ctrl Pts',(-22.2725188061863,-66.1155365149686,
32.9267695230097));
#33874=CARTESIAN_POINT('Ctrl Pts',(-21.3296355256586,-64.1534465131912,
32.8156364050182));
#33875=CARTESIAN_POINT('Ctrl Pts',(-19.1698174781052,-63.8813949421583,
32.7045032870266));
#33876=CARTESIAN_POINT('Ctrl Pts',(-17.7698151502549,-65.5483741075547,
32.5933701690351));
#33877=CARTESIAN_POINT('Ctrl Pts',(-18.410965776112,-67.6286990655338,32.4822370510435));
#33878=CARTESIAN_POINT('Ctrl Pts',(-20.5064630674488,-68.2183745337685,
32.371103933052));
#33879=CARTESIAN_POINT('Ctrl Pts',(-22.1384254252645,-66.7777063143262,
32.2599708150604));
#33880=CARTESIAN_POINT('Ctrl Pts',(-21.8132166662735,-64.6252506657909,
32.1488376970689));
#33881=CARTESIAN_POINT('Ctrl Pts',(-19.8284806467965,-63.73101971753,32.0377045790773));
#33882=CARTESIAN_POINT('Ctrl Pts',(-18.0007258903072,-64.9134488299795,
31.9265714610857));
#33883=CARTESIAN_POINT('Ctrl Pts',(-18.002785489671,-67.090332339469,31.8154383430942));
#33884=CARTESIAN_POINT('Ctrl Pts',(-19.8327744184849,-68.2693007768138,
31.7043052251026));
#33885=CARTESIAN_POINT('Ctrl Pts',(-21.8158147814363,-67.3713158244104,
31.5931721071111));
#33886=CARTESIAN_POINT('Ctrl Pts',(-22.1369499866437,-65.2182486550417,
31.4820389891195));
#33887=CARTESIAN_POINT('Ctrl Pts',(-20.502264454543,-63.780671086012,31.3709058711279));
#33888=CARTESIAN_POINT('Ctrl Pts',(-18.4078867247083,-64.3743106909989,
31.2597727531364));
#33889=CARTESIAN_POINT('Ctrl Pts',(-17.7706737293884,-66.4558451380913,
31.1486396351448));
#33890=CARTESIAN_POINT('Ctrl Pts',(-19.1738278823592,-68.1201721729128,
31.0375065171533));
#33891=CARTESIAN_POINT('Ctrl Pts',(-21.3331272752126,-67.8440341859209,
30.9263733991617));
#33892=CARTESIAN_POINT('Ctrl Pts',(-22.2722961144131,-65.8801635314959,
30.8152402811701));
#33893=CARTESIAN_POINT('Ctrl Pts',(-21.1317701129993,-64.0259719297634,
30.7041071631786));
#33894=CARTESIAN_POINT('Ctrl Pts',(-18.9554035581309,-63.978488514899,30.592974045187));
#33895=CARTESIAN_POINT('Ctrl Pts',(-17.7350927817764,-65.7811719771159,
30.4818409271955));
#33896=CARTESIAN_POINT('Ctrl Pts',(-18.5877142374196,-67.7841354588633,
30.3707078092039));
#33897=CARTESIAN_POINT('Ctrl Pts',(-20.7329152100023,-68.1541879457717,
30.2595746912124));
#33898=CARTESIAN_POINT('Ctrl Pts',(-22.2073233351293,-66.5526428366984,
30.1484415732208));
#33899=CARTESIAN_POINT('Ctrl Pts',(-21.6615022645462,-64.4452972516688,
30.0373084552293));
#33900=CARTESIAN_POINT('Ctrl Pts',(-19.5950089253585,-63.7608768144156,
29.9261753372376));
#33901=CARTESIAN_POINT('Ctrl Pts',(-17.8991793579761,-65.1257900476391,
29.8150422192461));
#33902=CARTESIAN_POINT('Ctrl Pts',(-18.1261035296687,-67.2908146378317,
29.7039091012545));
#33903=CARTESIAN_POINT('Ctrl Pts',(-20.0680915068549,-68.2744348655116,
29.592775983263));
#33904=CARTESIAN_POINT('Ctrl Pts',(-21.9477594569119,-67.1764027833913,
29.4816428652714));
#33905=CARTESIAN_POINT('Ctrl Pts',(-22.044761288938,-65.001680571149,29.3705097472799));
#33906=CARTESIAN_POINT('Ctrl Pts',(-20.2703171083079,-63.7406595936608,
29.2593766292883));
#33907=CARTESIAN_POINT('Ctrl Pts',(-18.2484680705768,-64.5474758828262,
29.1482435112968));
#33908=CARTESIAN_POINT('Ctrl Pts',(-17.8296899942787,-66.683699414821,29.0371103933052));
#33909=CARTESIAN_POINT('Ctrl Pts',(-19.3972650577863,-68.1941743322251,
28.9259772753137));
#33910=CARTESIAN_POINT('Ctrl Pts',(-21.5164868638238,-67.6964545389165,
28.8148441573221));
#33911=CARTESIAN_POINT('Ctrl Pts',(-22.247760203749,-65.6460727797915,28.7037110393305));
#33912=CARTESIAN_POINT('Ctrl Pts',(-20.9217949342225,-63.9196191430413,
28.592577921339));
#33913=CARTESIAN_POINT('Ctrl Pts',(-18.7521666594028,-64.0972119495715,
28.4814448033474));
#33914=CARTESIAN_POINT('Ctrl Pts',(-17.7246045721348,-66.0163112728636,
28.3703116853558));
#33915=CARTESIAN_POINT('Ctrl Pts',(-18.7795739391494,-67.9204818772215,
28.2591785673643));
#33916=CARTESIAN_POINT('Ctrl Pts',(-20.9515252725381,-68.0669518781245,
28.1480454493727));
#33917=CARTESIAN_POINT('Ctrl Pts',(-22.2526032248661,-66.3216661657179,
28.0369123313812));
#33918=CARTESIAN_POINT('Ctrl Pts',(-21.492010044126,-64.2819789178235,27.9257792133896));
#33919=CARTESIAN_POINT('Ctrl Pts',(-19.3658705462016,-63.8146921849193,
27.8146460953981));
#33920=CARTESIAN_POINT('Ctrl Pts',(-17.8201112832008,-65.3474851773918,
27.7035129774065));
#33921=CARTESIAN_POINT('Ctrl Pts',(-18.2694719739661,-67.4774854179741,
27.5923798594149));
#33922=CARTESIAN_POINT('Ctrl Pts',(-20.3026800259454,-68.2552328513142,
27.4812467414234));
#33923=CARTESIAN_POINT('Ctrl Pts',(-22.0588634070658,-66.9689024129409,
27.3701136234318));
#33924=CARTESIAN_POINT('Ctrl Pts',(-21.9306939574675,-64.7957943527911,
27.2589805054402));
#33925=CARTESIAN_POINT('Ctrl Pts',(-20.0354774155896,-63.724822693704,27.1478473874487));
#33926=CARTESIAN_POINT('Ctrl Pts',(-18.1077905287054,-64.7361828640888,
27.0367142694571));
#33927=CARTESIAN_POINT('Ctrl Pts',(-17.9119282622408,-66.9042382033836,
26.9255811514656));
#33928=CARTESIAN_POINT('Ctrl Pts',(-19.6271513647936,-68.2446991828334,
26.814448033474));
#33929=CARTESIAN_POINT('Ctrl Pts',(-21.6836203551913,-67.530723051147,26.7033149154825));
#33930=CARTESIAN_POINT('Ctrl Pts',(-22.1991734472949,-65.4157690709703,
26.5921817974909));
#33931=CARTESIAN_POINT('Ctrl Pts',(-20.7019570052038,-63.8355259598101,
26.4810486794993));
#33932=CARTESIAN_POINT('Ctrl Pts',(-18.5622807598954,-64.236295226086,26.3699155615078));
#33933=CARTESIAN_POINT('Ctrl Pts',(-17.7384639908433,-66.2512754375824,
26.2587824435162));
#33934=CARTESIAN_POINT('Ctrl Pts',(-18.9844895251645,-68.0362806370106,
26.1476493255246));
#33935=CARTESIAN_POINT('Ctrl Pts',(-21.1599591192924,-67.9575973465678,
26.0365162075331));
#33936=CARTESIAN_POINT('Ctrl Pts',(-22.2737707207758,-66.087252494916,25.9253830895415));
#33937=CARTESIAN_POINT('Ctrl Pts',(-21.3065732561559,-64.1370336175406,
25.81424997155));
#33938=CARTESIAN_POINT('Ctrl Pts',(-19.143477955881,-63.8919090093683,25.7031168535584));
#33939=CARTESIAN_POINT('Ctrl Pts',(-17.7644460369163,-65.5761242400821,
25.5919837355669));
#33940=CARTESIAN_POINT('Ctrl Pts',(-18.4312005729442,-67.6484228474986,
25.4808506175753));
#33941=CARTESIAN_POINT('Ctrl Pts',(-20.5343414733527,-68.2117496268139,
25.3697174995837));
#33942=CARTESIAN_POINT('Ctrl Pts',(-22.1473157811738,-66.7513351523705,
25.2585843815922));
#33943=CARTESIAN_POINT('Ctrl Pts',(-21.7972200927469,-64.6021942192541,
25.1474512636006));
#33944=CARTESIAN_POINT('Ctrl Pts',(-19.7976270581616,-63.7345298621146,
25.0363181456091));
#33945=CARTESIAN_POINT('Ctrl Pts',(-18.5958370490835,-64.5356340990305,
24.9622294002814));
#33946=CARTESIAN_POINT('Ctrl Pts',(-18.2971886650395,-65.1018350641589,
24.9251850276175));
#33947=CARTESIAN_POINT('Ctrl Pts',(-18.4347998857283,-64.6687801966677,
36.2244449171475));
#33948=CARTESIAN_POINT('Ctrl Pts',(-17.9921566392513,-65.1892241220309,
36.1874005444836));
#33949=CARTESIAN_POINT('Ctrl Pts',(-17.6748504276742,-66.6977540083394,
36.1133117991559));
#33950=CARTESIAN_POINT('Ctrl Pts',(-19.3275048361888,-68.3351554507938,
36.0021786811644));
#33951=CARTESIAN_POINT('Ctrl Pts',(-21.5959552454742,-67.8299093987937,
35.8910455631728));
#33952=CARTESIAN_POINT('Ctrl Pts',(-22.4035467682009,-65.6525020848995,
35.7799124451812));
#33953=CARTESIAN_POINT('Ctrl Pts',(-21.0114092448251,-63.7918186839967,
35.6687793271897));
#33954=CARTESIAN_POINT('Ctrl Pts',(-18.6935440716095,-63.9528112405962,
35.5576462091981));
#33955=CARTESIAN_POINT('Ctrl Pts',(-17.5714219214042,-65.9871397838458,
35.4465130912065));
#33956=CARTESIAN_POINT('Ctrl Pts',(-18.6720184117364,-68.0334048867885,
35.335379973215));
#33957=CARTESIAN_POINT('Ctrl Pts',(-20.9880417410518,-68.218534353231,35.2242468552234));
#33958=CARTESIAN_POINT('Ctrl Pts',(-22.3997674606856,-66.3732157135816,
35.1131137372319));
#33959=CARTESIAN_POINT('Ctrl Pts',(-21.6151330105718,-64.1862943708987,
35.0019806192403));
#33960=CARTESIAN_POINT('Ctrl Pts',(-19.3522645237931,-63.6593583355034,
34.8908475012488));
#33961=CARTESIAN_POINT('Ctrl Pts',(-17.6822294077865,-65.2746643974708,
34.7797143832572));
#33962=CARTESIAN_POINT('Ctrl Pts',(-18.1335089795993,-67.5538288003781,
34.6685812652656));
#33963=CARTESIAN_POINT('Ctrl Pts',(-20.2930746903084,-68.4108665986726,
34.5574481472741));
#33964=CARTESIAN_POINT('Ctrl Pts',(-22.1844068626685,-67.0613850613413,
34.4463150292825));
#33965=CARTESIAN_POINT('Ctrl Pts',(-22.076483920206,-64.7404818059946,34.3351819112909));
#33966=CARTESIAN_POINT('Ctrl Pts',(-20.0680811526701,-63.5723393435572,
34.2240487932995));
#33967=CARTESIAN_POINT('Ctrl Pts',(-17.9973678404257,-64.6260873816269,
34.1129156753078));
#33968=CARTESIAN_POINT('Ctrl Pts',(-17.7595423005167,-66.9372943668669,
34.0017825573163));
#33969=CARTESIAN_POINT('Ctrl Pts',(-19.5722718322054,-68.3906526348572,
33.8906494393247));
#33970=CARTESIAN_POINT('Ctrl Pts',(-21.7764750175367,-67.6559915268615,
33.7795163213332));
#33971=CARTESIAN_POINT('Ctrl Pts',(-22.354778345814,-65.4057017889712,33.6683832033416));
#33972=CARTESIAN_POINT('Ctrl Pts',(-20.7778958486438,-63.6993371678323,
33.5572500853501));
#33973=CARTESIAN_POINT('Ctrl Pts',(-18.4890524532058,-64.0986297225616,
33.4461169673585));
#33974=CARTESIAN_POINT('Ctrl Pts',(-17.5830877228631,-66.2381311930787,
33.334983849367));
#33975=CARTESIAN_POINT('Ctrl Pts',(-18.8891762373197,-68.159685622601,33.2238507313753));
#33976=CARTESIAN_POINT('Ctrl Pts',(-21.2119343809668,-68.1046107660899,
33.1127176133838));
#33977=CARTESIAN_POINT('Ctrl Pts',(-22.4254824778866,-66.1233132996962,
33.0015844953923));
#33978=CARTESIAN_POINT('Ctrl Pts',(-21.4191335449815,-64.0291546478987,
32.8904513774007));
#33979=CARTESIAN_POINT('Ctrl Pts',(-19.1139377351588,-63.7387912340402,
32.7793182594091));
#33980=CARTESIAN_POINT('Ctrl Pts',(-17.6197009851889,-65.5179750831086,
32.6681851414176));
#33981=CARTESIAN_POINT('Ctrl Pts',(-18.3040075812308,-67.7383271084264,
32.557052023426));
#33982=CARTESIAN_POINT('Ctrl Pts',(-20.5405531925411,-68.3676937442268,
32.4459189054345));
#33983=CARTESIAN_POINT('Ctrl Pts',(-22.2823632460717,-66.8300538737919,
32.3347857874429));
#33984=CARTESIAN_POINT('Ctrl Pts',(-21.9352646238553,-64.532716027461,32.2236526694514));
#33985=CARTESIAN_POINT('Ctrl Pts',(-19.8169356466133,-63.578294224532,32.1125195514598));
#33986=CARTESIAN_POINT('Ctrl Pts',(-17.8661543709335,-64.8403128647219,
32.0013864334682));
#33987=CARTESIAN_POINT('Ctrl Pts',(-17.8683526023209,-67.163722815959,31.8902533154767));
#33988=CARTESIAN_POINT('Ctrl Pts',(-19.8215184328882,-68.4220478423468,
31.7791201974851));
#33989=CARTESIAN_POINT('Ctrl Pts',(-21.9380376186423,-67.4636193525447,
31.6679870794936));
#33990=CARTESIAN_POINT('Ctrl Pts',(-22.2807884953976,-65.1656288237973,
31.556853961502));
#33991=CARTESIAN_POINT('Ctrl Pts',(-20.5360719702046,-63.63128763604,31.4457208435104));
#33992=CARTESIAN_POINT('Ctrl Pts',(-18.3007212782933,-64.2648852353891,
31.3345877255189));
#33993=CARTESIAN_POINT('Ctrl Pts',(-17.6206173554466,-66.4865281607617,
31.2234546075273));
#33994=CARTESIAN_POINT('Ctrl Pts',(-19.1182180804836,-68.2628813638435,
31.1123214895358));
#33995=CARTESIAN_POINT('Ctrl Pts',(-21.42286032486,-67.9681564765929,31.0011883715442));
#33996=CARTESIAN_POINT('Ctrl Pts',(-22.425244796688,-65.8720973160807,30.8900552535526));
#33997=CARTESIAN_POINT('Ctrl Pts',(-21.207949773882,-63.8930997260919,30.778922135561));
#33998=CARTESIAN_POINT('Ctrl Pts',(-18.8850915735795,-63.8424201935705,
30.6677890175695));
#33999=CARTESIAN_POINT('Ctrl Pts',(-17.582641447505,-65.766442621407,30.556655899578));
#34000=CARTESIAN_POINT('Ctrl Pts',(-18.4926530149794,-67.9042259548608,
30.4455227815864));
#34001=CARTESIAN_POINT('Ctrl Pts',(-20.7822478717438,-68.2991867448226,
30.3343896635948));
#34002=CARTESIAN_POINT('Ctrl Pts',(-22.3558986873121,-66.5898413308144,
30.2232565456033));
#34003=CARTESIAN_POINT('Ctrl Pts',(-21.7733382969836,-64.3406499149163,
30.1121234276117));
#34004=CARTESIAN_POINT('Ctrl Pts',(-19.5677488993405,-63.6101610082697,
30.0009903096201));
#34005=CARTESIAN_POINT('Ctrl Pts',(-17.7577727222585,-65.0669468100008,
29.8898571916286));
#34006=CARTESIAN_POINT('Ctrl Pts',(-17.9999712029712,-67.3776996158348,
29.7787240736371));
#34007=CARTESIAN_POINT('Ctrl Pts',(-20.072674759091,-68.4275275075284,29.6675909556455));
#34008=CARTESIAN_POINT('Ctrl Pts',(-22.0788635152401,-67.2555866777803,
29.5564578376539));
#34009=CARTESIAN_POINT('Ctrl Pts',(-22.1823945589708,-64.9344835011177,
29.4453247196624));
#34010=CARTESIAN_POINT('Ctrl Pts',(-20.2885122041186,-63.5885829625528,
29.3341916016708));
#34011=CARTESIAN_POINT('Ctrl Pts',(-18.1305721243274,-64.4497062091094,
29.2230584836793));
#34012=CARTESIAN_POINT('Ctrl Pts',(-17.6836060163159,-66.729719352058,29.1119253656877));
#34013=CARTESIAN_POINT('Ctrl Pts',(-19.3566948545509,-68.3418646225293,
29.0007922476961));
#34014=CARTESIAN_POINT('Ctrl Pts',(-21.6185618821445,-67.8106432155685,
28.8896591297046));
#34015=CARTESIAN_POINT('Ctrl Pts',(-22.3990573692251,-65.6222498714967,
28.778526011713));
#34016=CARTESIAN_POINT('Ctrl Pts',(-20.9838411260118,-63.7795883131318,
28.6673928937215));
#34017=CARTESIAN_POINT('Ctrl Pts',(-18.6681747606656,-63.9691349251399,
28.5562597757299));
#34018=CARTESIAN_POINT('Ctrl Pts',(-17.5714472744839,-66.0174091877327,
28.4451266577383));
#34019=CARTESIAN_POINT('Ctrl Pts',(-18.6974268296081,-68.0497498764889,
28.3339935397468));
#34020=CARTESIAN_POINT('Ctrl Pts',(-21.0155726190361,-68.2060788009229,
28.2228604217552));
#34021=CARTESIAN_POINT('Ctrl Pts',(-22.4042263750118,-66.3433175763181,
28.1117273037637));
#34022=CARTESIAN_POINT('Ctrl Pts',(-21.5924375230723,-64.1663385930559,
28.0005941857721));
#34023=CARTESIAN_POINT('Ctrl Pts',(-19.3231871724393,-63.667598701565,27.8894610677806));
#34024=CARTESIAN_POINT('Ctrl Pts',(-17.6733825603793,-65.3035642809691,
27.778327949789));
#34025=CARTESIAN_POINT('Ctrl Pts',(-18.152989804436,-67.5769352415803,27.6671948317974));
#34026=CARTESIAN_POINT('Ctrl Pts',(-20.3230534758781,-68.4070330021147,
27.5560617138059));
#34027=CARTESIAN_POINT('Ctrl Pts',(-22.1974458933435,-67.034119418054,27.4449285958143));
#34028=CARTESIAN_POINT('Ctrl Pts',(-22.0606493337925,-64.7147390423673,
27.3337954778227));
#34029=CARTESIAN_POINT('Ctrl Pts',(-20.0378654071592,-63.5716800778574,
27.2226623598312));
#34030=CARTESIAN_POINT('Ctrl Pts',(-17.9804255504411,-64.6511150930585,
27.1115292418396));
#34031=CARTESIAN_POINT('Ctrl Pts',(-17.7713797576864,-66.9651026482916,
27.0003961238481));
#34032=CARTESIAN_POINT('Ctrl Pts',(-19.602054852468,-68.3957903104112,26.8892630058565));
#34033=CARTESIAN_POINT('Ctrl Pts',(-21.7969451605035,-67.6337563099357,
26.7781298878649));
#34034=CARTESIAN_POINT('Ctrl Pts',(-22.3472002289823,-65.3764443763705,
26.6669967698734));
#34035=CARTESIAN_POINT('Ctrl Pts',(-20.7492058643109,-63.6898348017937,
26.5558636518818));
#34036=CARTESIAN_POINT('Ctrl Pts',(-18.465507605261,-64.1175799233661,26.4447305338903));
#34037=CARTESIAN_POINT('Ctrl Pts',(-17.5862395732934,-66.2681888349264,
26.3335974158987));
#34038=CARTESIAN_POINT('Ctrl Pts',(-18.9161353225687,-68.1733430727544,
26.2224642979071));
#34039=CARTESIAN_POINT('Ctrl Pts',(-21.2380361875332,-68.089363595114,26.1113311799156));
#34040=CARTESIAN_POINT('Ctrl Pts',(-22.4268186590844,-66.0931254768914,
26.000198061924));
#34041=CARTESIAN_POINT('Ctrl Pts',(-21.3945189497461,-64.0116369971301,
25.8890649439325));
#34042=CARTESIAN_POINT('Ctrl Pts',(-19.0858252946999,-63.7500130051076,
25.7779318259409));
#34043=CARTESIAN_POINT('Ctrl Pts',(-17.6139704758136,-65.5475930823177,
25.6667987079494));
#34044=CARTESIAN_POINT('Ctrl Pts',(-18.3256043860741,-67.7593785018947,
25.5556655899578));
#34045=CARTESIAN_POINT('Ctrl Pts',(-20.570308099232,-68.3606229135291,25.4445324719662));
#34046=CARTESIAN_POINT('Ctrl Pts',(-22.2918520135227,-66.8019076639252,
25.3333993539747));
#34047=CARTESIAN_POINT('Ctrl Pts',(-21.9181913179318,-64.5081076471365,
25.2222662359831));
#34048=CARTESIAN_POINT('Ctrl Pts',(-19.7840052970778,-63.5820406376141,
25.1111331179915));
#34049=CARTESIAN_POINT('Ctrl Pts',(-18.5013225746365,-64.4370673526013,
25.0370443726639));
#34050=CARTESIAN_POINT('Ctrl Pts',(-18.1825721112405,-65.0413794120407,
25.));
#34051=CARTESIAN_POINT('Ctrl Pts',(-18.7309291201477,-64.9206413469514,
36.));
#34052=CARTESIAN_POINT('Ctrl Pts',(-18.6855998945711,-64.9629287034795,
36.));
#34053=CARTESIAN_POINT('Ctrl Pts',(-18.6430006729863,-65.0077851737201,
36.));
#34054=CARTESIAN_POINT('Ctrl Pts',(-18.6031299766235,-65.0548657336984,
36.));
#34055=CARTESIAN_POINT('Ctrl Pts',(-18.5606276998918,-65.105053745733,36.));
#34056=CARTESIAN_POINT('Ctrl Pts',(-18.5212252911969,-65.157769362507,36.));
#34057=CARTESIAN_POINT('Ctrl Pts',(-18.48494979168,-65.2126493493662,36.));
#34058=CARTESIAN_POINT('Ctrl Pts',(-18.4532087296026,-65.2606693378681,
36.));
#34059=CARTESIAN_POINT('Ctrl Pts',(-18.4238619507797,-65.3103476478189,
36.));
#34060=CARTESIAN_POINT('Ctrl Pts',(-18.3969504636413,-65.3614684945306,
36.));
#34061=CARTESIAN_POINT('Ctrl Pts',(-18.3834501843084,-65.3871135176685,
36.));
#34062=CARTESIAN_POINT('Ctrl Pts',(-18.3705631253762,-65.4131219219355,
36.));
#34063=CARTESIAN_POINT('Ctrl Pts',(-18.3582968052852,-65.4394683065982,
36.));
#34064=CARTESIAN_POINT('Ctrl Pts',(-18.3526878548587,-65.4515155680748,
36.));
#34065=CARTESIAN_POINT('Ctrl Pts',(-18.3472081170408,-65.4636351822643,
36.));
#34066=CARTESIAN_POINT('Ctrl Pts',(-18.3418668232121,-65.4758047617324,
36.));
#34067=CARTESIAN_POINT('Ctrl Pts',(-18.3149478587099,-65.5371368075278,
36.));
#34068=CARTESIAN_POINT('Ctrl Pts',(-18.2914900585818,-65.5998443155028,
36.));
#34069=CARTESIAN_POINT('Ctrl Pts',(-18.2715169288168,-65.6635695192081,
36.));
#34070=CARTESIAN_POINT('Ctrl Pts',(-18.2511894863638,-65.728425174099,36.));
#34071=CARTESIAN_POINT('Ctrl Pts',(-18.2344708858127,-65.7943357931695,
36.));
#34072=CARTESIAN_POINT('Ctrl Pts',(-18.2214252225953,-65.8609607427827,
36.));
#34073=CARTESIAN_POINT('Ctrl Pts',(-18.2105139769834,-65.916685099375,36.));
#34074=CARTESIAN_POINT('Ctrl Pts',(-18.2021726753615,-65.9729101042603,
36.));
#34075=CARTESIAN_POINT('Ctrl Pts',(-18.1964636437841,-66.0294487409383,
36.));
#34076=CARTESIAN_POINT('Ctrl Pts',(-18.1938340141056,-66.0554909295261,
36.));
#34077=CARTESIAN_POINT('Ctrl Pts',(-18.1917631829515,-66.081599771445,36.));
#34078=CARTESIAN_POINT('Ctrl Pts',(-18.1902590427239,-66.1077573920335,
36.));
#34079=CARTESIAN_POINT('Ctrl Pts',(-18.18960167741,-66.119189246694,36.));
#34080=CARTESIAN_POINT('Ctrl Pts',(-18.189052668073,-66.1306302131104,36.));
#34081=CARTESIAN_POINT('Ctrl Pts',(-18.1886130081778,-66.14206466439,36.));
#34082=CARTESIAN_POINT('Ctrl Pts',(-18.1859166238465,-66.2121908587719,
36.));
#34083=CARTESIAN_POINT('Ctrl Pts',(-18.187320978683,-66.2822033640486,36.));
#34084=CARTESIAN_POINT('Ctrl Pts',(-18.1928807035668,-66.3517413797487,
36.));
#34085=CARTESIAN_POINT('Ctrl Pts',(-18.1978502575643,-66.4138978589117,
36.));
#34086=CARTESIAN_POINT('Ctrl Pts',(-18.2061401607249,-66.4756762006059,
36.));
#34087=CARTESIAN_POINT('Ctrl Pts',(-18.2178225373334,-66.5368308666899,
36.));
#34088=CARTESIAN_POINT('Ctrl Pts',(-18.2305529842617,-66.6034719498439,
36.));
#34089=CARTESIAN_POINT('Ctrl Pts',(-18.2473108243593,-66.6693732662793,
36.));
#34090=CARTESIAN_POINT('Ctrl Pts',(-18.2678508258431,-66.7343212384354,
36.));
#34091=CARTESIAN_POINT('Ctrl Pts',(-18.2757801894081,-66.7593940742109,
36.));
#34092=CARTESIAN_POINT('Ctrl Pts',(-18.2842737653242,-66.784324785242,36.));
#34093=CARTESIAN_POINT('Ctrl Pts',(-18.2933194547362,-66.8091007633723,
36.));
#34094=CARTESIAN_POINT('Ctrl Pts',(-18.2972868318851,-66.8199673369411,
36.));
#34095=CARTESIAN_POINT('Ctrl Pts',(-18.3013603141585,-66.8308035780201,
36.));
#34096=CARTESIAN_POINT('Ctrl Pts',(-18.3055337954211,-66.8415958863165,
36.));
#34097=CARTESIAN_POINT('Ctrl Pts',(-18.3307566163043,-66.9068202019305,
36.));
#34098=CARTESIAN_POINT('Ctrl Pts',(-18.3596702577605,-66.9705591095508,
36.));
#34099=CARTESIAN_POINT('Ctrl Pts',(-18.3919620622396,-67.0325938038885,
36.));
#34100=CARTESIAN_POINT('Ctrl Pts',(-18.4250018795219,-67.0960654803447,
36.));
#34101=CARTESIAN_POINT('Ctrl Pts',(-18.4615784793499,-67.1577538950259,
36.));
#34102=CARTESIAN_POINT('Ctrl Pts',(-18.5014131074424,-67.2174209687524,
36.));
#34103=CARTESIAN_POINT('Ctrl Pts',(-18.5319058104575,-67.2630950580072,
36.));
#34104=CARTESIAN_POINT('Ctrl Pts',(-18.5643088135805,-67.3075847482202,
36.));
#34105=CARTESIAN_POINT('Ctrl Pts',(-18.598516631454,-67.3507771468078,36.));
#34106=CARTESIAN_POINT('Ctrl Pts',(-18.6198131995129,-67.3776671945607,
36.));
#34107=CARTESIAN_POINT('Ctrl Pts',(-18.641809612871,-67.4040543069109,36.));
#34108=CARTESIAN_POINT('Ctrl Pts',(-18.6644833259196,-67.4299095535707,
36.));
#34109=CARTESIAN_POINT('Ctrl Pts',(-18.677161402459,-67.4443665944354,36.));
#34110=CARTESIAN_POINT('Ctrl Pts',(-18.6900557042991,-67.4586618783781,
36.));
#34111=CARTESIAN_POINT('Ctrl Pts',(-18.7031386066276,-67.4727649428971,
36.));
#34112=CARTESIAN_POINT('Ctrl Pts',(-18.7540098725322,-67.5276029847322,
36.));
#34113=CARTESIAN_POINT('Ctrl Pts',(-18.8077776801803,-67.5795960840031,
36.));
#34114=CARTESIAN_POINT('Ctrl Pts',(-18.8641570822702,-67.6284803205922,
36.));
#34115=CARTESIAN_POINT('Ctrl Pts',(-18.9063166745294,-67.6650351510109,
36.));
#34116=CARTESIAN_POINT('Ctrl Pts',(-18.9499377755388,-67.6998513681333,
36.));
#34117=CARTESIAN_POINT('Ctrl Pts',(-18.9949176240316,-67.7328088704017,
36.));
#34118=CARTESIAN_POINT('Ctrl Pts',(-19.0089812695787,-67.7431135433954,
36.));
#34119=CARTESIAN_POINT('Ctrl Pts',(-19.0231778384453,-67.7532364320782,
36.));
#34120=CARTESIAN_POINT('Ctrl Pts',(-19.0375044310318,-67.7631736385769,
36.));
#34121=CARTESIAN_POINT('Ctrl Pts',(-19.0512937947226,-67.7727382125433,
36.));
#34122=CARTESIAN_POINT('Ctrl Pts',(-19.0651965725833,-67.7821258221753,
36.));
#34123=CARTESIAN_POINT('Ctrl Pts',(-19.0792048052933,-67.7913302509702,
36.));
#34124=CARTESIAN_POINT('Ctrl Pts',(-19.1421585203574,-67.8326954252703,
36.));
#34125=CARTESIAN_POINT('Ctrl Pts',(-19.2072696868205,-67.870384921608,36.));
#34126=CARTESIAN_POINT('Ctrl Pts',(-19.2742770195005,-67.9041195716521,
36.));
#34127=CARTESIAN_POINT('Ctrl Pts',(-19.3255044410234,-67.9299098705436,
36.));
#34128=CARTESIAN_POINT('Ctrl Pts',(-19.3778410840131,-67.9533882828924,
36.));
#34129=CARTESIAN_POINT('Ctrl Pts',(-19.431184066025,-67.9744148140802,36.));
#34130=CARTESIAN_POINT('Ctrl Pts',(-19.4436313126694,-67.9793212218193,
36.));
#34131=CARTESIAN_POINT('Ctrl Pts',(-19.4561333979725,-67.9840940592263,
36.));
#34132=CARTESIAN_POINT('Ctrl Pts',(-19.4686883835207,-67.9887339150381,
36.));
#34133=CARTESIAN_POINT('Ctrl Pts',(-21.6673174954184,-66.0013023234915,
34.8714803633902));
#34134=CARTESIAN_POINT('Ctrl Pts',(-21.6680517811035,-66.0867862312482,
34.8772098489549));
#34135=CARTESIAN_POINT('Ctrl Pts',(-21.6620451624345,-66.1721666114135,
34.8829393345197));
#34136=CARTESIAN_POINT('Ctrl Pts',(-21.6489385970892,-66.2564427278022,
34.8886688200844));
#34137=CARTESIAN_POINT('Ctrl Pts',(-21.5641972210077,-66.8013356028936,
34.9257131927483));
#34138=CARTESIAN_POINT('Ctrl Pts',(-21.1826528240559,-67.3000663249856,
34.9627575654121));
#34139=CARTESIAN_POINT('Ctrl Pts',(-20.678907038636,-67.5244143934905,34.999801938076));
#34140=CARTESIAN_POINT('Ctrl Pts',(-20.1751612532161,-67.7487624619954,
35.0368463107398));
#34141=CARTESIAN_POINT('Ctrl Pts',(-19.549214079328,-67.6987278769132,35.0738906834037));
#34142=CARTESIAN_POINT('Ctrl Pts',(-19.0875124433194,-67.3971905161154,
35.1109350560675));
#34143=CARTESIAN_POINT('Ctrl Pts',(-18.6258108073107,-67.0956531553176,
35.1479794287314));
#34144=CARTESIAN_POINT('Ctrl Pts',(-18.3283547091814,-66.5426130188043,
35.1850238013952));
#34145=CARTESIAN_POINT('Ctrl Pts',(-18.3312635585425,-65.9911859178142,
35.2220681740591));
#34146=CARTESIAN_POINT('Ctrl Pts',(-18.3341724079037,-65.4397588168241,
35.2591125467229));
#34147=CARTESIAN_POINT('Ctrl Pts',(-18.6374462047552,-64.8899447513572,
35.2961569193868));
#34148=CARTESIAN_POINT('Ctrl Pts',(-19.1023055859304,-64.5932821441991,
35.3332012920506));
#34149=CARTESIAN_POINT('Ctrl Pts',(-19.5671649671057,-64.296619537041,35.3702456647145));
#34150=CARTESIAN_POINT('Ctrl Pts',(-20.1936099326047,-64.2531083881916,
35.4072900373783));
#34151=CARTESIAN_POINT('Ctrl Pts',(-20.6949575817528,-64.4827944770596,
35.4443344100422));
#34152=CARTESIAN_POINT('Ctrl Pts',(-21.1963052309008,-64.7124805659277,
35.4813787827061));
#34153=CARTESIAN_POINT('Ctrl Pts',(-21.5725555636978,-65.2153638925131,
35.5184231553699));
#34154=CARTESIAN_POINT('Ctrl Pts',(-21.6515476257557,-65.7610474007137,
35.5554675280338));
#34155=CARTESIAN_POINT('Ctrl Pts',(-21.6629293534267,-65.8396732894808,
35.5608051398192));
#34156=CARTESIAN_POINT('Ctrl Pts',(-21.6681396849502,-65.9191877552933,
35.5661427516047));
#34157=CARTESIAN_POINT('Ctrl Pts',(-21.6674773009859,-65.998786811783,35.5714803633902));
#34158=CARTESIAN_POINT('Ctrl Pts',(-20.5301702171885,-67.9851743256717,
36.));
#34159=CARTESIAN_POINT('Ctrl Pts',(-21.190259562418,-67.8088876857537,35.9629556273362));
#34160=CARTESIAN_POINT('Ctrl Pts',(-22.3092726893092,-66.7486255815858,
35.8888668820085));
#34161=CARTESIAN_POINT('Ctrl Pts',(-21.8813252557512,-64.4618791315732,
35.7777337640169));
#34162=CARTESIAN_POINT('Ctrl Pts',(-19.7281828815708,-63.5871681688473,
35.6666006460254));
#34163=CARTESIAN_POINT('Ctrl Pts',(-17.825468300226,-64.9187027300962,35.5554675280337));
#34164=CARTESIAN_POINT('Ctrl Pts',(-17.9121446998427,-67.2409164611445,
35.4443344100422));
#34165=CARTESIAN_POINT('Ctrl Pts',(-19.9101226099192,-68.4268768260922,
35.3332012920507));
#34166=CARTESIAN_POINT('Ctrl Pts',(-21.9901521335571,-67.3919236495908,
35.2220681740591));
#34167=CARTESIAN_POINT('Ctrl Pts',(-22.2488202686706,-65.0828969400198,
35.1109350560676));
#34168=CARTESIAN_POINT('Ctrl Pts',(-20.4492273324997,-63.61330436034,34.9998019380759));
#34169=CARTESIAN_POINT('Ctrl Pts',(-18.2385100652431,-64.3280768123671,
34.8886688200844));
#34170=CARTESIAN_POINT('Ctrl Pts',(-17.6399645748577,-66.5730756011264,
34.7775357020929));
#34171=CARTESIAN_POINT('Ctrl Pts',(-19.2014229874425,-68.2935648037488,
34.6664025841013));
#34172=CARTESIAN_POINT('Ctrl Pts',(-21.4937672075293,-67.9148973568499,
34.5552694661097));
#34173=CARTESIAN_POINT('Ctrl Pts',(-22.4189585433245,-65.7836384066037,
34.4441363481182));
#34174=CARTESIAN_POINT('Ctrl Pts',(-21.1302229793561,-63.8504031421106,
34.3330032301266));
#34175=CARTESIAN_POINT('Ctrl Pts',(-18.8070632766386,-63.8845630078765,
34.221870112135));
#34176=CARTESIAN_POINT('Ctrl Pts',(-17.5757260074789,-65.8548543331223,
34.1107369941435));
#34177=CARTESIAN_POINT('Ctrl Pts',(-18.5631798196893,-67.9579885544186,
33.9996038761519));
#34178=CARTESIAN_POINT('Ctrl Pts',(-20.8656679609891,-68.2690946508119,
33.8884707581604));
#34179=CARTESIAN_POINT('Ctrl Pts',(-22.3758627384251,-66.5034359790957,
33.7773376401688));
#34180=CARTESIAN_POINT('Ctrl Pts',(-21.7115744113714,-64.2770129008106,
33.6662045221773));
#34181=CARTESIAN_POINT('Ctrl Pts',(-19.4807858227571,-63.6275354235162,
33.5550714041857));
#34182=CARTESIAN_POINT('Ctrl Pts',(-17.7252024818967,-65.1494309100778,
33.4439382861942));
#34183=CARTESIAN_POINT('Ctrl Pts',(-18.0516033664323,-67.4498007037218,
33.3328051682026));
#34184=CARTESIAN_POINT('Ctrl Pts',(-20.1612535373157,-68.4232558307668,
33.221672050211));
#34185=CARTESIAN_POINT('Ctrl Pts',(-22.1233181243905,-67.1788518425491,
33.1105389322194));
#34186=CARTESIAN_POINT('Ctrl Pts',(-22.1420383908254,-64.8555162491372,
32.9994058142279));
#34187=CARTESIAN_POINT('Ctrl Pts',(-20.2002808122731,-63.5796572308245,
32.8882726962363));
#34188=CARTESIAN_POINT('Ctrl Pts',(-18.0752183512995,-64.5189911786904,
32.7771395782448));
#34189=CARTESIAN_POINT('Ctrl Pts',(-17.7117918139106,-66.8138026917249,
32.6660064602532));
#34190=CARTESIAN_POINT('Ctrl Pts',(-19.442623471414,-68.3637899503476,32.5548733422617));
#34191=CARTESIAN_POINT('Ctrl Pts',(-21.6835880660123,-67.7503436085379,
32.4437402242701));
#34192=CARTESIAN_POINT('Ctrl Pts',(-22.3836665972123,-65.5349139033455,
32.3326071062786));
#34193=CARTESIAN_POINT('Ctrl Pts',(-20.9021196384422,-63.7451492994194,
32.221473988287));
#34194=CARTESIAN_POINT('Ctrl Pts',(-18.594917279486,-64.0191128067246,32.1103408702954));
#34195=CARTESIAN_POINT('Ctrl Pts',(-17.5737019298616,-66.106062240275,31.9992077523039));
#34196=CARTESIAN_POINT('Ctrl Pts',(-18.7731300721891,-68.0959393369569,
31.8880746343123));
#34197=CARTESIAN_POINT('Ctrl Pts',(-21.095437861579,-68.1675302570873,31.7769415163208));
#34198=CARTESIAN_POINT('Ctrl Pts',(-22.4151578040377,-66.2553121727719,
31.6658083983292));
#34199=CARTESIAN_POINT('Ctrl Pts',(-21.5244302645563,-64.1094223389464,
31.5546752803376));
#34200=CARTESIAN_POINT('Ctrl Pts',(-19.2384841459624,-63.6938635929289,
31.4435421623461));
#34201=CARTESIAN_POINT('Ctrl Pts',(-17.6495073099557,-65.3889716553072,
31.3324090443545));
#34202=CARTESIAN_POINT('Ctrl Pts',(-18.2117938983683,-67.6433169085898,
31.221275926363));
#34203=CARTESIAN_POINT('Ctrl Pts',(-20.4107170941006,-68.3936338468077,
31.1101428083714));
#34204=CARTESIAN_POINT('Ctrl Pts',(-22.2337358396447,-66.9532028759171,
30.9990096903798));
#34205=CARTESIAN_POINT('Ctrl Pts',(-22.0123516257601,-64.6403631152875,
30.8878765723883));
#34206=CARTESIAN_POINT('Ctrl Pts',(-19.9491839985917,-63.5719165463332,
30.7767434543967));
#34207=CARTESIAN_POINT('Ctrl Pts',(-17.9325251760105,-64.7257475226081,
30.6656103364052));
#34208=CARTESIAN_POINT('Ctrl Pts',(-17.8081006873606,-67.0458245202808,
30.5544772184136));
#34209=CARTESIAN_POINT('Ctrl Pts',(-19.6897887219546,-68.4087217537406,
30.443344100422));
#34210=CARTESIAN_POINT('Ctrl Pts',(-21.8553943280126,-67.5670620318125,
30.3322109824305));
#34211=CARTESIAN_POINT('Ctrl Pts',(-22.3228700174644,-65.2911654594091,
30.221077864439));
#34212=CARTESIAN_POINT('Ctrl Pts',(-20.6643636396598,-63.6640221580101,
30.1099447464473));
#34213=CARTESIAN_POINT('Ctrl Pts',(-18.3978055097405,-64.1748577207922,
29.9988116284558));
#34214=CARTESIAN_POINT('Ctrl Pts',(-17.5976388390673,-66.3561353344053,
29.8876785104642));
#34215=CARTESIAN_POINT('Ctrl Pts',(-18.9962076588936,-68.2114638726205,
29.7765453924727));
#34216=CARTESIAN_POINT('Ctrl Pts',(-21.313486738182,-68.0427736322436,29.6654122744811));
#34217=CARTESIAN_POINT('Ctrl Pts',(-22.4286110563519,-66.0044565608507,
29.5542791564895));
#34218=CARTESIAN_POINT('Ctrl Pts',(-21.320974946549,-63.9620606695586,29.4431460384981));
#34219=CARTESIAN_POINT('Ctrl Pts',(-19.004330572597,-63.784867065997,29.3320129205064));
#34220=CARTESIAN_POINT('Ctrl Pts',(-17.5989620477711,-65.6350503104176,
29.2208798025149));
#34221=CARTESIAN_POINT('Ctrl Pts',(-18.391117960758,-67.8192498750237,29.1097466845233));
#34222=CARTESIAN_POINT('Ctrl Pts',(-20.6557860410391,-68.3384003490309,
28.9986135665318));
#34223=CARTESIAN_POINT('Ctrl Pts',(-22.3202529250742,-66.7173547850641,
28.8874804485402));
#34224=CARTESIAN_POINT('Ctrl Pts',(-21.8611330078161,-64.4397578869974,
28.7763473305487));
#34225=CARTESIAN_POINT('Ctrl Pts',(-19.6986309083236,-63.5901559812818,
28.6652142125571));
#34226=CARTESIAN_POINT('Ctrl Pts',(-17.8119536633046,-64.9461381720334,
28.5540810945656));
#34227=CARTESIAN_POINT('Ctrl Pts',(-17.9278625462951,-67.2666561873374,
28.4429479765739));
#34228=CARTESIAN_POINT('Ctrl Pts',(-19.9402731854491,-68.4278806048883,
28.3318148585824));
#34229=CARTESIAN_POINT('Ctrl Pts',(-22.0073481561099,-67.3670131323966,
28.2206817405908));
#34230=CARTESIAN_POINT('Ctrl Pts',(-22.2372190858348,-65.0550014360215,
28.1095486225993));
#34231=CARTESIAN_POINT('Ctrl Pts',(-20.4194990521396,-63.6078896201836,
27.9984155046077));
#34232=CARTESIAN_POINT('Ctrl Pts',(-18.2178369745624,-64.3501313764944,
27.8872823866162));
#34233=CARTESIAN_POINT('Ctrl Pts',(-17.6472806432027,-66.6023978352466,
27.7761492686246));
#34234=CARTESIAN_POINT('Ctrl Pts',(-19.2300256691482,-68.3033260850074,
27.665016150633));
#34235=CARTESIAN_POINT('Ctrl Pts',(-21.5174815089169,-67.89615964379,27.5538830326415));
#34236=CARTESIAN_POINT('Ctrl Pts',(-22.4160785435702,-65.7535532643562,
27.4427499146499));
#34237=CARTESIAN_POINT('Ctrl Pts',(-21.1033854005481,-63.836504637639,27.3316167966584));
#34238=CARTESIAN_POINT('Ctrl Pts',(-18.7808305074767,-63.8995721204905,
27.2204836786668));
#34239=CARTESIAN_POINT('Ctrl Pts',(-17.5741075252728,-65.8850338715259,
27.1093505606753));
#34240=CARTESIAN_POINT('Ctrl Pts',(-18.5876568076359,-67.9757171467262,
26.9982174426837));
#34241=CARTESIAN_POINT('Ctrl Pts',(-20.8938381898737,-68.2581463290383,
26.8870843246921));
#34242=CARTESIAN_POINT('Ctrl Pts',(-22.3819436378662,-66.4738311047313,
26.7759512067006));
#34243=CARTESIAN_POINT('Ctrl Pts',(-21.6900005993275,-64.2558470165435,
26.664818088709));
#34244=CARTESIAN_POINT('Ctrl Pts',(-19.4513023285576,-63.6341803621276,
26.5536849707175));
#34245=CARTESIAN_POINT('Ctrl Pts',(-17.7147940941022,-65.1778050096466,
26.4425518527259));
#34246=CARTESIAN_POINT('Ctrl Pts',(-18.0697955898292,-67.4739347707333,
26.3314187347343));
#34247=CARTESIAN_POINT('Ctrl Pts',(-20.1913974492333,-68.4210616212703,
26.2202856167428));
#34248=CARTESIAN_POINT('Ctrl Pts',(-22.1378222071026,-67.1523371749621,
26.1091524987513));
#34249=CARTESIAN_POINT('Ctrl Pts',(-22.1276331663505,-64.8289492060639,
25.9980193807597));
#34250=CARTESIAN_POINT('Ctrl Pts',(-20.1701400827706,-63.5773513899392,
25.8868862627681));
#34251=CARTESIAN_POINT('Ctrl Pts',(-18.0569488868988,-64.5430601781429,
25.7757531447766));
#34252=CARTESIAN_POINT('Ctrl Pts',(-17.7220730992874,-66.842211172105,25.664620026785));
#34253=CARTESIAN_POINT('Ctrl Pts',(-19.4721283107045,-68.3705502400566,
25.5534869087934));
#34254=CARTESIAN_POINT('Ctrl Pts',(-21.7051476952021,-67.7292427278489,
25.4423537908019));
#34255=CARTESIAN_POINT('Ctrl Pts',(-22.3778773330212,-65.5053154469377,
25.3312206728103));
#34256=CARTESIAN_POINT('Ctrl Pts',(-20.8736249251117,-63.7340407352631,
25.2200875548188));
#34257=CARTESIAN_POINT('Ctrl Pts',(-18.5711036444345,-64.0368654665697,
25.1089544368272));
#34258=CARTESIAN_POINT('Ctrl Pts',(-17.573747567038,-66.1360134381725,24.9978213188356));
#34259=CARTESIAN_POINT('Ctrl Pts',(-18.8023455421979,-68.1115881261982,
24.8866882008441));
#34260=CARTESIAN_POINT('Ctrl Pts',(-20.343660854084,-68.1379171412778,24.8125994555164));
#34261=CARTESIAN_POINT('Ctrl Pts',(-20.9495535522615,-67.8221815534923,
24.7755550828525));
#34262=CARTESIAN_POINT('Ctrl Pts',(-20.4967348970876,-67.8599788000028,
36.0748149723825));
#34263=CARTESIAN_POINT('Ctrl Pts',(-21.1151955392376,-67.6948097220377,
36.0377705997186));
#34264=CARTESIAN_POINT('Ctrl Pts',(-22.1636378175943,-66.7014133181569,
35.9636818543909));
#34265=CARTESIAN_POINT('Ctrl Pts',(-21.7626789981897,-64.5588811168271,
35.8525487363994));
#34266=CARTESIAN_POINT('Ctrl Pts',(-19.7453250975402,-63.7393340242815,
35.7414156184078));
#34267=CARTESIAN_POINT('Ctrl Pts',(-17.9626056970361,-64.9868950184809,
35.6302825004163));
#34268=CARTESIAN_POINT('Ctrl Pts',(-18.0438158273823,-67.162657747713,35.5191493824247));
#34269=CARTESIAN_POINT('Ctrl Pts',(-19.9157907504706,-68.2738252194664,
35.4080162644331));
#34270=CARTESIAN_POINT('Ctrl Pts',(-21.864642681163,-67.3041416292674,35.2968831464415));
#34271=CARTESIAN_POINT('Ctrl Pts',(-22.1069978442969,-65.1407342786364,
35.1857500284501));
#34272=CARTESIAN_POINT('Ctrl Pts',(-20.4208966960866,-63.763821930185,35.0746169104584));
#34273=CARTESIAN_POINT('Ctrl Pts',(-18.3495988776918,-64.4335170750418,
34.9634837924669));
#34274=CARTESIAN_POINT('Ctrl Pts',(-17.7888008114678,-66.5369344420336,
34.8523506744753));
#34275=CARTESIAN_POINT('Ctrl Pts',(-19.2517854506183,-68.148920553847,34.7412175564838));
#34276=CARTESIAN_POINT('Ctrl Pts',(-21.3995623972236,-67.7941338661616,
34.6300844384922));
#34277=CARTESIAN_POINT('Ctrl Pts',(-22.266406305223,-65.797283305729,34.5189513205006));
#34278=CARTESIAN_POINT('Ctrl Pts',(-21.0589451786139,-63.9859680167513,
34.4078182025091));
#34279=CARTESIAN_POINT('Ctrl Pts',(-18.8822961356574,-64.0179735818617,
34.2966850845175));
#34280=CARTESIAN_POINT('Ctrl Pts',(-17.7286134657411,-65.86400798166,34.185551966526));
#34281=CARTESIAN_POINT('Ctrl Pts',(-18.6537932511848,-67.8345075063544,
34.0744188485344));
#34282=CARTESIAN_POINT('Ctrl Pts',(-20.811074390022,-68.1259936173523,33.9632857305429));
#34283=CARTESIAN_POINT('Ctrl Pts',(-22.226028348262,-66.4716866605454,33.8521526125513));
#34284=CARTESIAN_POINT('Ctrl Pts',(-21.6036335341486,-64.3856735221044,
33.7410194945598));
#34285=CARTESIAN_POINT('Ctrl Pts',(-19.5135301974017,-63.7771555077289,
33.6298863765682));
#34286=CARTESIAN_POINT('Ctrl Pts',(-17.868663168138,-65.2030722668864,33.5187532585766));
#34287=CARTESIAN_POINT('Ctrl Pts',(-18.1744794975593,-67.3583686522034,
33.4076201405851));
#34288=CARTESIAN_POINT('Ctrl Pts',(-20.1510840418164,-68.2704325831357,
33.2964870225935));
#34289=CARTESIAN_POINT('Ctrl Pts',(-21.9894105247868,-67.1045072501346,
33.185353904602));
#34290=CARTESIAN_POINT('Ctrl Pts',(-22.0069501928397,-64.9276934090752,
33.0742207866104));
#34291=CARTESIAN_POINT('Ctrl Pts',(-20.1876500517149,-63.7322967654826,
32.9630876686188));
#34292=CARTESIAN_POINT('Ctrl Pts',(-18.1966051973769,-64.612391378112,32.8519545506273));
#34293=CARTESIAN_POINT('Ctrl Pts',(-17.8560982473522,-66.7624800172052,
32.7408214326357));
#34294=CARTESIAN_POINT('Ctrl Pts',(-19.477774564489,-68.2147169336469,32.6296883146442));
#34295=CARTESIAN_POINT('Ctrl Pts',(-21.5774121548046,-67.6399577419979,
32.5185551966526));
#34296=CARTESIAN_POINT('Ctrl Pts',(-22.2333400547025,-65.5642446767688,
32.4074220786611));
#34297=CARTESIAN_POINT('Ctrl Pts',(-20.8452272331302,-63.8873520345212,
32.2962889606695));
#34298=CARTESIAN_POINT('Ctrl Pts',(-18.6835291799767,-64.1440379632945,
32.1851558426779));
#34299=CARTESIAN_POINT('Ctrl Pts',(-17.7267170370955,-66.0993733980141,
32.0740227246864));
#34300=CARTESIAN_POINT('Ctrl Pts',(-18.8505029374097,-67.9637583875726,
31.9628896066948));
#34301=CARTESIAN_POINT('Ctrl Pts',(-21.0263537931702,-68.0308344080476,
31.8517564887032));
#34302=CARTESIAN_POINT('Ctrl Pts',(-22.2628452605296,-66.2392108454141,
31.7406233707117));
#34303=CARTESIAN_POINT('Ctrl Pts',(-21.4282916807308,-64.2286521018105,
31.6294902527201));
#34304=CARTESIAN_POINT('Ctrl Pts',(-19.2865093377144,-63.8393006742038,
31.5183571347286));
#34305=CARTESIAN_POINT('Ctrl Pts',(-17.7977417315406,-65.4275063138625,
31.407224016737));
#34306=CARTESIAN_POINT('Ctrl Pts',(-18.3245675727016,-67.5396807082061,
31.2960908987455));
#34307=CARTESIAN_POINT('Ctrl Pts',(-20.3848151157039,-68.2426787171575,
31.1849577807539));
#34308=CARTESIAN_POINT('Ctrl Pts',(-22.0928647186386,-66.893088893192,31.0738246627623));
#34309=CARTESIAN_POINT('Ctrl Pts',(-21.8854421567226,-64.726108962541,30.9626915447708));
#34310=CARTESIAN_POINT('Ctrl Pts',(-19.952388722694,-63.725044249235,30.8515584267792));
#34311=CARTESIAN_POINT('Ctrl Pts',(-18.0629110036174,-64.806108580415,30.7404253087877));
#34312=CARTESIAN_POINT('Ctrl Pts',(-17.9463333771102,-66.9798693299075,
30.6292921907961));
#34313=CARTESIAN_POINT('Ctrl Pts',(-19.7093522754023,-68.2568151013876,
30.5181590728045));
#34314=CARTESIAN_POINT('Ctrl Pts',(-21.7383834110292,-67.468234864701,30.407025954813));
#34315=CARTESIAN_POINT('Ctrl Pts',(-22.1763776267779,-65.3358682906789,
30.2958928368214));
#34316=CARTESIAN_POINT('Ctrl Pts',(-20.6224653771108,-63.8113411969967,
30.1847597188298));
#34317=CARTESIAN_POINT('Ctrl Pts',(-18.4988483143134,-64.2899607845943,
30.0736266008383));
#34318=CARTESIAN_POINT('Ctrl Pts',(-17.749144359011,-66.3336755686187,29.9624934828467));
#34319=CARTESIAN_POINT('Ctrl Pts',(-19.0595120791564,-68.071997338901,29.8513603648552));
#34320=CARTESIAN_POINT('Ctrl Pts',(-21.2306513617017,-67.9139455916004,
29.7402272468636));
#34321=CARTESIAN_POINT('Ctrl Pts',(-22.275450080052,-66.0041755067028,29.6290941288721));
#34322=CARTESIAN_POINT('Ctrl Pts',(-21.2376673242963,-64.0905838337245,
29.5179610108805));
#34323=CARTESIAN_POINT('Ctrl Pts',(-19.0671227192333,-63.9245649900093,
29.406827892889));
#34324=CARTESIAN_POINT('Ctrl Pts',(-17.75038411922,-65.6580659557638,29.2956947748974));
#34325=CARTESIAN_POINT('Ctrl Pts',(-18.4925825173148,-67.7045184171959,
29.1845616569058));
#34326=CARTESIAN_POINT('Ctrl Pts',(-20.6144287269369,-68.1909285340192,
29.0734285389143));
#34327=CARTESIAN_POINT('Ctrl Pts',(-22.1739255819875,-66.6721146224013,
28.9622954209227));
#34328=CARTESIAN_POINT('Ctrl Pts',(-21.7437601795258,-64.5381549541881,
28.8511623029312));
#34329=CARTESIAN_POINT('Ctrl Pts',(-19.7176368270306,-63.7421334095621,
28.7400291849396));
#34330=CARTESIAN_POINT('Ctrl Pts',(-17.9499433641425,-65.0126002372679,
28.6288960669481));
#34331=CARTESIAN_POINT('Ctrl Pts',(-18.0585424238354,-67.1867741915022,
28.5177629489565));
#34332=CARTESIAN_POINT('Ctrl Pts',(-19.9440398722572,-68.2747656946963,
28.4066298309649));
#34333=CARTESIAN_POINT('Ctrl Pts',(-21.8807542321633,-67.2808021001998,
28.2954967129733));
#34334=CARTESIAN_POINT('Ctrl Pts',(-22.0961282930185,-65.1145980117196,
28.1843635949818));
#34335=CARTESIAN_POINT('Ctrl Pts',(-20.3930432373172,-63.7587486719991,
28.0732304769902));
#34336=CARTESIAN_POINT('Ctrl Pts',(-18.3302295407528,-64.4541807624518,
27.9620973589987));
#34337=CARTESIAN_POINT('Ctrl Pts',(-17.7956554900948,-66.564407461973,27.8509642410071));
#34338=CARTESIAN_POINT('Ctrl Pts',(-19.2785842968999,-68.1580662374109,
27.7398311230155));
#34339=CARTESIAN_POINT('Ctrl Pts',(-21.4217811501398,-67.7765778517597,
27.628698005024));
#34340=CARTESIAN_POINT('Ctrl Pts',(-22.2637079333885,-65.769095490658,27.5175648870324));
#34341=CARTESIAN_POINT('Ctrl Pts',(-21.0338001185652,-63.9729460250127,
27.4064317690409));
#34342=CARTESIAN_POINT('Ctrl Pts',(-18.85771774278,-64.0320361409567,27.2952986510493));
#34343=CARTESIAN_POINT('Ctrl Pts',(-17.7270970535285,-65.8922842397695,
27.1841655330578));
#34344=CARTESIAN_POINT('Ctrl Pts',(-18.6767265916375,-67.8511180404618,
27.0730324150662));
#34345=CARTESIAN_POINT('Ctrl Pts',(-20.8374680562299,-68.1157357542866,
26.9618992970746));
#34346=CARTESIAN_POINT('Ctrl Pts',(-22.2317257542274,-66.4439488251411,
26.8507661790831));
#34347=CARTESIAN_POINT('Ctrl Pts',(-21.5834202800691,-64.3658424697322,
26.7396330610915));
#34348=CARTESIAN_POINT('Ctrl Pts',(-19.4859060872912,-63.7833813815903,
26.6284999431));
#34349=CARTESIAN_POINT('Ctrl Pts',(-17.858911187977,-65.2296569466219,26.5173668251084));
#34350=CARTESIAN_POINT('Ctrl Pts',(-18.1915244237431,-67.3809806981174,
26.4062337071169));
#34351=CARTESIAN_POINT('Ctrl Pts',(-20.1793269202331,-68.2683767520211,
26.2951005891253));
#34352=CARTESIAN_POINT('Ctrl Pts',(-22.0029999038198,-67.0796647368282,
26.1839674711337));
#34353=CARTESIAN_POINT('Ctrl Pts',(-21.993453437524,-64.902801823356,26.0728343531422));
#34354=CARTESIAN_POINT('Ctrl Pts',(-20.1594101550134,-63.7301363430416,
25.9617012351506));
#34355=CARTESIAN_POINT('Ctrl Pts',(-18.1794879014128,-64.634942459969,25.8505681171591));
#34356=CARTESIAN_POINT('Ctrl Pts',(-17.8657311408418,-66.7890969095174,
25.7394349991675));
#34357=CARTESIAN_POINT('Ctrl Pts',(-19.5054186735571,-68.2210508839594,
25.6283018811759));
#34358=CARTESIAN_POINT('Ctrl Pts',(-21.5976121204752,-67.6201875937367,
25.5171687631844));
#34359=CARTESIAN_POINT('Ctrl Pts',(-22.2279158919356,-65.5365128545709,
25.4060356451928));
#34360=CARTESIAN_POINT('Ctrl Pts',(-20.8185295461707,-63.8769440347993,
25.2949025272013));
#34361=CARTESIAN_POINT('Ctrl Pts',(-18.6612173578994,-64.1606710471141,
25.1837694092097));
#34362=CARTESIAN_POINT('Ctrl Pts',(-17.7267597961517,-66.1274357159696,
25.0726362912181));
#34363=CARTESIAN_POINT('Ctrl Pts',(-18.8778759263437,-67.9784202819252,
24.9615031732266));
#34364=CARTESIAN_POINT('Ctrl Pts',(-20.3219877945836,-68.003088850947,24.8874144278989));
#34365=CARTESIAN_POINT('Ctrl Pts',(-20.8896697150645,-67.7072652086133,
24.850370055235));
#34366=CARTESIAN_POINT('Ctrl Pts',(-20.4632995769867,-67.7347832743338,
36.149629944765));
#34367=CARTESIAN_POINT('Ctrl Pts',(-21.0401315160572,-67.5807317583216,
36.1125855721011));
#34368=CARTESIAN_POINT('Ctrl Pts',(-22.0180029458793,-66.654201054728,36.0384968267735));
#34369=CARTESIAN_POINT('Ctrl Pts',(-21.6440327406283,-64.6558831020808,
35.9273637087818));
#34370=CARTESIAN_POINT('Ctrl Pts',(-19.7624673135096,-63.8914998797159,
35.8162305907903));
#34371=CARTESIAN_POINT('Ctrl Pts',(-18.0997430938463,-65.0550873068655,
35.7050974727987));
#34372=CARTESIAN_POINT('Ctrl Pts',(-18.1754869549219,-67.0843990342815,
35.5939643548072));
#34373=CARTESIAN_POINT('Ctrl Pts',(-19.921458891022,-68.1207736128406,35.4828312368156));
#34374=CARTESIAN_POINT('Ctrl Pts',(-21.7391332287689,-67.2163596089439,
35.3716981188241));
#34375=CARTESIAN_POINT('Ctrl Pts',(-21.9651754199231,-65.198571617253,35.2605650008325));
#34376=CARTESIAN_POINT('Ctrl Pts',(-20.3925660596736,-63.9143395000302,
35.149431882841));
#34377=CARTESIAN_POINT('Ctrl Pts',(-18.4606876901404,-64.5389573377165,
35.0382987648494));
#34378=CARTESIAN_POINT('Ctrl Pts',(-17.937637048078,-66.5007932829407,34.9271656468579));
#34379=CARTESIAN_POINT('Ctrl Pts',(-19.3021479137942,-68.0042763039452,
34.8160325288662));
#34380=CARTESIAN_POINT('Ctrl Pts',(-21.3053575869179,-67.6733703754733,
34.7048994108748));
#34381=CARTESIAN_POINT('Ctrl Pts',(-22.1138540671214,-65.8109282048542,
34.5937662928831));
#34382=CARTESIAN_POINT('Ctrl Pts',(-20.9876673778718,-64.1215328913922,
34.4826331748916));
#34383=CARTESIAN_POINT('Ctrl Pts',(-18.9575289946762,-64.1513841558468,
34.3715000569001));
#34384=CARTESIAN_POINT('Ctrl Pts',(-17.8815009240032,-65.8731616301978,
34.2603669389085));
#34385=CARTESIAN_POINT('Ctrl Pts',(-18.7444066826802,-67.71102645829,34.1492338209169));
#34386=CARTESIAN_POINT('Ctrl Pts',(-20.7564808190548,-67.9828925838928,
34.0381007029253));
#34387=CARTESIAN_POINT('Ctrl Pts',(-22.0761939580989,-66.4399373419952,
33.9269675849338));
#34388=CARTESIAN_POINT('Ctrl Pts',(-21.4956926569258,-64.4943341433981,
33.8158344669422));
#34389=CARTESIAN_POINT('Ctrl Pts',(-19.5462745720463,-63.9267755919416,
33.7047013489507));
#34390=CARTESIAN_POINT('Ctrl Pts',(-18.0121238543792,-65.2567136236949,
33.5935682309591));
#34391=CARTESIAN_POINT('Ctrl Pts',(-18.2973556286862,-67.2669366006852,
33.4824351129676));
#34392=CARTESIAN_POINT('Ctrl Pts',(-20.1409145463171,-68.1176093355045,
33.371301994976));
#34393=CARTESIAN_POINT('Ctrl Pts',(-21.8555029251832,-67.0301626577201,
33.2601688769845));
#34394=CARTESIAN_POINT('Ctrl Pts',(-21.871861994854,-64.9998705690132,33.1490357589928));
#34395=CARTESIAN_POINT('Ctrl Pts',(-20.1750192911566,-63.8849363001409,
33.0379026410013));
#34396=CARTESIAN_POINT('Ctrl Pts',(-18.3179920434542,-64.7057915775334,
32.9267695230098));
#34397=CARTESIAN_POINT('Ctrl Pts',(-18.0004046807938,-66.7111573426855,
32.8156364050182));
#34398=CARTESIAN_POINT('Ctrl Pts',(-19.5129256575641,-68.065643916946,32.7045032870266));
#34399=CARTESIAN_POINT('Ctrl Pts',(-21.4712362435969,-67.529571875458,32.5933701690351));
#34400=CARTESIAN_POINT('Ctrl Pts',(-22.0830135121926,-65.5935754501919,
32.4822370510435));
#34401=CARTESIAN_POINT('Ctrl Pts',(-20.7883348278182,-64.029554769623,32.3711039330519));
#34402=CARTESIAN_POINT('Ctrl Pts',(-18.7721410804674,-64.2689631198643,
32.2599708150604));
#34403=CARTESIAN_POINT('Ctrl Pts',(-17.8797321443293,-66.0926845557532,
32.1488376970689));
#34404=CARTESIAN_POINT('Ctrl Pts',(-18.9278758026304,-67.8315774381883,
32.0377045790773));
#34405=CARTESIAN_POINT('Ctrl Pts',(-20.9572697247615,-67.894138559008,31.9265714610857));
#34406=CARTESIAN_POINT('Ctrl Pts',(-22.1105327170215,-66.2231095180563,
31.8154383430942));
#34407=CARTESIAN_POINT('Ctrl Pts',(-21.3321530969053,-64.3478818646744,
31.7043052251026));
#34408=CARTESIAN_POINT('Ctrl Pts',(-19.3345345294663,-63.9847377554787,
31.593172107111));
#34409=CARTESIAN_POINT('Ctrl Pts',(-17.9459761531255,-65.4660409724177,
31.4820389891195));
#34410=CARTESIAN_POINT('Ctrl Pts',(-18.437341247035,-67.4360445078226,31.3709058711279));
#34411=CARTESIAN_POINT('Ctrl Pts',(-20.3589131373073,-68.0917235875072,
31.2597727531364));
#34412=CARTESIAN_POINT('Ctrl Pts',(-21.9519935976325,-66.832974910467,31.1486396351448));
#34413=CARTESIAN_POINT('Ctrl Pts',(-21.7585326876851,-64.8118548097944,
31.0375065171533));
#34414=CARTESIAN_POINT('Ctrl Pts',(-19.9555934467963,-63.8781719521369,
30.9263733991617));
#34415=CARTESIAN_POINT('Ctrl Pts',(-18.1932968312243,-64.8864696382219,
30.8152402811701));
#34416=CARTESIAN_POINT('Ctrl Pts',(-18.0845660668597,-66.913914139534,30.7041071631786));
#34417=CARTESIAN_POINT('Ctrl Pts',(-19.72891582885,-68.1049084490347,30.592974045187));
#34418=CARTESIAN_POINT('Ctrl Pts',(-21.6213724940458,-67.3694076975895,
30.4818409271954));
#34419=CARTESIAN_POINT('Ctrl Pts',(-22.0298852360914,-65.3805711219487,
30.3707078092039));
#34420=CARTESIAN_POINT('Ctrl Pts',(-20.5805671145618,-63.9586602359834,
30.2595746912123));
#34421=CARTESIAN_POINT('Ctrl Pts',(-18.5998911188863,-64.4050638483964,
30.1484415732208));
#34422=CARTESIAN_POINT('Ctrl Pts',(-17.9006498789546,-66.3112158028321,
30.0373084552292));
#34423=CARTESIAN_POINT('Ctrl Pts',(-19.1228164994193,-67.9325308051813,
29.9261753372377));
#34424=CARTESIAN_POINT('Ctrl Pts',(-21.1478159852215,-67.7851175509572,
29.8150422192461));
#34425=CARTESIAN_POINT('Ctrl Pts',(-22.1222891037521,-66.003894452555,29.7039091012546));
#34426=CARTESIAN_POINT('Ctrl Pts',(-21.1543597020436,-64.2191069978902,
29.592775983263));
#34427=CARTESIAN_POINT('Ctrl Pts',(-19.1299148658697,-64.0642629140219,
29.4816428652715));
#34428=CARTESIAN_POINT('Ctrl Pts',(-17.9018061906689,-65.68108160111,29.3705097472798));
#34429=CARTESIAN_POINT('Ctrl Pts',(-18.5940470738716,-67.589786959368,29.2593766292883));
#34430=CARTESIAN_POINT('Ctrl Pts',(-20.5730714128348,-68.0434567190076,
29.1482435112967));
#34431=CARTESIAN_POINT('Ctrl Pts',(-22.0275982389007,-66.6268744597386,
29.0371103933052));
#34432=CARTESIAN_POINT('Ctrl Pts',(-21.6263873512355,-64.6365520213787,
28.9259772753136));
#34433=CARTESIAN_POINT('Ctrl Pts',(-19.7366427457375,-63.8941108378424,
28.8148441573221));
#34434=CARTESIAN_POINT('Ctrl Pts',(-18.0879330649805,-65.0790623025024,
28.7037110393305));
#34435=CARTESIAN_POINT('Ctrl Pts',(-18.1892223013757,-67.106892195667,28.592577921339));
#34436=CARTESIAN_POINT('Ctrl Pts',(-19.9478065590653,-68.1216507845045,
28.4814448033474));
#34437=CARTESIAN_POINT('Ctrl Pts',(-21.7541603082167,-67.194591068003,28.3703116853558));
#34438=CARTESIAN_POINT('Ctrl Pts',(-21.9550375002021,-65.1741945874176,
28.2591785673643));
#34439=CARTESIAN_POINT('Ctrl Pts',(-20.3665874224948,-63.9096077238146,
28.1480454493727));
#34440=CARTESIAN_POINT('Ctrl Pts',(-18.4426221069431,-64.5582301484091,
28.0369123313812));
#34441=CARTESIAN_POINT('Ctrl Pts',(-17.9440303369869,-66.5264170886993,
27.9257792133896));
#34442=CARTESIAN_POINT('Ctrl Pts',(-19.3271429246517,-68.0128063898144,
27.814646095398));
#34443=CARTESIAN_POINT('Ctrl Pts',(-21.3260807913628,-67.6569960597292,
27.7035129774065));
#34444=CARTESIAN_POINT('Ctrl Pts',(-22.1113373232067,-65.78463771696,27.5923798594149));
#34445=CARTESIAN_POINT('Ctrl Pts',(-20.9642148365823,-64.1093874123863,
27.4812467414234));
#34446=CARTESIAN_POINT('Ctrl Pts',(-18.9346049780834,-64.164500161423,27.3701136234318));
#34447=CARTESIAN_POINT('Ctrl Pts',(-17.8800865817842,-65.8995346080128,
27.2589805054402));
#34448=CARTESIAN_POINT('Ctrl Pts',(-18.765796375639,-67.7265189341975,27.1478473874487));
#34449=CARTESIAN_POINT('Ctrl Pts',(-20.7810979225862,-67.9733251795348,
27.0367142694571));
#34450=CARTESIAN_POINT('Ctrl Pts',(-22.0815078705886,-66.4140665455509,
26.9255811514656));
#34451=CARTESIAN_POINT('Ctrl Pts',(-21.4768399608107,-64.4758379229209,
26.814448033474));
#34452=CARTESIAN_POINT('Ctrl Pts',(-19.5205098460247,-63.932582401053,26.7033149154824));
#34453=CARTESIAN_POINT('Ctrl Pts',(-18.0030282818518,-65.2815088835971,
26.5921817974909));
#34454=CARTESIAN_POINT('Ctrl Pts',(-18.313253257657,-67.2880266255015,26.4810486794993));
#34455=CARTESIAN_POINT('Ctrl Pts',(-20.1672563912329,-68.115691882772,26.3699155615078));
#34456=CARTESIAN_POINT('Ctrl Pts',(-21.868177600537,-67.0069922986945,26.2587824435162));
#34457=CARTESIAN_POINT('Ctrl Pts',(-21.8592737086975,-64.976654440648,26.1476493255247));
#34458=CARTESIAN_POINT('Ctrl Pts',(-20.1486802272563,-63.882921296144,26.0365162075331));
#34459=CARTESIAN_POINT('Ctrl Pts',(-18.3020269159268,-64.7268247417951,
25.9253830895415));
#34460=CARTESIAN_POINT('Ctrl Pts',(-18.0093891823963,-66.7359826469298,
25.81424997155));
#34461=CARTESIAN_POINT('Ctrl Pts',(-19.5387090364096,-68.0715515278622,
25.7031168535584));
#34462=CARTESIAN_POINT('Ctrl Pts',(-21.4900765457484,-67.5111324596245,
25.5919837355669));
#34463=CARTESIAN_POINT('Ctrl Pts',(-22.07795445085,-65.5677102622041,25.4808506175753));
#34464=CARTESIAN_POINT('Ctrl Pts',(-20.7634341672297,-64.0198473343356,
25.3697174995838));
#34465=CARTESIAN_POINT('Ctrl Pts',(-18.7513310713643,-64.2844766276586,
25.2585843815922));
#34466=CARTESIAN_POINT('Ctrl Pts',(-17.8797720252654,-66.1188579937667,
25.1474512636006));
#34467=CARTESIAN_POINT('Ctrl Pts',(-18.9534063104895,-67.8452524376522,
25.0363181456091));
#34468=CARTESIAN_POINT('Ctrl Pts',(-20.3003147350832,-67.8682605606162,
24.9622294002814));
#34469=CARTESIAN_POINT('Ctrl Pts',(-20.8297858778675,-67.5923488637344,
24.9251850276175));
#34470=CARTESIAN_POINT('Ctrl Pts',(-20.4298642568858,-67.6095877486649,
36.2244449171475));
#34471=CARTESIAN_POINT('Ctrl Pts',(-20.9650674928767,-67.4666537946055,
36.1874005444836));
#34472=CARTESIAN_POINT('Ctrl Pts',(-21.8723680741644,-66.6069887912992,
36.113311799156));
#34473=CARTESIAN_POINT('Ctrl Pts',(-21.5253864830668,-64.7528850873347,
36.0021786811643));
#34474=CARTESIAN_POINT('Ctrl Pts',(-19.779609529479,-64.04366573515,35.8910455631728));
#34475=CARTESIAN_POINT('Ctrl Pts',(-18.2368804906565,-65.1232795952502,
35.7799124451812));
#34476=CARTESIAN_POINT('Ctrl Pts',(-18.3071580824616,-67.0061403208501,
35.6687793271897));
#34477=CARTESIAN_POINT('Ctrl Pts',(-19.9271270315734,-67.9677220062147,
35.5576462091981));
#34478=CARTESIAN_POINT('Ctrl Pts',(-21.6136237763748,-67.1285775886206,
35.4465130912065));
#34479=CARTESIAN_POINT('Ctrl Pts',(-21.8233529955495,-65.2564089558696,
35.335379973215));
#34480=CARTESIAN_POINT('Ctrl Pts',(-20.3642354232605,-64.0648570698753,
35.2242468552234));
#34481=CARTESIAN_POINT('Ctrl Pts',(-18.5717765025891,-64.6443976003911,
35.1131137372319));
#34482=CARTESIAN_POINT('Ctrl Pts',(-18.0864732846881,-66.4646521238479,
35.0019806192403));
#34483=CARTESIAN_POINT('Ctrl Pts',(-19.35251037697,-67.8596320540434,34.8908475012488));
#34484=CARTESIAN_POINT('Ctrl Pts',(-21.2111527766122,-67.552606884785,34.7797143832572));
#34485=CARTESIAN_POINT('Ctrl Pts',(-21.9613018290199,-65.8245731039795,
34.6685812652656));
#34486=CARTESIAN_POINT('Ctrl Pts',(-20.9163895771297,-64.2570977660329,
34.5574481472741));
#34487=CARTESIAN_POINT('Ctrl Pts',(-19.0327618536951,-64.284794729832,34.4463150292825));
#34488=CARTESIAN_POINT('Ctrl Pts',(-18.0343883822654,-65.8823152787355,
34.335181911291));
#34489=CARTESIAN_POINT('Ctrl Pts',(-18.8350201141757,-67.5875454102258,
34.2240487932994));
#34490=CARTESIAN_POINT('Ctrl Pts',(-20.7018872480875,-67.8397915504332,
34.1129156753078));
#34491=CARTESIAN_POINT('Ctrl Pts',(-21.9263595679359,-66.4081880234449,
34.0017825573163));
#34492=CARTESIAN_POINT('Ctrl Pts',(-21.387751779703,-64.6029947646918,33.8906494393247));
#34493=CARTESIAN_POINT('Ctrl Pts',(-19.579018946691,-64.0763956761543,33.7795163213332));
#34494=CARTESIAN_POINT('Ctrl Pts',(-18.1555845406205,-65.3103549805034,
33.6683832033416));
#34495=CARTESIAN_POINT('Ctrl Pts',(-18.4202317598132,-67.1755045491668,
33.5572500853501));
#34496=CARTESIAN_POINT('Ctrl Pts',(-20.1307450508178,-67.9647860878732,
33.4461169673584));
#34497=CARTESIAN_POINT('Ctrl Pts',(-21.7215953255795,-66.9558180653057,
33.334983849367));
#34498=CARTESIAN_POINT('Ctrl Pts',(-21.7367737968683,-65.0720477289512,
33.2238507313753));
#34499=CARTESIAN_POINT('Ctrl Pts',(-20.1623885305984,-64.0375758347992,
33.1127176133839));
#34500=CARTESIAN_POINT('Ctrl Pts',(-18.4393788895316,-64.7991917769549,
33.0015844953922));
#34501=CARTESIAN_POINT('Ctrl Pts',(-18.1447111142353,-66.6598346681659,
32.8904513774007));
#34502=CARTESIAN_POINT('Ctrl Pts',(-19.5480767506391,-67.9165709002453,
32.7793182594091));
#34503=CARTESIAN_POINT('Ctrl Pts',(-21.3650603323891,-67.419186008918,32.6681851414176));
#34504=CARTESIAN_POINT('Ctrl Pts',(-21.9326869696828,-65.6229062236153,
32.557052023426));
#34505=CARTESIAN_POINT('Ctrl Pts',(-20.7314424225063,-64.1717575047246,
32.4459189054345));
#34506=CARTESIAN_POINT('Ctrl Pts',(-18.8607529809581,-64.3938882764342,
32.3347857874429));
#34507=CARTESIAN_POINT('Ctrl Pts',(-18.0327472515632,-66.0859957134922,
32.2236526694514));
#34508=CARTESIAN_POINT('Ctrl Pts',(-19.0052486678511,-67.699396488804,32.1125195514597));
#34509=CARTESIAN_POINT('Ctrl Pts',(-20.8881856563527,-67.7574427099684,
32.0013864334682));
#34510=CARTESIAN_POINT('Ctrl Pts',(-21.9582201735135,-66.2070081906986,
31.8902533154767));
#34511=CARTESIAN_POINT('Ctrl Pts',(-21.2360145130798,-64.4671116275385,
31.7791201974851));
#34512=CARTESIAN_POINT('Ctrl Pts',(-19.3825597212183,-64.1301748367536,
31.6679870794935));
#34513=CARTESIAN_POINT('Ctrl Pts',(-18.0942105747104,-65.5045756309731,
31.556853961502));
#34514=CARTESIAN_POINT('Ctrl Pts',(-18.5501149213683,-67.3324083074391,
31.4457208435104));
#34515=CARTESIAN_POINT('Ctrl Pts',(-20.3330111589106,-67.940768457857,31.3345877255189));
#34516=CARTESIAN_POINT('Ctrl Pts',(-21.8111224766264,-66.772860927742,31.2234546075273));
#34517=CARTESIAN_POINT('Ctrl Pts',(-21.6316232186476,-64.8976006570478,
31.1123214895357));
#34518=CARTESIAN_POINT('Ctrl Pts',(-19.9587981708986,-64.0312996550389,
31.0011883715442));
#34519=CARTESIAN_POINT('Ctrl Pts',(-18.3236826588312,-64.9668306960287,
30.8900552535526));
#34520=CARTESIAN_POINT('Ctrl Pts',(-18.2227987566092,-66.8479589491607,
30.7789221355611));
#34521=CARTESIAN_POINT('Ctrl Pts',(-19.7484793822977,-67.9530017966818,
30.6677890175695));
#34522=CARTESIAN_POINT('Ctrl Pts',(-21.5043615770624,-67.2705805304779,
30.5566558995779));
#34523=CARTESIAN_POINT('Ctrl Pts',(-21.8833928454049,-65.4252739532185,
30.4455227815864));
#34524=CARTESIAN_POINT('Ctrl Pts',(-20.5386688520128,-64.1059792749701,
30.3343896635948));
#34525=CARTESIAN_POINT('Ctrl Pts',(-18.7009339234592,-64.5201669121985,
30.2232565456033));
#34526=CARTESIAN_POINT('Ctrl Pts',(-18.0521553988983,-66.2887560370454,
30.1121234276117));
#34527=CARTESIAN_POINT('Ctrl Pts',(-19.186120919682,-67.7930642714616,30.0009903096201));
#34528=CARTESIAN_POINT('Ctrl Pts',(-21.0649806087413,-67.6562895103141,
29.8898571916286));
#34529=CARTESIAN_POINT('Ctrl Pts',(-21.9691281274522,-66.0036133984072,
29.778724073637));
#34530=CARTESIAN_POINT('Ctrl Pts',(-21.071052079791,-64.347630162056,29.6675909556455));
#34531=CARTESIAN_POINT('Ctrl Pts',(-19.192707012506,-64.2039608380343,29.5564578376539));
#34532=CARTESIAN_POINT('Ctrl Pts',(-18.0532282621179,-65.704097246456,29.4453247196623));
#34533=CARTESIAN_POINT('Ctrl Pts',(-18.6955116304284,-67.4750555015402,
29.3341916016708));
#34534=CARTESIAN_POINT('Ctrl Pts',(-20.5317140987327,-67.8959849039958,
29.2230584836792));
#34535=CARTESIAN_POINT('Ctrl Pts',(-21.8812708958139,-66.581634297076,29.1119253656877));
#34536=CARTESIAN_POINT('Ctrl Pts',(-21.5090145229452,-64.7349490885693,
29.0007922476961));
#34537=CARTESIAN_POINT('Ctrl Pts',(-19.7556486644444,-64.0460882661226,
28.8896591297046));
#34538=CARTESIAN_POINT('Ctrl Pts',(-18.2259227658184,-65.145524367737,28.778526011713));
#34539=CARTESIAN_POINT('Ctrl Pts',(-18.319902178916,-67.0270101998317,28.6673928937214));
#34540=CARTESIAN_POINT('Ctrl Pts',(-19.9515732458733,-67.9685358743126,
28.5562597757299));
#34541=CARTESIAN_POINT('Ctrl Pts',(-21.6275663842701,-67.1083800358061,
28.4451266577383));
#34542=CARTESIAN_POINT('Ctrl Pts',(-21.8139467073857,-65.2337911631157,
28.3339935397468));
#34543=CARTESIAN_POINT('Ctrl Pts',(-20.3401316076723,-64.0604667756301,
28.2228604217552));
#34544=CARTESIAN_POINT('Ctrl Pts',(-18.5550146731335,-64.6622795343665,
28.1117273037637));
#34545=CARTESIAN_POINT('Ctrl Pts',(-18.0924051838791,-66.4884267154256,
28.0005941857721));
#34546=CARTESIAN_POINT('Ctrl Pts',(-19.3757015524034,-67.867546542218,27.8894610677805));
#34547=CARTESIAN_POINT('Ctrl Pts',(-21.2303804325857,-67.5374142676988,
27.778327949789));
#34548=CARTESIAN_POINT('Ctrl Pts',(-21.958966713025,-65.8001799432619,27.6671948317974));
#34549=CARTESIAN_POINT('Ctrl Pts',(-20.8946295545994,-64.2458287997599,
27.5560617138058));
#34550=CARTESIAN_POINT('Ctrl Pts',(-19.0114922133866,-64.2969641818893,
27.4449285958143));
#34551=CARTESIAN_POINT('Ctrl Pts',(-18.03307611004,-65.9067849762562,27.3337954778227));
#34552=CARTESIAN_POINT('Ctrl Pts',(-18.8548661596405,-67.6019198279331,
27.2226623598312));
#34553=CARTESIAN_POINT('Ctrl Pts',(-20.7247277889425,-67.830914604783,27.1115292418396));
#34554=CARTESIAN_POINT('Ctrl Pts',(-21.9312899869498,-66.3841842659606,
27.0003961238481));
#34555=CARTESIAN_POINT('Ctrl Pts',(-21.3702596415523,-64.5858333761097,
26.8892630058565));
#34556=CARTESIAN_POINT('Ctrl Pts',(-19.5551136047582,-64.0817834205157,
26.7781298878649));
#34557=CARTESIAN_POINT('Ctrl Pts',(-18.1471453757266,-65.3333608205724,
26.6669967698734));
#34558=CARTESIAN_POINT('Ctrl Pts',(-18.4349820915709,-67.1950725528856,
26.5558636518818));
#34559=CARTESIAN_POINT('Ctrl Pts',(-20.1551858622327,-67.9630070135229,
26.4447305338903));
#34560=CARTESIAN_POINT('Ctrl Pts',(-21.7333552972541,-66.9343198605606,
26.3335974158987));
#34561=CARTESIAN_POINT('Ctrl Pts',(-21.725093979871,-65.0505070579402,26.2224642979072));
#34562=CARTESIAN_POINT('Ctrl Pts',(-20.1379502994991,-64.0357062492462,
26.1113311799156));
#34563=CARTESIAN_POINT('Ctrl Pts',(-18.4245659304409,-64.8187070236213,
26.000198061924));
#34564=CARTESIAN_POINT('Ctrl Pts',(-18.1530472239507,-66.6828683843421,
25.8890649439325));
#34565=CARTESIAN_POINT('Ctrl Pts',(-19.5719993992621,-67.922052171765,25.7779318259409));
#34566=CARTESIAN_POINT('Ctrl Pts',(-21.3825409710216,-67.4020773255123,
25.6667987079494));
#34567=CARTESIAN_POINT('Ctrl Pts',(-21.9279930097644,-65.5989076698373,
25.5556655899578));
#34568=CARTESIAN_POINT('Ctrl Pts',(-20.7083387882887,-64.162750633872,25.4445324719662));
#34569=CARTESIAN_POINT('Ctrl Pts',(-18.8414447848292,-64.408282208203,25.3333993539747));
#34570=CARTESIAN_POINT('Ctrl Pts',(-18.032784254379,-66.1102802715637,25.2222662359831));
#34571=CARTESIAN_POINT('Ctrl Pts',(-19.0289366946352,-67.7120845933793,
25.1111331179916));
#34572=CARTESIAN_POINT('Ctrl Pts',(-20.2786416755829,-67.7334322702853,
25.0370443726639));
#34573=CARTESIAN_POINT('Ctrl Pts',(-20.7699020406705,-67.4774325188554,
25.));
#34574=CARTESIAN_POINT('Ctrl Pts',(-21.6638441630143,-65.999055839902,35.3785196366098));
#34575=CARTESIAN_POINT('Ctrl Pts',(-21.664963066366,-65.7833631633576,35.3641397488116));
#34576=CARTESIAN_POINT('Ctrl Pts',(-21.6260431435441,-65.5680576298417,
35.3497598610133));
#34577=CARTESIAN_POINT('Ctrl Pts',(-21.5452118636389,-65.369845080329,35.335379973215));
#34578=CARTESIAN_POINT('Ctrl Pts',(-21.3369804714531,-64.8592249938715,
35.2983356005512));
#34579=CARTESIAN_POINT('Ctrl Pts',(-20.8506079473568,-64.4620410318734,
35.2612912278873));
#34580=CARTESIAN_POINT('Ctrl Pts',(-20.3086785318634,-64.3600391392936,
35.2242468552234));
#34581=CARTESIAN_POINT('Ctrl Pts',(-19.76674911637,-64.2580372467139,35.1872024825596));
#34582=CARTESIAN_POINT('Ctrl Pts',(-19.1692628094796,-64.4512174235525,
35.1501581098957));
#34583=CARTESIAN_POINT('Ctrl Pts',(-18.7896357863842,-64.8511832658813,
35.1131137372319));
#34584=CARTESIAN_POINT('Ctrl Pts',(-18.4100087632888,-65.2511491082101,
35.076069364568));
#34585=CARTESIAN_POINT('Ctrl Pts',(-18.2482410239884,-65.857900616029,35.0390249919042));
#34586=CARTESIAN_POINT('Ctrl Pts',(-18.3783633363853,-66.393773024971,35.0019806192403));
#34587=CARTESIAN_POINT('Ctrl Pts',(-18.5084856487821,-66.9296454339131,
34.9649362465765));
#34588=CARTESIAN_POINT('Ctrl Pts',(-18.9304980128761,-67.3946387439782,
34.9278918739126));
#34589=CARTESIAN_POINT('Ctrl Pts',(-19.4512779281967,-67.5759645374677,
34.8908475012488));
#34590=CARTESIAN_POINT('Ctrl Pts',(-19.9720578435174,-67.7572903309572,
34.8538031285849));
#34591=CARTESIAN_POINT('Ctrl Pts',(-20.5916053100648,-67.6549486078711,
34.8167587559211));
#34592=CARTESIAN_POINT('Ctrl Pts',(-21.0264038854064,-67.3157721161938,
34.7797143832572));
#34593=CARTESIAN_POINT('Ctrl Pts',(-21.4223194546762,-67.0069273742812,
34.7459828010414));
#34594=CARTESIAN_POINT('Ctrl Pts',(-21.6650519511804,-66.5017129689095,
34.7122512188256));
#34595=CARTESIAN_POINT('Ctrl Pts',(-21.668208945928,-65.9991411290017,34.6785196366098));
#34596=CARTESIAN_POINT('Ctrl Pts',(-20.5301702171885,-67.9851743256717,
36.));
#34597=CARTESIAN_POINT('Ctrl Pts',(-20.5988349568115,-67.9597503182989,
36.));
#34598=CARTESIAN_POINT('Ctrl Pts',(-20.6657963519685,-67.9304366251968,
36.));
#34599=CARTESIAN_POINT('Ctrl Pts',(-20.7308654665295,-67.8975272739048,
36.));
#34600=CARTESIAN_POINT('Ctrl Pts',(-20.7977455609987,-67.8637020015282,
36.));
#34601=CARTESIAN_POINT('Ctrl Pts',(-20.8626273501256,-67.8260774511082,
36.));
#34602=CARTESIAN_POINT('Ctrl Pts',(-20.9252744643285,-67.7849282442006,
36.));
#34603=CARTESIAN_POINT('Ctrl Pts',(-20.978207188369,-67.7501598491764,36.));
#34604=CARTESIAN_POINT('Ctrl Pts',(-21.0295442108216,-67.712874099006,36.));
#34605=CARTESIAN_POINT('Ctrl Pts',(-21.0791202112029,-67.6732186358219,
36.));
#34606=CARTESIAN_POINT('Ctrl Pts',(-21.1011498844546,-67.6555972688324,
36.));
#34607=CARTESIAN_POINT('Ctrl Pts',(-21.122831527857,-67.6375078058363,36.));
#34608=CARTESIAN_POINT('Ctrl Pts',(-21.1441490823126,-67.6189624773662,
36.));
#34609=CARTESIAN_POINT('Ctrl Pts',(-21.155861650937,-67.6087730612763,36.));
#34610=CARTESIAN_POINT('Ctrl Pts',(-21.1674642919294,-67.5984460234341,
36.));
#34611=CARTESIAN_POINT('Ctrl Pts',(-21.1789542074706,-67.5879833507474,
36.));
#34612=CARTESIAN_POINT('Ctrl Pts',(-21.1895477678368,-67.5783368956189,
36.));
#34613=CARTESIAN_POINT('Ctrl Pts',(-21.2000469385075,-67.5685736271126,
36.));
#34614=CARTESIAN_POINT('Ctrl Pts',(-21.2104336389044,-67.558710558091,36.));
#34615=CARTESIAN_POINT('Ctrl Pts',(-21.2635184075268,-67.5083019858866,
36.));
#34616=CARTESIAN_POINT('Ctrl Pts',(-21.3137631820402,-67.4552050116029,
36.));
#34617=CARTESIAN_POINT('Ctrl Pts',(-21.3609492954881,-67.3996791016713,
36.));
#34618=CARTESIAN_POINT('Ctrl Pts',(-21.4077692547296,-67.3445840609934,
36.));
#34619=CARTESIAN_POINT('Ctrl Pts',(-21.4515783462198,-67.2870967510757,
36.));
#34620=CARTESIAN_POINT('Ctrl Pts',(-21.492118162325,-67.227446405065,36.));
#34621=CARTESIAN_POINT('Ctrl Pts',(-21.5258065913802,-67.1778772002002,
36.));
#34622=CARTESIAN_POINT('Ctrl Pts',(-21.5572367636985,-67.1268136492829,
36.));
#34623=CARTESIAN_POINT('Ctrl Pts',(-21.5862327897514,-67.0743808223096,
36.));
#34624=CARTESIAN_POINT('Ctrl Pts',(-21.5983389541644,-67.0524895320059,
36.));
#34625=CARTESIAN_POINT('Ctrl Pts',(-21.6100204872529,-67.0303595164811,
36.));
#34626=CARTESIAN_POINT('Ctrl Pts',(-21.6212631465098,-67.00799979522,36.));
#34627=CARTESIAN_POINT('Ctrl Pts',(-21.6264639667105,-66.9976562557281,
36.));
#34628=CARTESIAN_POINT('Ctrl Pts',(-21.6315708572837,-66.9872635601815,
36.));
#34629=CARTESIAN_POINT('Ctrl Pts',(-21.6365823430867,-66.9768226034342,
36.));
#34630=CARTESIAN_POINT('Ctrl Pts',(-21.6418143363506,-66.9659222402453,
36.));
#34631=CARTESIAN_POINT('Ctrl Pts',(-21.646938735,-66.9549767280432,36.));
#34632=CARTESIAN_POINT('Ctrl Pts',(-21.6519524804853,-66.9439913743558,
36.));
#34633=CARTESIAN_POINT('Ctrl Pts',(-21.6804928809327,-66.8814580059955,
36.));
#34634=CARTESIAN_POINT('Ctrl Pts',(-21.7054723099544,-66.8175915741647,
36.));
#34635=CARTESIAN_POINT('Ctrl Pts',(-21.7266673077709,-66.75259653298,36.));
#34636=CARTESIAN_POINT('Ctrl Pts',(-21.745869779544,-66.6937116274686,36.));
#34637=CARTESIAN_POINT('Ctrl Pts',(-21.7619655953208,-66.6338997397485,
36.));
#34638=CARTESIAN_POINT('Ctrl Pts',(-21.7747518800532,-66.5733080889475,
36.));
#34639=CARTESIAN_POINT('Ctrl Pts',(-21.7898843881512,-66.5015981539972,
36.));
#34640=CARTESIAN_POINT('Ctrl Pts',(-21.800381967919,-66.4287945165716,36.));
#34641=CARTESIAN_POINT('Ctrl Pts',(-21.8063197580553,-66.3553202766994,
36.));
#34642=CARTESIAN_POINT('Ctrl Pts',(-21.8076265822748,-66.3391496283656,
36.));
#34643=CARTESIAN_POINT('Ctrl Pts',(-21.8087123163694,-66.3229465792852,
36.));
#34644=CARTESIAN_POINT('Ctrl Pts',(-21.8095773920817,-66.3067158043034,
36.));
#34645=CARTESIAN_POINT('Ctrl Pts',(-21.8104727224283,-66.2899173840217,
36.));
#34646=CARTESIAN_POINT('Ctrl Pts',(-21.8111317001266,-66.273083070086,36.));
#34647=CARTESIAN_POINT('Ctrl Pts',(-21.8115542428401,-66.2562523196269,
36.));
#34648=CARTESIAN_POINT('Ctrl Pts',(-21.8132754914067,-66.1876914281915,
36.));
#34649=CARTESIAN_POINT('Ctrl Pts',(-21.8110851349638,-66.1191029658962,
36.));
#34650=CARTESIAN_POINT('Ctrl Pts',(-21.8051037575689,-66.0508252572189,
36.));
#34651=CARTESIAN_POINT('Ctrl Pts',(-21.7991236159828,-65.982561655357,36.));
#34652=CARTESIAN_POINT('Ctrl Pts',(-21.7893535661429,-65.9146076071237,
36.));
#34653=CARTESIAN_POINT('Ctrl Pts',(-21.775864512327,-65.8473162604127,36.));
#34654=CARTESIAN_POINT('Ctrl Pts',(-21.7661045201055,-65.7986276696904,
36.));
#34655=CARTESIAN_POINT('Ctrl Pts',(-21.7543964928538,-65.7502862841395,
36.));
#34656=CARTESIAN_POINT('Ctrl Pts',(-21.7407530856673,-65.7024355240451,
36.));
#34657=CARTESIAN_POINT('Ctrl Pts',(-21.730516731348,-65.6665341302011,36.));
#34658=CARTESIAN_POINT('Ctrl Pts',(-21.7191906681288,-65.6309090730154,
36.));
#34659=CARTESIAN_POINT('Ctrl Pts',(-21.7067763258098,-65.5956251017723,
36.));
#34660=CARTESIAN_POINT('Ctrl Pts',(-21.7026468040941,-65.5838881992669,
36.));
#34661=CARTESIAN_POINT('Ctrl Pts',(-21.6984000585611,-65.5721982316542,
36.));
#34662=CARTESIAN_POINT('Ctrl Pts',(-21.694036734101,-65.5605577596171,36.));
#34663=CARTESIAN_POINT('Ctrl Pts',(-21.6709127863924,-65.4988677181932,
36.));
#34664=CARTESIAN_POINT('Ctrl Pts',(-21.644516250875,-65.4385612113467,36.));
#34665=CARTESIAN_POINT('Ctrl Pts',(-21.6148971220792,-65.3799723297871,
36.));
#34666=CARTESIAN_POINT('Ctrl Pts',(-21.5940647872686,-65.3387643926717,
36.));
#34667=CARTESIAN_POINT('Ctrl Pts',(-21.5716374194864,-65.2984066732515,
36.));
#34668=CARTESIAN_POINT('Ctrl Pts',(-21.5476220123981,-65.2590267602619,
36.));
#34669=CARTESIAN_POINT('Ctrl Pts',(-21.5399089963368,-65.2463791336669,
36.));
#34670=CARTESIAN_POINT('Ctrl Pts',(-21.5320310170669,-65.2338307611699,
36.));
#34671=CARTESIAN_POINT('Ctrl Pts',(-21.5239916307924,-65.2213915044329,
36.));
#34672=CARTESIAN_POINT('Ctrl Pts',(-21.4897471128518,-65.1684053266386,
36.));
#34673=CARTESIAN_POINT('Ctrl Pts',(-21.4526468301773,-65.117502937192,36.));
#34674=CARTESIAN_POINT('Ctrl Pts',(-21.4127250200562,-65.0689995578316,
36.));
#34675=CARTESIAN_POINT('Ctrl Pts',(-21.3759382490648,-65.024305123801,36.));
#34676=CARTESIAN_POINT('Ctrl Pts',(-21.3367551102847,-64.9816476143428,
36.));
#34677=CARTESIAN_POINT('Ctrl Pts',(-21.2951809526149,-64.9413065633649,
36.));
#34678=CARTESIAN_POINT('Ctrl Pts',(-21.2873626038736,-64.9337201100773,
36.));
#34679=CARTESIAN_POINT('Ctrl Pts',(-21.2794596418601,-64.9262156834178,
36.));
#34680=CARTESIAN_POINT('Ctrl Pts',(-21.2714736587043,-64.9187939493416,
36.));
#34681=CARTESIAN_POINT('Origin',(-20.,-66.,30.));
#34682=CARTESIAN_POINT('Origin',(20.,-66.,24.));
#34683=CARTESIAN_POINT('Origin',(-20.,-66.,24.));
#34684=CARTESIAN_POINT('Origin',(-20.,66.,24.));
#34685=CARTESIAN_POINT('Origin',(20.,66.,24.));
#34686=CARTESIAN_POINT('Origin',(20.,50.,0.));
#34687=CARTESIAN_POINT('',(24.,45.,6.12323399573677E-16));
#34688=CARTESIAN_POINT('Origin',(24.,50.,0.));
#34689=CARTESIAN_POINT('',(16.,45.,6.12323399573677E-16));
#34690=CARTESIAN_POINT('',(20.,45.,6.12323399573677E-16));
#34691=CARTESIAN_POINT('Origin',(16.,50.,0.));
#34692=CARTESIAN_POINT('Origin',(20.,30.,20.));
#34693=CARTESIAN_POINT('',(24.,25.,20.));
#34694=CARTESIAN_POINT('Origin',(24.,30.,20.));
#34695=CARTESIAN_POINT('',(16.,25.,20.));
#34696=CARTESIAN_POINT('',(20.,25.,20.));
#34697=CARTESIAN_POINT('Origin',(16.,30.,20.));
#34698=CARTESIAN_POINT('Origin',(20.,30.,-20.));
#34699=CARTESIAN_POINT('',(24.,25.,-20.));
#34700=CARTESIAN_POINT('Origin',(24.,30.,-20.));
#34701=CARTESIAN_POINT('',(16.,25.,-20.));
#34702=CARTESIAN_POINT('',(20.,25.,-20.));
#34703=CARTESIAN_POINT('Origin',(16.,30.,-20.));
#34704=CARTESIAN_POINT('Origin',(20.,10.,0.));
#34705=CARTESIAN_POINT('',(24.,5.,6.12323399573677E-16));
#34706=CARTESIAN_POINT('Origin',(24.,10.,0.));
#34707=CARTESIAN_POINT('',(16.,5.,6.12323399573677E-16));
#34708=CARTESIAN_POINT('',(20.,5.,6.12323399573677E-16));
#34709=CARTESIAN_POINT('Origin',(16.,10.,0.));
#34710=CARTESIAN_POINT('Origin',(20.,-10.,20.));
#34711=CARTESIAN_POINT('',(24.,-15.,20.));
#34712=CARTESIAN_POINT('Origin',(24.,-10.,20.));
#34713=CARTESIAN_POINT('',(16.,-15.,20.));
#34714=CARTESIAN_POINT('',(20.,-15.,20.));
#34715=CARTESIAN_POINT('Origin',(16.,-10.,20.));
#34716=CARTESIAN_POINT('Origin',(20.,-10.,-20.));
#34717=CARTESIAN_POINT('',(24.,-15.,-20.));
#34718=CARTESIAN_POINT('Origin',(24.,-10.,-20.));
#34719=CARTESIAN_POINT('',(16.,-15.,-20.));
#34720=CARTESIAN_POINT('',(20.,-15.,-20.));
#34721=CARTESIAN_POINT('Origin',(16.,-10.,-20.));
#34722=CARTESIAN_POINT('Origin',(20.,-30.,0.));
#34723=CARTESIAN_POINT('',(24.,-35.,6.12323399573677E-16));
#34724=CARTESIAN_POINT('Origin',(24.,-30.,0.));
#34725=CARTESIAN_POINT('',(16.,-35.,6.12323399573677E-16));
#34726=CARTESIAN_POINT('',(20.,-35.,6.12323399573677E-16));
#34727=CARTESIAN_POINT('Origin',(16.,-30.,0.));
#34728=CARTESIAN_POINT('Origin',(20.,-50.,20.));
#34729=CARTESIAN_POINT('',(24.,-55.,20.));
#34730=CARTESIAN_POINT('Origin',(24.,-50.,20.));
#34731=CARTESIAN_POINT('',(16.,-55.,20.));
#34732=CARTESIAN_POINT('',(20.,-55.,20.));
#34733=CARTESIAN_POINT('Origin',(16.,-50.,20.));
#34734=CARTESIAN_POINT('Origin',(20.,-50.,-20.));
#34735=CARTESIAN_POINT('',(24.,-50.,-25.));
#34736=CARTESIAN_POINT('Origin',(24.,-50.,-20.));
#34737=CARTESIAN_POINT('',(20.,-50.,-25.));
#34738=CARTESIAN_POINT('',(16.,-50.,-25.));
#34739=CARTESIAN_POINT('',(20.,-50.,-25.));
#34740=CARTESIAN_POINT('Origin',(16.,-50.,-20.));
#34741=CARTESIAN_POINT('Origin',(20.,-50.,0.));
#34742=CARTESIAN_POINT('',(24.,-55.,6.12323399573677E-16));
#34743=CARTESIAN_POINT('Origin',(24.,-50.,0.));
#34744=CARTESIAN_POINT('',(16.,-55.,6.12323399573677E-16));
#34745=CARTESIAN_POINT('',(20.,-55.,6.12323399573677E-16));
#34746=CARTESIAN_POINT('Origin',(16.,-50.,0.));
#34747=CARTESIAN_POINT('Origin',(20.,-30.,-20.));
#34748=CARTESIAN_POINT('',(24.,-35.,-20.));
#34749=CARTESIAN_POINT('Origin',(24.,-30.,-20.));
#34750=CARTESIAN_POINT('',(16.,-35.,-20.));
#34751=CARTESIAN_POINT('',(20.,-35.,-20.));
#34752=CARTESIAN_POINT('Origin',(16.,-30.,-20.));
#34753=CARTESIAN_POINT('Origin',(20.,-30.,20.));
#34754=CARTESIAN_POINT('',(24.,-35.,20.));
#34755=CARTESIAN_POINT('Origin',(24.,-30.,20.));
#34756=CARTESIAN_POINT('',(16.,-35.,20.));
#34757=CARTESIAN_POINT('',(20.,-35.,20.));
#34758=CARTESIAN_POINT('Origin',(16.,-30.,20.));
#34759=CARTESIAN_POINT('Origin',(20.,-10.,0.));
#34760=CARTESIAN_POINT('',(24.,-15.,6.12323399573677E-16));
#34761=CARTESIAN_POINT('Origin',(24.,-10.,0.));
#34762=CARTESIAN_POINT('',(16.,-15.,6.12323399573677E-16));
#34763=CARTESIAN_POINT('',(20.,-15.,6.12323399573677E-16));
#34764=CARTESIAN_POINT('Origin',(16.,-10.,0.));
#34765=CARTESIAN_POINT('Origin',(20.,10.,-20.));
#34766=CARTESIAN_POINT('',(24.,5.,-20.));
#34767=CARTESIAN_POINT('Origin',(24.,10.,-20.));
#34768=CARTESIAN_POINT('',(16.,5.,-20.));
#34769=CARTESIAN_POINT('',(20.,5.,-20.));
#34770=CARTESIAN_POINT('Origin',(16.,10.,-20.));
#34771=CARTESIAN_POINT('Origin',(20.,10.,20.));
#34772=CARTESIAN_POINT('',(24.,5.,20.));
#34773=CARTESIAN_POINT('Origin',(24.,10.,20.));
#34774=CARTESIAN_POINT('',(16.,5.,20.));
#34775=CARTESIAN_POINT('',(20.,5.,20.));
#34776=CARTESIAN_POINT('Origin',(16.,10.,20.));
#34777=CARTESIAN_POINT('Origin',(20.,30.,0.));
#34778=CARTESIAN_POINT('',(24.,25.,6.12323399573677E-16));
#34779=CARTESIAN_POINT('Origin',(24.,30.,0.));
#34780=CARTESIAN_POINT('',(16.,25.,6.12323399573677E-16));
#34781=CARTESIAN_POINT('',(20.,25.,6.12323399573677E-16));
#34782=CARTESIAN_POINT('Origin',(16.,30.,0.));
#34783=CARTESIAN_POINT('Origin',(20.,50.,-20.));
#34784=CARTESIAN_POINT('',(24.,50.,-25.));
#34785=CARTESIAN_POINT('Origin',(24.,50.,-20.));
#34786=CARTESIAN_POINT('',(20.,50.,-25.));
#34787=CARTESIAN_POINT('',(16.,50.,-25.));
#34788=CARTESIAN_POINT('',(20.,50.,-25.));
#34789=CARTESIAN_POINT('Origin',(16.,50.,-20.));
#34790=CARTESIAN_POINT('Origin',(20.,50.,20.));
#34791=CARTESIAN_POINT('',(24.,45.,20.));
#34792=CARTESIAN_POINT('Origin',(24.,50.,20.));
#34793=CARTESIAN_POINT('',(16.,45.,20.));
#34794=CARTESIAN_POINT('',(20.,45.,20.));
#34795=CARTESIAN_POINT('Origin',(16.,50.,20.));
#34796=CARTESIAN_POINT('Origin',(16.,-62.,36.));
#34797=CARTESIAN_POINT('',(16.,-62.,36.));
#34798=CARTESIAN_POINT('',(-16.,-62.,36.));
#34799=CARTESIAN_POINT('',(8.,-62.,36.));
#34800=CARTESIAN_POINT('',(16.,-62.,-36.));
#34801=CARTESIAN_POINT('',(16.,-62.,36.));
#34802=CARTESIAN_POINT('',(-16.,-62.,-36.));
#34803=CARTESIAN_POINT('',(-16.,-62.,-36.));
#34804=CARTESIAN_POINT('',(-16.,-62.,36.));
#34805=CARTESIAN_POINT('Origin',(16.,62.,36.));
#34806=CARTESIAN_POINT('',(16.,62.,36.));
#34807=CARTESIAN_POINT('',(16.,31.,36.));
#34808=CARTESIAN_POINT('',(16.,62.,-36.));
#34809=CARTESIAN_POINT('',(16.,62.,36.));
#34810=CARTESIAN_POINT('',(16.,-62.,-36.));
#34811=CARTESIAN_POINT('Origin',(-16.,62.,36.));
#34812=CARTESIAN_POINT('',(-16.,62.,36.));
#34813=CARTESIAN_POINT('',(-8.,62.,36.));
#34814=CARTESIAN_POINT('',(-16.,62.,-36.));
#34815=CARTESIAN_POINT('',(-16.,62.,36.));
#34816=CARTESIAN_POINT('',(16.,62.,-36.));
#34817=CARTESIAN_POINT('Origin',(-16.,-62.,36.));
#34818=CARTESIAN_POINT('',(-16.,-31.,36.));
#34819=CARTESIAN_POINT('',(-16.,62.,-36.));
#34820=CARTESIAN_POINT('Origin',(0.,0.,-36.));
#34821=CARTESIAN_POINT('Origin',(24.,75.,-40.));
#34822=CARTESIAN_POINT('',(-29.,75.,36.));
#34823=CARTESIAN_POINT('',(-29.,75.,-40.));
#34824=CARTESIAN_POINT('',(24.,75.,36.));
#34825=CARTESIAN_POINT('',(12.,75.,36.));
#34826=CARTESIAN_POINT('',(24.,75.,-40.));
#34827=CARTESIAN_POINT('Origin',(24.,-70.,-40.));
#34828=CARTESIAN_POINT('',(24.,-75.,36.));
#34829=CARTESIAN_POINT('',(24.,-70.,36.));
#34830=CARTESIAN_POINT('',(24.,-75.,-40.));
#34831=CARTESIAN_POINT('Origin',(-24.,-75.,-40.));
#34832=CARTESIAN_POINT('',(-29.,-75.,36.));
#34833=CARTESIAN_POINT('',(-12.,-75.,36.));
#34834=CARTESIAN_POINT('',(-29.,-75.,-40.));
#34835=CARTESIAN_POINT('Origin',(-29.,70.,-40.));
#34836=CARTESIAN_POINT('',(-29.,35.,36.));
#34837=CARTESIAN_POINT('Origin',(0.,0.,36.));
#34838=CARTESIAN_POINT('',(0.,0.,0.));
#34839=CARTESIAN_POINT('Origin',(20.,-66.,39.));
#34840=CARTESIAN_POINT('',(17.5,-66.,41.));
#34841=CARTESIAN_POINT('Origin',(20.,-66.,41.));
#34842=CARTESIAN_POINT('',(17.5,-66.,37.));
#34843=CARTESIAN_POINT('',(17.5,-66.,39.));
#34844=CARTESIAN_POINT('Origin',(20.,-66.,37.));
#34845=CARTESIAN_POINT('Origin',(-20.,-66.,39.));
#34846=CARTESIAN_POINT('',(-22.5,-66.,41.));
#34847=CARTESIAN_POINT('Origin',(-20.,-66.,41.));
#34848=CARTESIAN_POINT('',(-22.5,-66.,37.));
#34849=CARTESIAN_POINT('',(-22.5,-66.,39.));
#34850=CARTESIAN_POINT('Origin',(-20.,-66.,37.));
#34851=CARTESIAN_POINT('Origin',(-20.,66.,39.));
#34852=CARTESIAN_POINT('',(-22.5,66.,41.));
#34853=CARTESIAN_POINT('Origin',(-20.,66.,41.));
#34854=CARTESIAN_POINT('',(-22.5,66.,37.));
#34855=CARTESIAN_POINT('',(-22.5,66.,39.));
#34856=CARTESIAN_POINT('Origin',(-20.,66.,37.));
#34857=CARTESIAN_POINT('Origin',(20.,66.,39.));
#34858=CARTESIAN_POINT('',(17.5,66.,41.));
#34859=CARTESIAN_POINT('Origin',(20.,66.,41.));
#34860=CARTESIAN_POINT('',(17.5,66.,37.));
#34861=CARTESIAN_POINT('',(17.5,66.,39.));
#34862=CARTESIAN_POINT('Origin',(20.,66.,37.));
#34863=CARTESIAN_POINT('Origin',(24.,70.,37.));
#34864=CARTESIAN_POINT('',(24.,70.,37.));
#34865=CARTESIAN_POINT('',(-24.,70.,37.));
#34866=CARTESIAN_POINT('',(24.,70.,37.));
#34867=CARTESIAN_POINT('',(-24.,70.,41.));
#34868=CARTESIAN_POINT('',(-24.,70.,37.));
#34869=CARTESIAN_POINT('',(24.,70.,41.));
#34870=CARTESIAN_POINT('',(24.,70.,41.));
#34871=CARTESIAN_POINT('',(24.,70.,37.));
#34872=CARTESIAN_POINT('Origin',(24.,-70.,37.));
#34873=CARTESIAN_POINT('',(24.,-70.,37.));
#34874=CARTESIAN_POINT('',(24.,-70.,37.));
#34875=CARTESIAN_POINT('',(24.,-70.,41.));
#34876=CARTESIAN_POINT('',(24.,-70.,41.));
#34877=CARTESIAN_POINT('',(24.,-70.,37.));
#34878=CARTESIAN_POINT('Origin',(-24.,-70.,37.));
#34879=CARTESIAN_POINT('',(-24.,-70.,37.));
#34880=CARTESIAN_POINT('',(-24.,-70.,37.));
#34881=CARTESIAN_POINT('',(-24.,-70.,41.));
#34882=CARTESIAN_POINT('',(-24.,-70.,41.));
#34883=CARTESIAN_POINT('',(-24.,-70.,37.));
#34884=CARTESIAN_POINT('Origin',(-24.,70.,37.));
#34885=CARTESIAN_POINT('',(-24.,70.,37.));
#34886=CARTESIAN_POINT('',(-24.,70.,41.));
#34887=CARTESIAN_POINT('Origin',(0.,0.,41.));
#34888=CARTESIAN_POINT('Origin',(0.,0.,37.));
#34889=CARTESIAN_POINT('',(0.,0.,0.));
#34890=CARTESIAN_POINT('Origin',(20.,-66.,36.5));
#34891=CARTESIAN_POINT('',(17.5,-66.,37.));
#34892=CARTESIAN_POINT('Origin',(20.,-66.,37.));
#34893=CARTESIAN_POINT('',(17.5,-66.,36.));
#34894=CARTESIAN_POINT('',(17.5,-66.,36.5));
#34895=CARTESIAN_POINT('Origin',(20.,-66.,36.));
#34896=CARTESIAN_POINT('Origin',(-20.,-66.,36.5));
#34897=CARTESIAN_POINT('',(-22.5,-66.,37.));
#34898=CARTESIAN_POINT('Origin',(-20.,-66.,37.));
#34899=CARTESIAN_POINT('',(-22.5,-66.,36.));
#34900=CARTESIAN_POINT('',(-22.5,-66.,36.5));
#34901=CARTESIAN_POINT('Origin',(-20.,-66.,36.));
#34902=CARTESIAN_POINT('Origin',(-20.,66.,36.5));
#34903=CARTESIAN_POINT('',(-22.5,66.,37.));
#34904=CARTESIAN_POINT('Origin',(-20.,66.,37.));
#34905=CARTESIAN_POINT('',(-22.5,66.,36.));
#34906=CARTESIAN_POINT('',(-22.5,66.,36.5));
#34907=CARTESIAN_POINT('Origin',(-20.,66.,36.));
#34908=CARTESIAN_POINT('Origin',(20.,66.,36.5));
#34909=CARTESIAN_POINT('',(17.5,66.,37.));
#34910=CARTESIAN_POINT('Origin',(20.,66.,37.));
#34911=CARTESIAN_POINT('',(17.5,66.,36.));
#34912=CARTESIAN_POINT('',(17.5,66.,36.5));
#34913=CARTESIAN_POINT('Origin',(20.,66.,36.));
#34914=CARTESIAN_POINT('Origin',(16.,-62.,37.));
#34915=CARTESIAN_POINT('',(16.,-62.,37.));
#34916=CARTESIAN_POINT('',(-16.,-62.,37.));
#34917=CARTESIAN_POINT('',(8.,-62.,37.));
#34918=CARTESIAN_POINT('',(16.,-62.,36.));
#34919=CARTESIAN_POINT('',(16.,-62.,37.));
#34920=CARTESIAN_POINT('',(-16.,-62.,36.));
#34921=CARTESIAN_POINT('',(8.,-62.,36.));
#34922=CARTESIAN_POINT('',(-16.,-62.,37.));
#34923=CARTESIAN_POINT('Origin',(16.,62.,37.));
#34924=CARTESIAN_POINT('',(16.,62.,37.));
#34925=CARTESIAN_POINT('',(16.,31.,37.));
#34926=CARTESIAN_POINT('',(16.,62.,36.));
#34927=CARTESIAN_POINT('',(16.,62.,37.));
#34928=CARTESIAN_POINT('',(16.,31.,36.));
#34929=CARTESIAN_POINT('Origin',(-16.,62.,37.));
#34930=CARTESIAN_POINT('',(-16.,62.,37.));
#34931=CARTESIAN_POINT('',(-8.,62.,37.));
#34932=CARTESIAN_POINT('',(-16.,62.,36.));
#34933=CARTESIAN_POINT('',(-16.,62.,37.));
#34934=CARTESIAN_POINT('',(-8.,62.,36.));
#34935=CARTESIAN_POINT('Origin',(-16.,-62.,37.));
#34936=CARTESIAN_POINT('',(-16.,-31.,37.));
#34937=CARTESIAN_POINT('',(-16.,-31.,36.));
#34938=CARTESIAN_POINT('Origin',(24.,70.,36.));
#34939=CARTESIAN_POINT('',(24.,70.,36.));
#34940=CARTESIAN_POINT('',(-24.,70.,36.));
#34941=CARTESIAN_POINT('',(24.,70.,36.));
#34942=CARTESIAN_POINT('',(-24.,70.,37.));
#34943=CARTESIAN_POINT('',(-24.,70.,36.));
#34944=CARTESIAN_POINT('',(24.,70.,37.));
#34945=CARTESIAN_POINT('',(24.,70.,37.));
#34946=CARTESIAN_POINT('',(24.,70.,36.));
#34947=CARTESIAN_POINT('Origin',(24.,-70.,36.));
#34948=CARTESIAN_POINT('',(24.,-70.,36.));
#34949=CARTESIAN_POINT('',(24.,-70.,36.));
#34950=CARTESIAN_POINT('',(24.,-70.,37.));
#34951=CARTESIAN_POINT('',(24.,-70.,37.));
#34952=CARTESIAN_POINT('',(24.,-70.,36.));
#34953=CARTESIAN_POINT('Origin',(-24.,-70.,36.));
#34954=CARTESIAN_POINT('',(-24.,-70.,36.));
#34955=CARTESIAN_POINT('',(-24.,-70.,36.));
#34956=CARTESIAN_POINT('',(-24.,-70.,37.));
#34957=CARTESIAN_POINT('',(-24.,-70.,37.));
#34958=CARTESIAN_POINT('',(-24.,-70.,36.));
#34959=CARTESIAN_POINT('Origin',(-24.,70.,36.));
#34960=CARTESIAN_POINT('',(-24.,70.,36.));
#34961=CARTESIAN_POINT('',(-24.,70.,37.));
#34962=CARTESIAN_POINT('Origin',(0.,0.,37.));
#34963=CARTESIAN_POINT('Origin',(0.,0.,36.));
#34964=CARTESIAN_POINT('',(0.,0.,0.));
#34965=CARTESIAN_POINT('Origin',(0.,0.,0.));
#34966=CARTESIAN_POINT('',(-4.,-4.89858719658941E-16,316.));
#34967=CARTESIAN_POINT('Origin',(0.,0.,316.));
#34968=CARTESIAN_POINT('',(-4.,-4.89858719658941E-16,0.));
#34969=CARTESIAN_POINT('',(-4.,-4.89858719658941E-16,0.));
#34970=CARTESIAN_POINT('Origin',(0.,0.,0.));
#34971=CARTESIAN_POINT('Origin',(0.,0.,0.));
#34972=CARTESIAN_POINT('',(-5.,-6.12323399573677E-16,316.));
#34973=CARTESIAN_POINT('Origin',(0.,0.,316.));
#34974=CARTESIAN_POINT('',(-5.,-6.12323399573677E-16,0.));
#34975=CARTESIAN_POINT('',(-5.,-6.12323399573677E-16,0.));
#34976=CARTESIAN_POINT('Origin',(0.,0.,0.));
#34977=CARTESIAN_POINT('Origin',(0.,0.,316.));
#34978=CARTESIAN_POINT('Origin',(0.,0.,0.));
#34979=CARTESIAN_POINT('',(0.,0.,0.));
#34980=CARTESIAN_POINT('Origin',(50.,0.,0.5));
#34981=CARTESIAN_POINT('',(45.,6.12323399573677E-16,1.));
#34982=CARTESIAN_POINT('Origin',(50.,0.,1.));
#34983=CARTESIAN_POINT('',(45.,6.12323399573677E-16,0.));
#34984=CARTESIAN_POINT('',(45.,6.12323399573677E-16,0.5));
#34985=CARTESIAN_POINT('Origin',(50.,0.,0.));
#34986=CARTESIAN_POINT('Origin',(30.,20.,0.5));
#34987=CARTESIAN_POINT('',(25.,20.,1.));
#34988=CARTESIAN_POINT('Origin',(30.,20.,1.));
#34989=CARTESIAN_POINT('',(25.,20.,0.));
#34990=CARTESIAN_POINT('',(25.,20.,0.5));
#34991=CARTESIAN_POINT('Origin',(30.,20.,0.));
#34992=CARTESIAN_POINT('Origin',(30.,-20.,0.5));
#34993=CARTESIAN_POINT('',(25.,-20.,1.));
#34994=CARTESIAN_POINT('Origin',(30.,-20.,1.));
#34995=CARTESIAN_POINT('',(25.,-20.,0.));
#34996=CARTESIAN_POINT('',(25.,-20.,0.5));
#34997=CARTESIAN_POINT('Origin',(30.,-20.,0.));
#34998=CARTESIAN_POINT('Origin',(10.,0.,0.5));
#34999=CARTESIAN_POINT('',(5.,6.12323399573677E-16,1.));
#35000=CARTESIAN_POINT('Origin',(10.,0.,1.));
#35001=CARTESIAN_POINT('',(5.,6.12323399573677E-16,0.));
#35002=CARTESIAN_POINT('',(5.,6.12323399573677E-16,0.5));
#35003=CARTESIAN_POINT('Origin',(10.,0.,0.));
#35004=CARTESIAN_POINT('Origin',(-10.,20.,0.5));
#35005=CARTESIAN_POINT('',(-15.,20.,1.));
#35006=CARTESIAN_POINT('Origin',(-10.,20.,1.));
#35007=CARTESIAN_POINT('',(-15.,20.,0.));
#35008=CARTESIAN_POINT('',(-15.,20.,0.5));
#35009=CARTESIAN_POINT('Origin',(-10.,20.,0.));
#35010=CARTESIAN_POINT('Origin',(-10.,-20.,0.5));
#35011=CARTESIAN_POINT('',(-15.,-20.,1.));
#35012=CARTESIAN_POINT('Origin',(-10.,-20.,1.));
#35013=CARTESIAN_POINT('',(-15.,-20.,0.));
#35014=CARTESIAN_POINT('',(-15.,-20.,0.5));
#35015=CARTESIAN_POINT('Origin',(-10.,-20.,0.));
#35016=CARTESIAN_POINT('Origin',(-30.,0.,0.5));
#35017=CARTESIAN_POINT('',(-35.,6.12323399573677E-16,1.));
#35018=CARTESIAN_POINT('Origin',(-30.,0.,1.));
#35019=CARTESIAN_POINT('',(-35.,6.12323399573677E-16,0.));
#35020=CARTESIAN_POINT('',(-35.,6.12323399573677E-16,0.5));
#35021=CARTESIAN_POINT('Origin',(-30.,0.,0.));
#35022=CARTESIAN_POINT('Origin',(-50.,20.,0.5));
#35023=CARTESIAN_POINT('',(-55.,20.,1.));
#35024=CARTESIAN_POINT('Origin',(-50.,20.,1.));
#35025=CARTESIAN_POINT('',(-55.,20.,0.));
#35026=CARTESIAN_POINT('',(-55.,20.,0.5));
#35027=CARTESIAN_POINT('Origin',(-50.,20.,0.));
#35028=CARTESIAN_POINT('Origin',(-50.,-20.,0.5));
#35029=CARTESIAN_POINT('',(-55.,-20.,1.));
#35030=CARTESIAN_POINT('Origin',(-50.,-20.,1.));
#35031=CARTESIAN_POINT('',(-55.,-20.,0.));
#35032=CARTESIAN_POINT('',(-55.,-20.,0.5));
#35033=CARTESIAN_POINT('Origin',(-50.,-20.,0.));
#35034=CARTESIAN_POINT('Origin',(-50.,0.,0.5));
#35035=CARTESIAN_POINT('',(-55.,6.12323399573677E-16,1.));
#35036=CARTESIAN_POINT('Origin',(-50.,0.,1.));
#35037=CARTESIAN_POINT('',(-55.,6.12323399573677E-16,0.));
#35038=CARTESIAN_POINT('',(-55.,6.12323399573677E-16,0.5));
#35039=CARTESIAN_POINT('Origin',(-50.,0.,0.));
#35040=CARTESIAN_POINT('Origin',(-30.,-20.,0.5));
#35041=CARTESIAN_POINT('',(-35.,-20.,1.));
#35042=CARTESIAN_POINT('Origin',(-30.,-20.,1.));
#35043=CARTESIAN_POINT('',(-35.,-20.,0.));
#35044=CARTESIAN_POINT('',(-35.,-20.,0.5));
#35045=CARTESIAN_POINT('Origin',(-30.,-20.,0.));
#35046=CARTESIAN_POINT('Origin',(-30.,20.,0.5));
#35047=CARTESIAN_POINT('',(-35.,20.,1.));
#35048=CARTESIAN_POINT('Origin',(-30.,20.,1.));
#35049=CARTESIAN_POINT('',(-35.,20.,0.));
#35050=CARTESIAN_POINT('',(-35.,20.,0.5));
#35051=CARTESIAN_POINT('Origin',(-30.,20.,0.));
#35052=CARTESIAN_POINT('Origin',(-10.,0.,0.5));
#35053=CARTESIAN_POINT('',(-15.,6.12323399573677E-16,1.));
#35054=CARTESIAN_POINT('Origin',(-10.,0.,1.));
#35055=CARTESIAN_POINT('',(-15.,6.12323399573677E-16,0.));
#35056=CARTESIAN_POINT('',(-15.,6.12323399573677E-16,0.5));
#35057=CARTESIAN_POINT('Origin',(-10.,0.,0.));
#35058=CARTESIAN_POINT('Origin',(10.,-20.,0.5));
#35059=CARTESIAN_POINT('',(5.,-20.,1.));
#35060=CARTESIAN_POINT('Origin',(10.,-20.,1.));
#35061=CARTESIAN_POINT('',(5.,-20.,0.));
#35062=CARTESIAN_POINT('',(5.,-20.,0.5));
#35063=CARTESIAN_POINT('Origin',(10.,-20.,0.));
#35064=CARTESIAN_POINT('Origin',(10.,20.,0.5));
#35065=CARTESIAN_POINT('',(5.,20.,1.));
#35066=CARTESIAN_POINT('Origin',(10.,20.,1.));
#35067=CARTESIAN_POINT('',(5.,20.,0.));
#35068=CARTESIAN_POINT('',(5.,20.,0.5));
#35069=CARTESIAN_POINT('Origin',(10.,20.,0.));
#35070=CARTESIAN_POINT('Origin',(30.,0.,0.5));
#35071=CARTESIAN_POINT('',(25.,6.12323399573677E-16,1.));
#35072=CARTESIAN_POINT('Origin',(30.,0.,1.));
#35073=CARTESIAN_POINT('',(25.,6.12323399573677E-16,0.));
#35074=CARTESIAN_POINT('',(25.,6.12323399573677E-16,0.5));
#35075=CARTESIAN_POINT('Origin',(30.,0.,0.));
#35076=CARTESIAN_POINT('Origin',(50.,-20.,0.5));
#35077=CARTESIAN_POINT('',(45.,-20.,1.));
#35078=CARTESIAN_POINT('Origin',(50.,-20.,1.));
#35079=CARTESIAN_POINT('',(45.,-20.,0.));
#35080=CARTESIAN_POINT('',(45.,-20.,0.5));
#35081=CARTESIAN_POINT('Origin',(50.,-20.,0.));
#35082=CARTESIAN_POINT('Origin',(50.,20.,0.5));
#35083=CARTESIAN_POINT('',(45.,20.,1.));
#35084=CARTESIAN_POINT('Origin',(50.,20.,1.));
#35085=CARTESIAN_POINT('',(45.,20.,0.));
#35086=CARTESIAN_POINT('',(45.,20.,0.5));
#35087=CARTESIAN_POINT('Origin',(50.,20.,0.));
#35088=CARTESIAN_POINT('Origin',(70.,40.,0.));
#35089=CARTESIAN_POINT('',(75.,40.,0.));
#35090=CARTESIAN_POINT('',(-75.,40.,0.));
#35091=CARTESIAN_POINT('',(70.,40.,0.));
#35092=CARTESIAN_POINT('',(-75.,40.,1.));
#35093=CARTESIAN_POINT('',(-75.,40.,0.));
#35094=CARTESIAN_POINT('',(75.,40.,1.));
#35095=CARTESIAN_POINT('',(70.,40.,1.));
#35096=CARTESIAN_POINT('',(75.,40.,0.));
#35097=CARTESIAN_POINT('Origin',(75.,-40.,0.));
#35098=CARTESIAN_POINT('',(75.,-45.,0.));
#35099=CARTESIAN_POINT('',(75.,-20.,0.));
#35100=CARTESIAN_POINT('',(75.,-45.,1.));
#35101=CARTESIAN_POINT('',(75.,-20.,1.));
#35102=CARTESIAN_POINT('',(75.,-45.,0.));
#35103=CARTESIAN_POINT('Origin',(-70.,-45.,0.));
#35104=CARTESIAN_POINT('',(-75.,-45.,0.));
#35105=CARTESIAN_POINT('',(-35.,-45.,0.));
#35106=CARTESIAN_POINT('',(-75.,-45.,1.));
#35107=CARTESIAN_POINT('',(-35.,-45.,1.));
#35108=CARTESIAN_POINT('',(-75.,-45.,0.));
#35109=CARTESIAN_POINT('Origin',(-75.,40.,0.));
#35110=CARTESIAN_POINT('',(-75.,20.,0.));
#35111=CARTESIAN_POINT('',(-75.,20.,1.));
#35112=CARTESIAN_POINT('Origin',(0.,0.,1.));
#35113=CARTESIAN_POINT('Origin',(0.,0.,0.));
#35114=CARTESIAN_POINT('',(0.,0.,0.));
#35115=CARTESIAN_POINT('Origin',(0.,0.,-43.));
#35116=CARTESIAN_POINT('',(-13.,1.59204083889156E-15,-40.));
#35117=CARTESIAN_POINT('Origin',(0.,0.,-40.));
#35118=CARTESIAN_POINT('',(-13.,1.59204083889156E-15,-46.));
#35119=CARTESIAN_POINT('',(-13.,1.59204083889156E-15,-43.));
#35120=CARTESIAN_POINT('Origin',(0.,0.,-46.));
#35121=CARTESIAN_POINT('Origin',(0.,-73.,-43.));
#35122=CARTESIAN_POINT('',(-4.5,-73.,-40.));
#35123=CARTESIAN_POINT('Origin',(0.,-73.,-40.));
#35124=CARTESIAN_POINT('',(-4.5,-73.,-46.));
#35125=CARTESIAN_POINT('',(-4.5,-73.,-43.));
#35126=CARTESIAN_POINT('Origin',(0.,-73.,-46.));
#35127=CARTESIAN_POINT('Origin',(0.,73.,-43.));
#35128=CARTESIAN_POINT('',(-4.5,73.,-40.));
#35129=CARTESIAN_POINT('Origin',(0.,73.,-40.));
#35130=CARTESIAN_POINT('',(-4.5,73.,-46.));
#35131=CARTESIAN_POINT('',(-4.5,73.,-43.));
#35132=CARTESIAN_POINT('Origin',(0.,73.,-46.));
#35133=CARTESIAN_POINT('Origin',(20.,-50.,-43.));
#35134=CARTESIAN_POINT('',(16.5,-50.,-40.));
#35135=CARTESIAN_POINT('Origin',(20.,-50.,-40.));
#35136=CARTESIAN_POINT('',(16.5,-50.,-46.));
#35137=CARTESIAN_POINT('',(16.5,-50.,-43.));
#35138=CARTESIAN_POINT('Origin',(20.,-50.,-46.));
#35139=CARTESIAN_POINT('Origin',(-20.,-50.,-43.));
#35140=CARTESIAN_POINT('',(-23.5,-50.,-40.));
#35141=CARTESIAN_POINT('Origin',(-20.,-50.,-40.));
#35142=CARTESIAN_POINT('',(-23.5,-50.,-46.));
#35143=CARTESIAN_POINT('',(-23.5,-50.,-43.));
#35144=CARTESIAN_POINT('Origin',(-20.,-50.,-46.));
#35145=CARTESIAN_POINT('Origin',(-20.,50.,-43.));
#35146=CARTESIAN_POINT('',(-23.5,50.,-40.));
#35147=CARTESIAN_POINT('Origin',(-20.,50.,-40.));
#35148=CARTESIAN_POINT('',(-23.5,50.,-46.));
#35149=CARTESIAN_POINT('',(-23.5,50.,-43.));
#35150=CARTESIAN_POINT('Origin',(-20.,50.,-46.));
#35151=CARTESIAN_POINT('Origin',(20.,50.,-43.));
#35152=CARTESIAN_POINT('',(16.5,50.,-40.));
#35153=CARTESIAN_POINT('Origin',(20.,50.,-40.));
#35154=CARTESIAN_POINT('',(16.5,50.,-46.));
#35155=CARTESIAN_POINT('',(16.5,50.,-43.));
#35156=CARTESIAN_POINT('Origin',(20.,50.,-46.));
#35157=CARTESIAN_POINT('Origin',(28.,80.,-46.));
#35158=CARTESIAN_POINT('',(28.,80.,-46.));
#35159=CARTESIAN_POINT('',(-28.,80.,-46.));
#35160=CARTESIAN_POINT('',(28.,80.,-46.));
#35161=CARTESIAN_POINT('',(-28.,80.,-40.));
#35162=CARTESIAN_POINT('',(-28.,80.,-46.));
#35163=CARTESIAN_POINT('',(28.,80.,-40.));
#35164=CARTESIAN_POINT('',(28.,80.,-40.));
#35165=CARTESIAN_POINT('',(28.,80.,-46.));
#35166=CARTESIAN_POINT('Origin',(28.,-80.,-46.));
#35167=CARTESIAN_POINT('',(28.,-80.,-46.));
#35168=CARTESIAN_POINT('',(28.,-80.,-46.));
#35169=CARTESIAN_POINT('',(28.,-80.,-40.));
#35170=CARTESIAN_POINT('',(28.,-80.,-40.));
#35171=CARTESIAN_POINT('',(28.,-80.,-46.));
#35172=CARTESIAN_POINT('Origin',(-28.,-80.,-46.));
#35173=CARTESIAN_POINT('',(-28.,-80.,-46.));
#35174=CARTESIAN_POINT('',(-28.,-80.,-46.));
#35175=CARTESIAN_POINT('',(-28.,-80.,-40.));
#35176=CARTESIAN_POINT('',(-28.,-80.,-40.));
#35177=CARTESIAN_POINT('',(-28.,-80.,-46.));
#35178=CARTESIAN_POINT('Origin',(-28.,80.,-46.));
#35179=CARTESIAN_POINT('',(-28.,80.,-46.));
#35180=CARTESIAN_POINT('',(-28.,80.,-40.));
#35181=CARTESIAN_POINT('Origin',(0.,0.,-40.));
#35182=CARTESIAN_POINT('Origin',(0.,0.,-46.));
#35183=CARTESIAN_POINT('',(0.,0.,0.));
#35184=CARTESIAN_POINT('Origin',(0.,0.,0.));
#35185=CARTESIAN_POINT('',(-1.95633559071744,0.0012731057411345,0.225869692124231));
#35186=CARTESIAN_POINT('',(-1.95587799559821,0.00207186393275607,0.124130307875758));
#35187=CARTESIAN_POINT('',(-1.954,-2.39295984553393E-16,0.));
#35188=CARTESIAN_POINT('',(0.861525859670522,1.75382131162755,0.));
#35189=CARTESIAN_POINT('Ctrl Pts',(-1.95633559071744,0.0012731057411345,
0.225869692124231));
#35190=CARTESIAN_POINT('Ctrl Pts',(-1.95680032440099,0.0682557629313676,
0.222037301306047));
#35191=CARTESIAN_POINT('Ctrl Pts',(-1.95365903766855,0.135191473590706,
0.218204910487863));
#35192=CARTESIAN_POINT('Ctrl Pts',(-1.94676806606145,0.201735328972743,
0.214372519669679));
#35193=CARTESIAN_POINT('Ctrl Pts',(-1.88017193281744,0.844832371344698,
0.1773353028412));
#35194=CARTESIAN_POINT('Ctrl Pts',(-1.46336311091822,1.45133095416213,0.140298086012721));
#35195=CARTESIAN_POINT('Ctrl Pts',(-0.886884671668765,1.7445317403525,0.103260869184242));
#35196=CARTESIAN_POINT('Ctrl Pts',(-0.351138290053491,2.01701592986141,
0.0688405794561611));
#35197=CARTESIAN_POINT('Ctrl Pts',(0.322511385444639,2.01891139473935,0.0344202897280807));
#35198=CARTESIAN_POINT('Ctrl Pts',(0.863567639152679,1.75641488315944,2.92734586571086E-17));
#35199=CARTESIAN_POINT('',(-0.861525859670574,1.75382131162752,1.38777878078145E-16));
#35200=CARTESIAN_POINT('Origin',(0.,0.,0.));
#35201=CARTESIAN_POINT('Ctrl Pts',(-0.861525859670571,1.75382131162752,
2.28983498828939E-15));
#35202=CARTESIAN_POINT('Ctrl Pts',(-1.44496782441851,1.46721837385109,0.0370621399437224));
#35203=CARTESIAN_POINT('Ctrl Pts',(-1.8691020329229,0.869083656944534,0.0741242798874424));
#35204=CARTESIAN_POINT('Ctrl Pts',(-1.94380023116171,0.227435527544788,
0.111186419831163));
#35205=CARTESIAN_POINT('Ctrl Pts',(-1.95249630318745,0.152737362394887,
0.115501049179361));
#35206=CARTESIAN_POINT('Ctrl Pts',(-1.95645657185248,0.0774494727773659,
0.119815678527559));
#35207=CARTESIAN_POINT('Ctrl Pts',(-1.95587799559821,0.00207186393275607,
0.124130307875758));
#35208=CARTESIAN_POINT('Origin',(0.,0.,0.));
#35209=CARTESIAN_POINT('',(-1.95128203910989,0.000979727872364722,0.92586969212423));
#35210=CARTESIAN_POINT('',(-1.95118672945361,0.000916100096969453,0.824130307875757));
#35211=CARTESIAN_POINT('',(-1.954,-2.39295984553393E-16,0.));
#35212=CARTESIAN_POINT('Ctrl Pts',(-1.95128203910989,0.000979727872364722,
0.92586969212423));
#35213=CARTESIAN_POINT('Ctrl Pts',(-1.9524730612105,0.263901717292074,0.910927268943587));
#35214=CARTESIAN_POINT('Ctrl Pts',(-1.90305141123492,0.526394079969068,
0.895984845762944));
#35215=CARTESIAN_POINT('Ctrl Pts',(-1.80089049647467,0.766440059940591,
0.881042422582301));
#35216=CARTESIAN_POINT('Ctrl Pts',(-1.54766811710363,1.36143291361156,0.844005205753822));
#35217=CARTESIAN_POINT('Ctrl Pts',(-0.970428066964404,1.81852045762203,
0.806967988925342));
#35218=CARTESIAN_POINT('Ctrl Pts',(-0.333230591869142,1.92861999489257,
0.769930772096863));
#35219=CARTESIAN_POINT('Ctrl Pts',(0.30396688322612,2.0387195321631,0.732893555268385));
#35220=CARTESIAN_POINT('Ctrl Pts',(1.00112178327742,1.8018310626937,0.695856338439906));
#35221=CARTESIAN_POINT('Ctrl Pts',(1.43930998255098,1.32629143144902,0.658819121611426));
#35222=CARTESIAN_POINT('Ctrl Pts',(1.87749818182454,0.850751800204341,0.621781904782947));
#35223=CARTESIAN_POINT('Ctrl Pts',(2.05671968032037,0.136561007184397,0.584744687954468));
#35224=CARTESIAN_POINT('Ctrl Pts',(1.89499805994521,-0.489512382298273,
0.547707471125989));
#35225=CARTESIAN_POINT('Ctrl Pts',(1.73327643957006,-1.11558577178094,0.51067025429751));
#35226=CARTESIAN_POINT('Ctrl Pts',(1.23061170032392,-1.65354175772633,0.473633037469032));
#35227=CARTESIAN_POINT('Ctrl Pts',(0.616932989107385,-1.8573955796291,0.436595820640553));
#35228=CARTESIAN_POINT('Ctrl Pts',(0.00325427789084558,-2.06124940153187,
0.399558603812074));
#35229=CARTESIAN_POINT('Ctrl Pts',(-0.721438405296094,-1.93100105939202,
0.362521386983595));
#35230=CARTESIAN_POINT('Ctrl Pts',(-1.22559302459517,-1.52602913735885,
0.325484170155115));
#35231=CARTESIAN_POINT('Ctrl Pts',(-1.67758072371516,-1.1629613001496,0.29227934414482));
#35232=CARTESIAN_POINT('Ctrl Pts',(-1.95230901779331,-0.579081973692791,
0.259074518134526));
#35233=CARTESIAN_POINT('Ctrl Pts',(-1.95633559071744,0.0012731057411345,
0.225869692124231));
#35234=CARTESIAN_POINT('Ctrl Pts',(-1.95587799559821,0.00207186393275607,
0.124130307875758));
#35235=CARTESIAN_POINT('Ctrl Pts',(-1.95148667238412,-0.570034995103637,
0.15687781847128));
#35236=CARTESIAN_POINT('Ctrl Pts',(-1.68562951923343,-1.14731024226281,
0.189625329066803));
#35237=CARTESIAN_POINT('Ctrl Pts',(-1.2444215732779,-1.51113938431406,0.222372839662326));
#35238=CARTESIAN_POINT('Ctrl Pts',(-0.745082529182101,-1.92290462488019,
0.259434979606046));
#35239=CARTESIAN_POINT('Ctrl Pts',(-0.0211422530173012,-2.0612735641195,
0.296497119549767));
#35240=CARTESIAN_POINT('Ctrl Pts',(0.595334795120667,-1.86428772433344,
0.333559259493488));
#35241=CARTESIAN_POINT('Ctrl Pts',(1.21181184325864,-1.66730188454737,0.370621399437209));
#35242=CARTESIAN_POINT('Ctrl Pts',(1.72082566336977,-1.13496126573593,0.40768353938093));
#35243=CARTESIAN_POINT('Ctrl Pts',(1.8894870924304,-0.510370283185346,0.444745679324651));
#35244=CARTESIAN_POINT('Ctrl Pts',(2.05814852149104,0.114220699365238,0.481807819268372));
#35245=CARTESIAN_POINT('Ctrl Pts',(1.88645755950116,0.831062045654966,0.518869959212093));
#35246=CARTESIAN_POINT('Ctrl Pts',(1.45292142815886,1.31145007703775,0.555932099155814));
#35247=CARTESIAN_POINT('Ctrl Pts',(1.01938529681656,1.79183810842053,0.592994239099535));
#35248=CARTESIAN_POINT('Ctrl Pts',(0.324003996121834,2.03577282489637,0.630056379043256));
#35249=CARTESIAN_POINT('Ctrl Pts',(-0.314654015224673,1.93172336479658,
0.667118518986976));
#35250=CARTESIAN_POINT('Ctrl Pts',(-0.953312026571179,1.8276739046968,0.704180658930697));
#35251=CARTESIAN_POINT('Ctrl Pts',(-1.53524674856946,1.37564026802139,0.741242798874417));
#35252=CARTESIAN_POINT('Ctrl Pts',(-1.79395555636014,0.782560471576942,
0.778304938818138));
#35253=CARTESIAN_POINT('Ctrl Pts',(-1.90058212652462,0.538123240897563,
0.793580061837345));
#35254=CARTESIAN_POINT('Ctrl Pts',(-1.95230335199157,0.269726953471863,
0.808855184856551));
#35255=CARTESIAN_POINT('Ctrl Pts',(-1.95118672945361,0.000916100096969453,
0.824130307875757));
#35256=CARTESIAN_POINT('Origin',(0.,0.,0.));
#35257=CARTESIAN_POINT('',(-1.95279554503994,-0.00168121501241181,1.62586969212423));
#35258=CARTESIAN_POINT('',(-1.95287184048439,-0.001702989282844,1.52413030787576));
#35259=CARTESIAN_POINT('',(-1.954,-2.39295984553393E-16,0.));
#35260=CARTESIAN_POINT('Ctrl Pts',(-1.95279554503994,-0.00168121501241181,
1.62586969212423));
#35261=CARTESIAN_POINT('Ctrl Pts',(-1.94903656010943,0.455834752155161,
1.59981723658113));
#35262=CARTESIAN_POINT('Ctrl Pts',(-1.78856730317397,0.91572573117829,1.57376478103802));
#35263=CARTESIAN_POINT('Ctrl Pts',(-1.49500760249196,1.26316552728133,1.54771232549492));
#35264=CARTESIAN_POINT('Ctrl Pts',(-1.07767134532899,1.75709989142681,1.51067510866644));
#35265=CARTESIAN_POINT('Ctrl Pts',(-0.39135122029848,2.02376358702057,1.47363789183796));
#35266=CARTESIAN_POINT('Ctrl Pts',(0.249990333148566,1.94116955279127,1.43660067500948));
#35267=CARTESIAN_POINT('Ctrl Pts',(0.891331886595613,1.85857551856197,1.39956345818101));
#35268=CARTESIAN_POINT('Ctrl Pts',(1.4876948684592,1.42672375450961,1.36252624135253));
#35269=CARTESIAN_POINT('Ctrl Pts',(1.76626827046517,0.843167597229759,1.32548902452405));
#35270=CARTESIAN_POINT('Ctrl Pts',(2.04484167247113,0.259611439949913,1.28845180769557));
#35271=CARTESIAN_POINT('Ctrl Pts',(2.00562549461947,-0.475649110557425,
1.25141459086709));
#35272=CARTESIAN_POINT('Ctrl Pts',(1.66655969053473,-1.02626219289756,1.21437737403861));
#35273=CARTESIAN_POINT('Ctrl Pts',(1.32749388644999,-1.57687527523771,1.17734015721013));
#35274=CARTESIAN_POINT('Ctrl Pts',(0.688578456132156,-1.94284088941065,
1.14030294038165));
#35275=CARTESIAN_POINT('Ctrl Pts',(0.0420898544956178,-1.9567474659654,
1.10326572355317));
#35276=CARTESIAN_POINT('Ctrl Pts',(-0.604398747140919,-1.97065404252014,
1.06622850672469));
#35277=CARTESIAN_POINT('Ctrl Pts',(-1.25846052009616,-1.6325015814567,1.02919128989622));
#35278=CARTESIAN_POINT('Ctrl Pts',(-1.62088905227235,-1.09697626925925,
0.992154073067737));
#35279=CARTESIAN_POINT('Ctrl Pts',(-1.83709816073764,-0.777505145902677,
0.970059279419901));
#35280=CARTESIAN_POINT('Ctrl Pts',(-1.94952091996443,-0.387793032173158,
0.947964485772066));
#35281=CARTESIAN_POINT('Ctrl Pts',(-1.95128203910989,0.000979727872364722,
0.92586969212423));
#35282=CARTESIAN_POINT('Ctrl Pts',(-1.95118672945361,0.000916100096969453,
0.824130307875757));
#35283=CARTESIAN_POINT('Ctrl Pts',(-1.94959408276249,-0.382490737583375,
0.845917324800272));
#35284=CARTESIAN_POINT('Ctrl Pts',(-1.84051065227066,-0.766740948347571,
0.867704341724787));
#35285=CARTESIAN_POINT('Ctrl Pts',(-1.62993550876047,-1.0835175828476,0.889491358649302));
#35286=CARTESIAN_POINT('Ctrl Pts',(-1.27172375978704,-1.62238988461419,
0.926553498593023));
#35287=CARTESIAN_POINT('Ctrl Pts',(-0.619817368257128,-1.96600853193387,
0.963615638536743));
#35288=CARTESIAN_POINT('Ctrl Pts',(0.0271864367452719,-1.95701720127518,
1.00067777848046));
#35289=CARTESIAN_POINT('Ctrl Pts',(0.674190241747668,-1.94802587061648,
1.03773991842418));
#35290=CARTESIAN_POINT('Ctrl Pts',(1.31629146022255,-1.5864245619794,1.07480205836791));
#35291=CARTESIAN_POINT('Ctrl Pts',(1.65939903784035,-1.03781956343241,1.11186419831163));
#35292=CARTESIAN_POINT('Ctrl Pts',(2.00250661545815,-0.489214564885407,
1.14892633825535));
#35293=CARTESIAN_POINT('Ctrl Pts',(2.04662055221888,0.246394123571516,1.18598847819907));
#35294=CARTESIAN_POINT('Ctrl Pts',(1.77153295980734,0.832073910176122,1.22305061814279));
#35295=CARTESIAN_POINT('Ctrl Pts',(1.49644536739581,1.41775369678073,1.26011275808651));
#35296=CARTESIAN_POINT('Ctrl Pts',(0.902156245812001,1.85350458153303,1.29717489803023));
#35297=CARTESIAN_POINT('Ctrl Pts',(0.260864347694114,1.93974733338565,1.33423703797395));
#35298=CARTESIAN_POINT('Ctrl Pts',(-0.380427550423769,2.02599008523827,
1.37129917791767));
#35299=CARTESIAN_POINT('Ctrl Pts',(-1.06872222507573,1.76272470419122,1.40836131786139));
#35300=CARTESIAN_POINT('Ctrl Pts',(-1.48876654315921,1.27053027794487,1.44542345780511));
#35301=CARTESIAN_POINT('Ctrl Pts',(-1.78610829781436,0.922114770268632,
1.47165907449533));
#35302=CARTESIAN_POINT('Ctrl Pts',(-1.94903067523895,0.458983666015645,
1.49789469118554));
#35303=CARTESIAN_POINT('Ctrl Pts',(-1.95287184048439,-0.001702989282844,
1.52413030787576));
#35304=CARTESIAN_POINT('Origin',(0.,0.,0.));
#35305=CARTESIAN_POINT('',(-1.9571996697324,4.08272333451705E-5,2.32586969212423));
#35306=CARTESIAN_POINT('',(-1.95720915199432,4.37834080700025E-5,2.22413030787575));
#35307=CARTESIAN_POINT('',(-1.954,-2.39295984553393E-16,0.));
#35308=CARTESIAN_POINT('Ctrl Pts',(-1.9571996697324,4.08272333451412E-5,
2.32586969212423));
#35309=CARTESIAN_POINT('Ctrl Pts',(-1.9572003426898,0.00222795607483405,
2.32574442104715));
#35310=CARTESIAN_POINT('Ctrl Pts',(-1.95719699336635,0.00441508279392128,
2.32561914997006));
#35311=CARTESIAN_POINT('Ctrl Pts',(-1.95718961556757,0.00660219592375261,
2.32549387889298));
#35312=CARTESIAN_POINT('Ctrl Pts',(-1.9550083208942,0.653236559609951,2.2884566620645));
#35313=CARTESIAN_POINT('Ctrl Pts',(-1.60068669068514,1.29868304829585,2.25141944523602));
#35314=CARTESIAN_POINT('Ctrl Pts',(-1.05631192010051,1.64767712566922,2.21438222840754));
#35315=CARTESIAN_POINT('Ctrl Pts',(-0.511937149515876,1.9966712030426,2.17734501157906));
#35316=CARTESIAN_POINT('Ctrl Pts',(0.222490761444335,2.04921286910345,2.14030779475058));
#35317=CARTESIAN_POINT('Ctrl Pts',(0.811002035332165,1.78126653559889,2.10327057792211));
#35318=CARTESIAN_POINT('Ctrl Pts',(1.39951330921999,1.51332020209433,2.06623336109363));
#35319=CARTESIAN_POINT('Ctrl Pts',(1.84210794603544,0.92488586902436,2.02919614426515));
#35320=CARTESIAN_POINT('Ctrl Pts',(1.93631757329266,0.28514740055385,1.99215892743667));
#35321=CARTESIAN_POINT('Ctrl Pts',(2.03052720054988,-0.354591067916664,
1.95512171060819));
#35322=CARTESIAN_POINT('Ctrl Pts',(1.77635181824887,-1.04563367178771,1.91808449377971));
#35323=CARTESIAN_POINT('Ctrl Pts',(1.29006594271768,-1.47185755477259,1.88104727695123));
#35324=CARTESIAN_POINT('Ctrl Pts',(0.803780067186484,-1.89808143775746,
1.84401006012275));
#35325=CARTESIAN_POINT('Ctrl Pts',(0.0853836984250916,-2.05948659985616,
1.80697284329427));
#35326=CARTESIAN_POINT('Ctrl Pts',(-0.536487147273854,-1.88223703762279,
1.76993562646579));
#35327=CARTESIAN_POINT('Ctrl Pts',(-1.1583579929728,-1.70498747538942,1.73289840963732));
#35328=CARTESIAN_POINT('Ctrl Pts',(-1.68370331560931,-1.18908318882399,
1.69586119280884));
#35329=CARTESIAN_POINT('Ctrl Pts',(-1.87219978227984,-0.570528529192665,
1.65882397598036));
#35330=CARTESIAN_POINT('Ctrl Pts',(-1.92810540551016,-0.387073187246384,
1.64783921469498));
#35331=CARTESIAN_POINT('Ctrl Pts',(-1.95438048401311,-0.194588316428208,
1.63685445340961));
#35332=CARTESIAN_POINT('Ctrl Pts',(-1.95279554503994,-0.00168121501241192,
1.62586969212423));
#35333=CARTESIAN_POINT('Ctrl Pts',(-1.95287184048439,-0.00170298928284375,
1.52413030787576));
#35334=CARTESIAN_POINT('Ctrl Pts',(-1.95445695530526,-0.191812291650776,
1.53495683112926));
#35335=CARTESIAN_POINT('Ctrl Pts',(-1.92895173588402,-0.381505322742495,
1.54578335438277));
#35336=CARTESIAN_POINT('Ctrl Pts',(-1.87462310228398,-0.562548805321496,
1.55660987763628));
#35337=CARTESIAN_POINT('Ctrl Pts',(-1.68864138181028,-1.18230999089587,
1.59367201758));
#35338=CARTESIAN_POINT('Ctrl Pts',(-1.16488397934787,-1.70070889059895,
1.63073415752372));
#35339=CARTESIAN_POINT('Ctrl Pts',(-0.543243355780667,-1.88030816136644,
1.66779629746744));
#35340=CARTESIAN_POINT('Ctrl Pts',(0.0783972677865321,-2.05990743213392,
1.70485843741116));
#35341=CARTESIAN_POINT('Ctrl Pts',(0.797921112458524,-1.90070707396579,
1.74192057735488));
#35342=CARTESIAN_POINT('Ctrl Pts',(1.28577075941843,-1.47562399010748,1.7789827172986));
#35343=CARTESIAN_POINT('Ctrl Pts',(1.77362040637834,-1.05054090624917,1.81604485724232));
#35344=CARTESIAN_POINT('Ctrl Pts',(2.02979585562615,-0.359575096700667,
1.85310699718604));
#35345=CARTESIAN_POINT('Ctrl Pts',(1.93696313672928,0.28079594435252,1.89016913712977));
#35346=CARTESIAN_POINT('Ctrl Pts',(1.84413041783241,0.921166985405712,1.92723127707349));
#35347=CARTESIAN_POINT('Ctrl Pts',(1.40228953079084,1.51094325796358,1.96429341701721));
#35348=CARTESIAN_POINT('Ctrl Pts',(0.813813216582781,1.77999452248681,2.00135555696093));
#35349=CARTESIAN_POINT('Ctrl Pts',(0.225336902374724,2.04904578701004,2.03841769690465));
#35350=CARTESIAN_POINT('Ctrl Pts',(-0.509774838999831,1.99737204349863,
2.07547983684837));
#35351=CARTESIAN_POINT('Ctrl Pts',(-1.05482489992153,1.64864094185095,2.11254197679209));
#35352=CARTESIAN_POINT('Ctrl Pts',(-1.59987496084323,1.29990984020327,2.14960411673581));
#35353=CARTESIAN_POINT('Ctrl Pts',(-1.95486334131209,0.654121380419318,
2.18666625667953));
#35354=CARTESIAN_POINT('Ctrl Pts',(-1.95719765431867,0.0070607094029605,
2.22372839662325));
#35355=CARTESIAN_POINT('Ctrl Pts',(-1.95720609227958,0.00472174601940803,
2.22386236704075));
#35356=CARTESIAN_POINT('Ctrl Pts',(-1.95720992231195,0.00238276601260064,
2.22399633745825));
#35357=CARTESIAN_POINT('Ctrl Pts',(-1.95720915199432,4.37834080701142E-5,
2.22413030787575));
#35358=CARTESIAN_POINT('Origin',(0.,0.,0.));
#35359=CARTESIAN_POINT('',(-1.95267691385146,0.00165493661177622,3.02586969212423));
#35360=CARTESIAN_POINT('',(-1.95274315056508,0.00167675988910205,2.92413030787576));
#35361=CARTESIAN_POINT('',(-1.954,-2.39295984553393E-16,0.));
#35362=CARTESIAN_POINT('Ctrl Pts',(-1.95267691385146,0.00165493661177622,
3.02586969212423));
#35363=CARTESIAN_POINT('Ctrl Pts',(-1.95426560914452,0.198992208020636,
3.01463438868469));
#35364=CARTESIAN_POINT('Ctrl Pts',(-1.92675342506316,0.395896803504792,
3.00339908524515));
#35365=CARTESIAN_POINT('Ctrl Pts',(-1.86830808103941,0.583146374609883,
2.9921637818056));
#35366=CARTESIAN_POINT('Ctrl Pts',(-1.67564280138135,1.20041523640586,2.95512656497712));
#35367=CARTESIAN_POINT('Ctrl Pts',(-1.14682887836242,1.71276357431471,2.91808934814864));
#35368=CARTESIAN_POINT('Ctrl Pts',(-0.523776367443795,1.8858136432031,2.88105213132016));
#35369=CARTESIAN_POINT('Ctrl Pts',(0.0992761434748341,2.0588637120915,2.84401491449168));
#35370=CARTESIAN_POINT('Ctrl Pts',(0.816567242293159,1.89261551195942,2.80697769766321));
#35371=CARTESIAN_POINT('Ctrl Pts',(1.29996651882171,1.46312057934516,2.76994048083473));
#35372=CARTESIAN_POINT('Ctrl Pts',(1.78336579535026,1.03362564673089,2.73290326400625));
#35373=CARTESIAN_POINT('Ctrl Pts',(2.03287324958903,0.340883981634439,2.69586604717777));
#35374=CARTESIAN_POINT('Ctrl Pts',(1.93434974962867,-0.298204336020968,
2.65882883034929));
#35375=CARTESIAN_POINT('Ctrl Pts',(1.83582624966831,-0.937292653676373,
2.62179161352081));
#35376=CARTESIAN_POINT('Ctrl Pts',(1.38927179550881,-1.52272762389073,2.58475439669233));
#35377=CARTESIAN_POINT('Ctrl Pts',(0.798966206784796,-1.78669745083631,
2.54771717986385));
#35378=CARTESIAN_POINT('Ctrl Pts',(0.208660618060775,-2.05066727778188,
2.51067996303538));
#35379=CARTESIAN_POINT('Ctrl Pts',(-0.525396105227766,-1.99317196145866,
2.4736427462069));
#35380=CARTESIAN_POINT('Ctrl Pts',(-1.0674039873032,-1.6405131839538,2.43660552937842));
#35381=CARTESIAN_POINT('Ctrl Pts',(-1.60757863467609,-1.28904720517098,
2.39969358362702));
#35382=CARTESIAN_POINT('Ctrl Pts',(-1.95700137841649,-0.644411052866131,
2.36278163787563));
#35383=CARTESIAN_POINT('Ctrl Pts',(-1.9571996697324,4.08272333451705E-5,
2.32586969212423));
#35384=CARTESIAN_POINT('Ctrl Pts',(-1.95720915199432,4.37834080700025E-5,
2.22413030787575));
#35385=CARTESIAN_POINT('Ctrl Pts',(-1.95699681840184,-0.644683222376,2.26105847740198));
#35386=CARTESIAN_POINT('Ctrl Pts',(-1.60725113883781,-1.28960760246236,
2.2979866469282));
#35387=CARTESIAN_POINT('Ctrl Pts',(-1.06669244200308,-1.64098742623895,
2.33491481645442));
#35388=CARTESIAN_POINT('Ctrl Pts',(-0.524172671136578,-1.99364200861572,
2.37197695639814));
#35389=CARTESIAN_POINT('Ctrl Pts',(0.210547116140745,-2.05061829112049,
2.40903909634186));
#35390=CARTESIAN_POINT('Ctrl Pts',(0.800949322066953,-1.78581989384044,
2.44610123628558));
#35391=CARTESIAN_POINT('Ctrl Pts',(1.39135152799316,-1.52102149656038,2.4831633762293));
#35392=CARTESIAN_POINT('Ctrl Pts',(1.83743615256826,-0.934448419495488,
2.52022551617302));
#35393=CARTESIAN_POINT('Ctrl Pts',(1.93488676008295,-0.294763859316313,
2.55728765611674));
#35394=CARTESIAN_POINT('Ctrl Pts',(2.03233736759764,0.344920700862864,2.59434979606046));
#35395=CARTESIAN_POINT('Ctrl Pts',(1.78115395805193,1.03771674415633,2.63141193600418));
#35396=CARTESIAN_POINT('Ctrl Pts',(1.29638398231036,1.46630865646616,2.6684740759479));
#35397=CARTESIAN_POINT('Ctrl Pts',(0.811614006568792,1.894900568776,2.70553621589162));
#35398=CARTESIAN_POINT('Ctrl Pts',(0.0932574646313782,2.05928835010221,
2.74259835583535));
#35399=CARTESIAN_POINT('Ctrl Pts',(-0.529662765081927,1.88417882975093,
2.77966049577907));
#35400=CARTESIAN_POINT('Ctrl Pts',(-1.15258299479523,1.70906930939964,2.81672263572279));
#35401=CARTESIAN_POINT('Ctrl Pts',(-1.68006691228442,1.19446248737086,2.85378477566651));
#35402=CARTESIAN_POINT('Ctrl Pts',(-1.87051544101399,0.576059451476712,
2.89084691561023));
#35403=CARTESIAN_POINT('Ctrl Pts',(-1.92752575844056,0.390941962730205,
2.90194137969874));
#35404=CARTESIAN_POINT('Ctrl Pts',(-1.95433466869055,0.196523398123763,
2.91303584378725));
#35405=CARTESIAN_POINT('Ctrl Pts',(-1.95274315056508,0.00167675988910205,
2.92413030787576));
#35406=CARTESIAN_POINT('Origin',(0.,0.,0.));
#35407=CARTESIAN_POINT('',(-1.95135107115213,-0.00103745302926256,3.72586969212423));
#35408=CARTESIAN_POINT('',(-1.95125983814034,-0.000967513988672578,3.62413030787576));
#35409=CARTESIAN_POINT('',(-1.954,-2.39295984553393E-16,0.));
#35410=CARTESIAN_POINT('Ctrl Pts',(-1.95135107115213,-0.00103745302926256,
3.72586969212423));
#35411=CARTESIAN_POINT('Ctrl Pts',(-1.9494564270682,0.392108141373472,3.70352435632223));
#35412=CARTESIAN_POINT('Ctrl Pts',(-1.83428685915158,0.78627490539017,3.68117902052023));
#35413=CARTESIAN_POINT('Ctrl Pts',(-1.61345116677478,1.10788542383069,3.65883368471823));
#35414=CARTESIAN_POINT('Ctrl Pts',(-1.24741775852795,1.64095230684139,3.62179646788975));
#35415=CARTESIAN_POINT('Ctrl Pts',(-0.591089924893776,1.97468687095231,
3.58475925106126));
#35416=CARTESIAN_POINT('Ctrl Pts',(0.0552900452708404,1.95641963566092,
3.54772203423278));
#35417=CARTESIAN_POINT('Ctrl Pts',(0.701670015435453,1.93815240036952,3.51068481740431));
#35418=CARTESIAN_POINT('Ctrl Pts',(1.3381021221305,1.56788336567581,3.47364760057583));
#35419=CARTESIAN_POINT('Ctrl Pts',(1.6734455320356,1.01499499073225,3.43661038374735));
#35420=CARTESIAN_POINT('Ctrl Pts',(2.0087889419407,0.462106615788698,3.39957316691887));
#35421=CARTESIAN_POINT('Ctrl Pts',(2.04304365505584,-0.273401099404705,
3.36253595009039));
#35422=CARTESIAN_POINT('Ctrl Pts',(1.76053958557416,-0.855064411333041,
3.32549873326191));
#35423=CARTESIAN_POINT('Ctrl Pts',(1.47803551609248,-1.43672772326139,3.28846151643343));
#35424=CARTESIAN_POINT('Ctrl Pts',(0.878772664013962,-1.86454663192466,
3.25142429960495));
#35425=CARTESIAN_POINT('Ctrl Pts',(0.236888497103484,-1.94281203925035,
3.21438708277648));
#35426=CARTESIAN_POINT('Ctrl Pts',(-0.404995669806982,-2.02107744657604,
3.177349865948));
#35427=CARTESIAN_POINT('Ctrl Pts',(-1.08950115154941,-1.74978935256416,
3.14031264911952));
#35428=CARTESIAN_POINT('Ctrl Pts',(-1.50349557427203,-1.25305061271667,
3.10327543229104));
#35429=CARTESIAN_POINT('Ctrl Pts',(-1.79190407667273,-0.906998424134863,
3.0774735189021));
#35430=CARTESIAN_POINT('Ctrl Pts',(-1.94902846959061,-0.451530792879088,
3.05167160551317));
#35431=CARTESIAN_POINT('Ctrl Pts',(-1.95267691385146,0.00165493661177622,
3.02586969212423));
#35432=CARTESIAN_POINT('Ctrl Pts',(-1.95274315056508,0.00167675988910205,
2.92413030787576));
#35433=CARTESIAN_POINT('Ctrl Pts',(-1.94901804708373,-0.45438081105706,
2.95009798373097));
#35434=CARTESIAN_POINT('Ctrl Pts',(-1.78970412039892,-0.912783539307832,
2.97606565958618));
#35435=CARTESIAN_POINT('Ctrl Pts',(-1.49789482266332,-1.25975537577289,
3.00203333544139));
#35436=CARTESIAN_POINT('Ctrl Pts',(-1.08141253561316,-1.75496791736879,
3.03909547538511));
#35437=CARTESIAN_POINT('Ctrl Pts',(-0.3950348215429,-2.02319375080107,3.07615761532883));
#35438=CARTESIAN_POINT('Ctrl Pts',(0.246862437687336,-1.94157962588032,
3.11321975527255));
#35439=CARTESIAN_POINT('Ctrl Pts',(0.888759696917571,-1.85996550095957,
3.15028189521628));
#35440=CARTESIAN_POINT('Ctrl Pts',(1.48617650130778,-1.4285114176858,3.18734403516));
#35441=CARTESIAN_POINT('Ctrl Pts',(1.76548299529208,-0.84483270534745,3.22440617510372));
#35442=CARTESIAN_POINT('Ctrl Pts',(2.04478948927638,-0.261153993009101,
3.26146831504744));
#35443=CARTESIAN_POINT('Ctrl Pts',(2.00598567285476,0.474749348393822,3.29853045499116));
#35444=CARTESIAN_POINT('Ctrl Pts',(1.66684453569178,1.02581762536563,3.33559259493488));
#35445=CARTESIAN_POINT('Ctrl Pts',(1.3277033985288,1.57688590233743,3.3726547348786));
#35446=CARTESIAN_POINT('Ctrl Pts',(0.688224940624468,1.94311911487812,3.40971687482232));
#35447=CARTESIAN_POINT('Ctrl Pts',(0.0413041672205065,1.95677450731496,
3.44677901476604));
#35448=CARTESIAN_POINT('Ctrl Pts',(-0.605616606183457,1.9704298997518,3.48384115470976));
#35449=CARTESIAN_POINT('Ctrl Pts',(-1.25997969508704,1.63150747208479,3.52090329465349));
#35450=CARTESIAN_POINT('Ctrl Pts',(-1.62207261036362,1.09524104808107,3.55796543459721));
#35451=CARTESIAN_POINT('Ctrl Pts',(-1.83754705311226,0.776119342016343,
3.58002039235672));
#35452=CARTESIAN_POINT('Ctrl Pts',(-1.94952253842872,0.387114015523011,
3.60207535011624));
#35453=CARTESIAN_POINT('Ctrl Pts',(-1.95125983814034,-0.000967513988672578,
3.62413030787576));
#35454=CARTESIAN_POINT('Origin',(0.,0.,0.));
#35455=CARTESIAN_POINT('',(-1.95645574651684,-0.00107576288577632,4.42586969212423));
#35456=CARTESIAN_POINT('',(-1.95628130950281,-0.00119277919923279,4.32413030787576));
#35457=CARTESIAN_POINT('',(-1.954,-2.39295984553393E-16,0.));
#35458=CARTESIAN_POINT('Ctrl Pts',(-1.95645574651684,-0.00107576288577632,
4.42586969212423));
#35459=CARTESIAN_POINT('Ctrl Pts',(-1.95258201164419,0.583617837825317,
4.39241432395977));
#35460=CARTESIAN_POINT('Ctrl Pts',(-1.67312331125722,1.17152394520949,4.35895895579531));
#35461=CARTESIAN_POINT('Ctrl Pts',(-1.21525966387556,1.53420296221226,4.32550358763085));
#35462=CARTESIAN_POINT('Ctrl Pts',(-0.70837553387317,1.93571166257503,4.28846637080237));
#35463=CARTESIAN_POINT('Ctrl Pts',(0.0171598407939347,2.06118438706562,
4.25142915397389));
#35464=CARTESIAN_POINT('Ctrl Pts',(0.629444641593513,1.8532226587955,4.21439193714541));
#35465=CARTESIAN_POINT('Ctrl Pts',(1.24172944239309,1.64526093052537,4.17735472031693));
#35466=CARTESIAN_POINT('Ctrl Pts',(1.74076366932515,1.10386474949453,4.14031750348845));
#35467=CARTESIAN_POINT('Ctrl Pts',(1.89826022128925,0.476700023258525,4.10328028665997));
#35468=CARTESIAN_POINT('Ctrl Pts',(2.05575677325334,-0.150464702977478,
4.06624306983149));
#35469=CARTESIAN_POINT('Ctrl Pts',(1.87171565024948,-0.86339797441863,4.02920585300301));
#35470=CARTESIAN_POINT('Ctrl Pts',(1.43032790007833,-1.33596290298842,3.99216863617453));
#35471=CARTESIAN_POINT('Ctrl Pts',(0.988940149907184,-1.80852783155821,
3.95513141934605));
#35472=CARTESIAN_POINT('Ctrl Pts',(0.290205772568748,-2.04072441725662,
3.91809420251758));
#35473=CARTESIAN_POINT('Ctrl Pts',(-0.346233738762281,-1.92633252011348,
3.8810569856891));
#35474=CARTESIAN_POINT('Ctrl Pts',(-0.982673250093302,-1.81194062297035,
3.84401976886062));
#35475=CARTESIAN_POINT('Ctrl Pts',(-1.55681789541692,-1.35096024298568,
3.80698255203214));
#35476=CARTESIAN_POINT('Ctrl Pts',(-1.806020726649,-0.754270452038098,3.76994533520366));
#35477=CARTESIAN_POINT('Ctrl Pts',(-1.90487422217158,-0.517576224744695,
3.75525345417718));
#35478=CARTESIAN_POINT('Ctrl Pts',(-1.9525967846073,-0.259527562563923,
3.74056157315071));
#35479=CARTESIAN_POINT('Ctrl Pts',(-1.95135107115213,-0.00103745302926256,
3.72586969212423));
#35480=CARTESIAN_POINT('Ctrl Pts',(-1.95125983814034,-0.000967513988672578,
3.62413030787576));
#35481=CARTESIAN_POINT('Ctrl Pts',(-1.95244197476311,-0.265035587897937,
3.63913749005996));
#35482=CARTESIAN_POINT('Ctrl Pts',(-1.90258326051973,-0.528675939020291,
3.65414467224416));
#35483=CARTESIAN_POINT('Ctrl Pts',(-1.799560505048,-0.769580726996389,3.66915185442837));
#35484=CARTESIAN_POINT('Ctrl Pts',(-1.54513274280624,-1.36452565772967,
3.70621399437209));
#35485=CARTESIAN_POINT('Ctrl Pts',(-0.966454476673152,-1.8208050988558,
3.74327613431581));
#35486=CARTESIAN_POINT('Ctrl Pts',(-0.328572905191125,-1.92943316874967,
3.78033827425953));
#35487=CARTESIAN_POINT('Ctrl Pts',(0.309308666290907,-2.03806123864353,
3.81740041420325));
#35488=CARTESIAN_POINT('Ctrl Pts',(1.00639354312189,-1.79903793730513,3.85446255414697));
#35489=CARTESIAN_POINT('Ctrl Pts',(1.44340173058911,-1.32184112162819,3.89152469409069));
#35490=CARTESIAN_POINT('Ctrl Pts',(1.88040991805633,-0.844644305951239,
3.92858683403441));
#35491=CARTESIAN_POINT('Ctrl Pts',(2.05734141615979,-0.129273975935752,
3.96564897397814));
#35492=CARTESIAN_POINT('Ctrl Pts',(1.89315776078089,0.496614739501458,4.00271111392186));
#35493=CARTESIAN_POINT('Ctrl Pts',(1.72897410540198,1.12250345493866,4.03977325386558));
#35494=CARTESIAN_POINT('Ctrl Pts',(1.22367529654071,1.65891055579759,4.0768353938093));
#35495=CARTESIAN_POINT('Ctrl Pts',(0.608699149567017,1.86014995417357,4.11389753375302));
#35496=CARTESIAN_POINT('Ctrl Pts',(-0.00627699740667481,2.06138935254956,
4.15095967369674));
#35497=CARTESIAN_POINT('Ctrl Pts',(-0.730930482492791,1.9274610484426,4.18802181364046));
#35498=CARTESIAN_POINT('Ctrl Pts',(-1.23335429038162,1.51970711029871,4.22508395358418));
#35499=CARTESIAN_POINT('Ctrl Pts',(-1.68092015819396,1.15647443240051,4.25809940501471));
#35500=CARTESIAN_POINT('Ctrl Pts',(-1.95213599025838,0.575947822566119,
4.29111485644523));
#35501=CARTESIAN_POINT('Ctrl Pts',(-1.95628130950281,-0.00119277919923279,
4.32413030787576));
#35502=CARTESIAN_POINT('Origin',(0.,0.,0.));
#35503=CARTESIAN_POINT('',(-1.95458266482996,0.00173443779922018,5.12586969212423));
#35504=CARTESIAN_POINT('',(-1.95491180920002,0.00168629508682236,5.02413030787576));
#35505=CARTESIAN_POINT('',(-1.954,-2.39295984553393E-16,0.));
#35506=CARTESIAN_POINT('Ctrl Pts',(-1.95458266482996,0.00173443779922018,
5.12586969212423));
#35507=CARTESIAN_POINT('Ctrl Pts',(-1.95579683437623,0.13363129532035,5.11834150842579));
#35508=CARTESIAN_POINT('Ctrl Pts',(-1.94358523444966,0.265304620125551,
5.11081332472735));
#35509=CARTESIAN_POINT('Ctrl Pts',(-1.91712292268468,0.394048828472761,
5.10328514102891));
#35510=CARTESIAN_POINT('Ctrl Pts',(-1.78693343503641,1.0274455880328,5.06624792420043));
#35511=CARTESIAN_POINT('Ctrl Pts',(-1.31181246839585,1.58994452273665,5.02921070737195));
#35512=CARTESIAN_POINT('Ctrl Pts',(-0.709107816346671,1.8242261056952,4.99217349054347));
#35513=CARTESIAN_POINT('Ctrl Pts',(-0.106403164297495,2.05850768865374,
4.95513627371499));
#35514=CARTESIAN_POINT('Ctrl Pts',(0.623885173160298,1.96457191986698,4.91809905688651));
#35515=CARTESIAN_POINT('Ctrl Pts',(1.14768109757825,1.58539044975217,4.88106184005803));
#35516=CARTESIAN_POINT('Ctrl Pts',(1.67147702199619,1.20620897963737,4.84402462322955));
#35517=CARTESIAN_POINT('Ctrl Pts',(1.9887805333743,0.541781808194522,4.80698740640107));
#35518=CARTESIAN_POINT('Ctrl Pts',(1.95443866449662,-0.103943670439598,
4.76995018957259));
#35519=CARTESIAN_POINT('Ctrl Pts',(1.92009679561895,-0.749669149073727,
4.73291297274411));
#35520=CARTESIAN_POINT('Ctrl Pts',(1.53410954648549,-1.37669293489913,4.69587575591563));
#35521=CARTESIAN_POINT('Ctrl Pts',(0.973049796091196,-1.69817810439032,
4.65883853908716));
#35522=CARTESIAN_POINT('Ctrl Pts',(0.411990045696909,-2.0196632738815,4.62180132225868));
#35523=CARTESIAN_POINT('Ctrl Pts',(-0.324142205958206,-2.03560982703848,
4.5847641054302));
#35524=CARTESIAN_POINT('Ctrl Pts',(-0.898597516275757,-1.7387228886878,
4.54772688860172));
#35525=CARTESIAN_POINT('Ctrl Pts',(-1.47305282659331,-1.44183595033712,
4.51068967177324));
#35526=CARTESIAN_POINT('Ctrl Pts',(-1.8858311955733,-0.832115520478776,
4.47365245494476));
#35527=CARTESIAN_POINT('Ctrl Pts',(-1.94810393739446,-0.188482967432129,
4.43661523811628));
#35528=CARTESIAN_POINT('Ctrl Pts',(-1.9541262996613,-0.126237620787308,
4.43303338945226));
#35529=CARTESIAN_POINT('Ctrl Pts',(-1.95687048211354,-0.0636751036633503,
4.42945154078825));
#35530=CARTESIAN_POINT('Ctrl Pts',(-1.95645574651684,-0.00107576288577632,
4.42586969212423));
#35531=CARTESIAN_POINT('Ctrl Pts',(-1.95628130950281,-0.00119277919923279,
4.32413030787576));
#35532=CARTESIAN_POINT('Ctrl Pts',(-1.95678939935296,-0.0719326340995119,
4.32817699638895));
#35533=CARTESIAN_POINT('Ctrl Pts',(-1.95328521122814,-0.14262162001596,
4.33222368490215));
#35534=CARTESIAN_POINT('Ctrl Pts',(-1.94560169264522,-0.212853377401693,
4.33627037341534));
#35535=CARTESIAN_POINT('Ctrl Pts',(-1.87523115632842,-0.856080354777335,
4.37333251335906));
#35536=CARTESIAN_POINT('Ctrl Pts',(-1.45429595300328,-1.46095473734778,
4.41039465330279));
#35537=CARTESIAN_POINT('Ctrl Pts',(-0.875593536694013,-1.75043093699665,
4.44745679324651));
#35538=CARTESIAN_POINT('Ctrl Pts',(-0.296891120384743,-2.03990713664554,
4.48451893319023));
#35539=CARTESIAN_POINT('Ctrl Pts',(0.439578508908652,-2.01398515337285,
4.52158107313395));
#35540=CARTESIAN_POINT('Ctrl Pts',(0.9964962855145,-1.68453781781564,4.55864321307767));
#35541=CARTESIAN_POINT('Ctrl Pts',(1.55341406212034,-1.35509048225843,4.59570535302139));
#35542=CARTESIAN_POINT('Ctrl Pts',(1.93077998603865,-0.72211779441669,4.63276749296511));
#35543=CARTESIAN_POINT('Ctrl Pts',(1.95575227831571,-0.0755349757277263,
4.66982963290883));
#35544=CARTESIAN_POINT('Ctrl Pts',(1.98072457059277,0.571047842961237,4.70689177285256));
#35545=CARTESIAN_POINT('Ctrl Pts',(1.6533032312286,1.23124079249743,4.74395391279628));
#35546=CARTESIAN_POINT('Ctrl Pts',(1.12345433605614,1.60266118112717,4.78101605273999));
#35547=CARTESIAN_POINT('Ctrl Pts',(0.59360544088369,1.97408156975691,4.81807819268371));
#35548=CARTESIAN_POINT('Ctrl Pts',(-0.138671010097046,2.05672939748021,
4.85514033262744));
#35549=CARTESIAN_POINT('Ctrl Pts',(-0.737976517839776,1.81275016640803,
4.89220247257116));
#35550=CARTESIAN_POINT('Ctrl Pts',(-1.33728202558251,1.56877093533586,4.92926461251488));
#35551=CARTESIAN_POINT('Ctrl Pts',(-1.80361659008724,0.998164645468222,
4.9663267524586));
#35552=CARTESIAN_POINT('Ctrl Pts',(-1.92338886510923,0.362281355122108,
5.00338889240232));
#35553=CARTESIAN_POINT('Ctrl Pts',(-1.94573194011967,0.243659678682544,
5.01030269756014));
#35554=CARTESIAN_POINT('Ctrl Pts',(-1.95601481281436,0.122766393772507,
5.01721650271795));
#35555=CARTESIAN_POINT('Ctrl Pts',(-1.95491180920002,0.00168629508682236,
5.02413030787576));
#35556=CARTESIAN_POINT('Origin',(0.,0.,0.));
#35557=CARTESIAN_POINT('',(-1.9507978584999,-3.45334863967226E-5,5.82586969212423));
#35558=CARTESIAN_POINT('',(-1.95080468396925,0.00018981806121043,5.72413030787576));
#35559=CARTESIAN_POINT('',(-1.954,-2.39295984553393E-16,0.));
#35560=CARTESIAN_POINT('Ctrl Pts',(-1.95079815420139,-3.45302974047446E-5,
5.82586969212423));
#35561=CARTESIAN_POINT('Ctrl Pts',(-1.95074640707532,0.328120037045956,
5.80723147606333));
#35562=CARTESIAN_POINT('Ctrl Pts',(-1.87237758907749,0.656297824114404,
5.78859326000243));
#35563=CARTESIAN_POINT('Ctrl Pts',(-1.715829951129,0.941574404236039,5.76995504394152));
#35564=CARTESIAN_POINT('Ctrl Pts',(-1.4047439120071,1.50846613462089,5.73291782711304));
#35565=CARTESIAN_POINT('Ctrl Pts',(-0.784943311216198,1.90594846094957,
5.69588061028457));
#35566=CARTESIAN_POINT('Ctrl Pts',(-0.139960769924853,1.95218999146749,
5.65884339345609));
#35567=CARTESIAN_POINT('Ctrl Pts',(0.505021771366483,1.99843152198542,5.62180617662761));
#35568=CARTESIAN_POINT('Ctrl Pts',(1.17518625315826,1.69343225669258,5.58476895979913));
#35569=CARTESIAN_POINT('Ctrl Pts',(1.56396070392606,1.17671648942254,5.54773174297065));
#35570=CARTESIAN_POINT('Ctrl Pts',(1.95273515469386,0.660000722152496,5.51069452614217));
#35571=CARTESIAN_POINT('Ctrl Pts',(2.06011957443768,-0.0684315470947738,
5.47365730931369));
#35572=CARTESIAN_POINT('Ctrl Pts',(1.83699012241942,-0.675353292756691,
5.43662009248521));
#35573=CARTESIAN_POINT('Ctrl Pts',(1.61386067040115,-1.28227503841861,5.39958287565673));
#35574=CARTESIAN_POINT('Ctrl Pts',(1.06021734662079,-1.76768626049519,5.36254565882826));
#35575=CARTESIAN_POINT('Ctrl Pts',(0.429328609649713,-1.90953180775813,
5.32550844199978));
#35576=CARTESIAN_POINT('Ctrl Pts',(-0.201560127321352,-2.05137735502108,
5.2884712251713));
#35577=CARTESIAN_POINT('Ctrl Pts',(-0.909694277483132,-1.84965722747041,
5.25143400834282));
#35578=CARTESIAN_POINT('Ctrl Pts',(-1.37113234823603,-1.39664987148696,
5.21439679151434));
#35579=CARTESIAN_POINT('Ctrl Pts',(-1.73877852911313,-1.03572077852157,
5.1848877583843));
#35580=CARTESIAN_POINT('Ctrl Pts',(-1.94982335358017,-0.515275892214865,
5.15537872525427));
#35581=CARTESIAN_POINT('Ctrl Pts',(-1.95458266482996,0.00173443779922018,
5.12586969212423));
#35582=CARTESIAN_POINT('Ctrl Pts',(-1.95491180920002,0.00168629508682236,
5.02413030787576));
#35583=CARTESIAN_POINT('Ctrl Pts',(-1.95010205227512,-0.526295513449078,
5.05427864266167));
#35584=CARTESIAN_POINT('Ctrl Pts',(-1.72879182329996,-1.05782955367232,
5.08442697744757));
#35585=CARTESIAN_POINT('Ctrl Pts',(-1.34689356786549,-1.42005289462677,
5.11457531223348));
#35586=CARTESIAN_POINT('Ctrl Pts',(-0.877416010060499,-1.86534356320495,
5.1516374521772));
#35587=CARTESIAN_POINT('Ctrl Pts',(-0.165250908911267,-2.05476460953673,
5.18869959212092));
#35588=CARTESIAN_POINT('Ctrl Pts',(0.463414671012952,-1.90155708549211,
5.22576173206464));
#35589=CARTESIAN_POINT('Ctrl Pts',(1.09208025093718,-1.74834956144749,5.26282387200837));
#35590=CARTESIAN_POINT('Ctrl Pts',(1.63724630963639,-1.25251346702646,5.29988601195209));
#35591=CARTESIAN_POINT('Ctrl Pts',(1.84921496651671,-0.641152489120857,
5.33694815189581));
#35592=CARTESIAN_POINT('Ctrl Pts',(2.06118362339704,-0.0297915112152539,
5.37401029183953));
#35593=CARTESIAN_POINT('Ctrl Pts',(1.93995487845847,0.697094350174917,5.41107243178325));
#35594=CARTESIAN_POINT('Ctrl Pts',(1.54105412656959,1.20657560296821,5.44813457172697));
#35595=CARTESIAN_POINT('Ctrl Pts',(1.14215337468071,1.71605685576151,5.48519671167069));
#35596=CARTESIAN_POINT('Ctrl Pts',(0.465580615841514,2.00813349995792,5.52225885161441));
#35597=CARTESIAN_POINT('Ctrl Pts',(-0.178779150223708,1.94902809680635,
5.55932099155813));
#35598=CARTESIAN_POINT('Ctrl Pts',(-0.823138916288934,1.88992269365477,
5.59638313150186));
#35599=CARTESIAN_POINT('Ctrl Pts',(-1.43528568958019,1.4796352431552,5.63344527144558));
#35600=CARTESIAN_POINT('Ctrl Pts',(-1.73484296927877,0.906086297567352,
5.6705074113893));
#35601=CARTESIAN_POINT('Ctrl Pts',(-1.87931321146693,0.629475576708828,
5.68838171021812));
#35602=CARTESIAN_POINT('Ctrl Pts',(-1.95107725773013,0.31489133949035,5.70625600904694));
#35603=CARTESIAN_POINT('Ctrl Pts',(-1.95080468396925,0.00018981806121043,
5.72413030787576));
#35604=CARTESIAN_POINT('Origin',(0.,0.,0.));
#35605=CARTESIAN_POINT('',(-1.95470932084261,-0.00171584046685047,6.52586969212424));
#35606=CARTESIAN_POINT('',(-1.95421427783755,-0.00177812761388513,6.42413030787576));
#35607=CARTESIAN_POINT('',(-1.954,-2.39295984553393E-16,0.));
#35608=CARTESIAN_POINT('Ctrl Pts',(-1.95470932084261,-0.00171584046685047,
6.52586969212424));
#35609=CARTESIAN_POINT('Ctrl Pts',(-1.94992946923152,0.519398730151351,
6.49612144370087));
#35610=CARTESIAN_POINT('Ctrl Pts',(-1.73506994162404,1.04399306729571,6.46637319527751));
#35611=CARTESIAN_POINT('Ctrl Pts',(-1.36210733975536,1.40545308526766,6.43662494685414));
#35612=CARTESIAN_POINT('Ctrl Pts',(-0.897760782010601,1.85547867567989,
6.39958773002566));
#35613=CARTESIAN_POINT('Ctrl Pts',(-0.188341937200331,2.05263315093338,
6.36255051319719));
#35614=CARTESIAN_POINT('Ctrl Pts',(0.441620008484366,1.90672665791667,6.32551329636871));
#35615=CARTESIAN_POINT('Ctrl Pts',(1.07158195416906,1.76082016489995,6.28847607954023));
#35616=CARTESIAN_POINT('Ctrl Pts',(1.62208700072817,1.27185270361303,6.25143886271175));
#35617=CARTESIAN_POINT('Ctrl Pts',(1.84130231899333,0.663506254660481,6.21440164588327));
#35618=CARTESIAN_POINT('Ctrl Pts',(2.0605176372585,0.0551598057079281,6.17736442905479));
#35619=CARTESIAN_POINT('Ctrl Pts',(1.94844322722972,-0.672565630910262,
6.14032721222632));
#35620=CARTESIAN_POINT('Ctrl Pts',(1.55634840229719,-1.18676637573315,6.10328999539784));
#35621=CARTESIAN_POINT('Ctrl Pts',(1.16425357736466,-1.70096712055603,6.06625277856936));
#35622=CARTESIAN_POINT('Ctrl Pts',(0.492138337528384,-2.00164317358361,
6.02921556174087));
#35623=CARTESIAN_POINT('Ctrl Pts',(-0.152532956197894,-1.95124792816734,
5.9921783449124));
#35624=CARTESIAN_POINT('Ctrl Pts',(-0.797204249924167,-1.90085268275106,
5.95514112808392));
#35625=CARTESIAN_POINT('Ctrl Pts',(-1.41443159754043,-1.49938613889095,
5.91810391125544));
#35626=CARTESIAN_POINT('Ctrl Pts',(-1.72185953262212,-0.930502299740384,
5.88106669442696));
#35627=CARTESIAN_POINT('Ctrl Pts',(-1.87458069522289,-0.647897528391999,
5.86266769365939));
#35628=CARTESIAN_POINT('Ctrl Pts',(-1.95084923717034,-0.323977343102287,
5.84426869289181));
#35629=CARTESIAN_POINT('Ctrl Pts',(-1.95079815420139,-3.45302974047446E-5,
5.82586969212423));
#35630=CARTESIAN_POINT('Ctrl Pts',(-1.95080468396925,0.00018981806121043,
5.72413030787576));
#35631=CARTESIAN_POINT('Ctrl Pts',(-1.95051207937167,-0.337638415069996,
5.74331814899066));
#35632=CARTESIAN_POINT('Ctrl Pts',(-1.86720620393942,-0.675601803708791,
5.76250599010555));
#35633=CARTESIAN_POINT('Ctrl Pts',(-1.70171536425399,-0.966869859783203,
5.78169383122045));
#35634=CARTESIAN_POINT('Ctrl Pts',(-1.38206269342473,-1.5294666308698,5.81875597116418));
#35635=CARTESIAN_POINT('Ctrl Pts',(-0.755789565660301,-1.91784973236686,
5.85581811110791));
#35636=CARTESIAN_POINT('Ctrl Pts',(-0.109742658556152,-1.95413127900566,
5.89288025105163));
#35637=CARTESIAN_POINT('Ctrl Pts',(0.536304248547996,-1.99041282564447,
5.92994239099535));
#35638=CARTESIAN_POINT('Ctrl Pts',(1.20212493499187,-1.674592817425,5.96700453093906));
#35639=CARTESIAN_POINT('Ctrl Pts',(1.58275908344154,-1.15132366886058,6.00406667088278));
#35640=CARTESIAN_POINT('Ctrl Pts',(1.9633932318912,-0.628054520296152,6.0411288108265));
#35641=CARTESIAN_POINT('Ctrl Pts',(2.05884084234667,0.102663768613233,6.07819095077022));
#35642=CARTESIAN_POINT('Ctrl Pts',(1.82538483877546,0.706146370849535,6.11525309071394));
#35643=CARTESIAN_POINT('Ctrl Pts',(1.59192883520425,1.30962897308584,6.15231523065767));
#35644=CARTESIAN_POINT('Ctrl Pts',(1.02956921760636,1.78587588864905,6.18937737060139));
#35645=CARTESIAN_POINT('Ctrl Pts',(0.395878889512919,1.91675569949154,6.22643951054511));
#35646=CARTESIAN_POINT('Ctrl Pts',(-0.237811438580523,2.04763551033402,
6.26350165048883));
#35647=CARTESIAN_POINT('Ctrl Pts',(-0.942832477169518,1.83314821645578,
6.30056379043255));
#35648=CARTESIAN_POINT('Ctrl Pts',(-1.39626929730598,1.37153365109863,6.33762593037627));
#35649=CARTESIAN_POINT('Ctrl Pts',(-1.7490486198241,1.01239194403086,6.3664607228761));
#35650=CARTESIAN_POINT('Ctrl Pts',(-1.94954331224527,0.503663409317413,
6.39529551537593));
#35651=CARTESIAN_POINT('Ctrl Pts',(-1.95421427783755,-0.00177812761388513,
6.42413030787576));
#35652=CARTESIAN_POINT('Origin',(0.,0.,0.));
#35653=CARTESIAN_POINT('',(-1.95636369417486,0.00113518110994186,7.22586969212423));
#35654=CARTESIAN_POINT('',(-1.95675615924934,0.000851174274233985,7.12413030787576));
#35655=CARTESIAN_POINT('',(-1.954,-2.39295984553393E-16,0.));
#35656=CARTESIAN_POINT('Ctrl Pts',(-1.95636369417486,0.00113518110994186,
7.22586969212423));
#35657=CARTESIAN_POINT('Ctrl Pts',(-1.95682546989371,0.0679235189129894,
7.22204862816689));
#35658=CARTESIAN_POINT('Ctrl Pts',(-1.95370156992351,0.134668159558925,
7.21822756420955));
#35659=CARTESIAN_POINT('Ctrl Pts',(-1.94684940168549,0.201027826582277,
7.2144065002522));
#35660=CARTESIAN_POINT('Ctrl Pts',(-1.88043197355288,0.844245894546327,
7.17736928342373));
#35661=CARTESIAN_POINT('Ctrl Pts',(-1.46373463610807,1.45129475044757,7.14033206659525));
#35662=CARTESIAN_POINT('Ctrl Pts',(-0.887378837876281,1.74447515831938,
7.10329484976677));
#35663=CARTESIAN_POINT('Ctrl Pts',(-0.31102303964449,2.03765556619118,7.06625763293829));
#35664=CARTESIAN_POINT('Ctrl Pts',(0.424991219374283,2.01696752603353,7.02922041610981));
#35665=CARTESIAN_POINT('Ctrl Pts',(0.983968473233738,1.69187494324663,6.99218319928133));
#35666=CARTESIAN_POINT('Ctrl Pts',(1.54294572709319,1.36678236045973,6.95514598245285));
#35667=CARTESIAN_POINT('Ctrl Pts',(1.92488597579333,0.737285235043576,6.91810876562437));
#35668=CARTESIAN_POINT('Ctrl Pts',(1.95506767226643,0.0913519390189264,
6.8810715487959));
#35669=CARTESIAN_POINT('Ctrl Pts',(1.98524936873952,-0.554581357005719,
6.84403433196742));
#35670=CARTESIAN_POINT('Ctrl Pts',(1.66367251298559,-1.21695082363886,6.80699711513894));
#35671=CARTESIAN_POINT('Ctrl Pts',(1.13744494695038,-1.59275037986524,6.76995989831046));
#35672=CARTESIAN_POINT('Ctrl Pts',(0.611217380915185,-1.96854993609162,
6.73292268148198));
#35673=CARTESIAN_POINT('Ctrl Pts',(-0.119660895401274,-2.05777958191125,
6.69588546465349));
#35674=CARTESIAN_POINT('Ctrl Pts',(-0.72084391141631,-1.81962051958034,
6.65884824782502));
#35675=CARTESIAN_POINT('Ctrl Pts',(-1.32202692743135,-1.58146145724943,
6.62181103099654));
#35676=CARTESIAN_POINT('Ctrl Pts',(-1.79351468314497,-1.01591368676797,
6.58477381416807));
#35677=CARTESIAN_POINT('Ctrl Pts',(-1.91962142566216,-0.381691448741754,
6.54773659733959));
#35678=CARTESIAN_POINT('Ctrl Pts',(-1.9444393828574,-0.256875756563692,
6.54044762893447));
#35679=CARTESIAN_POINT('Ctrl Pts',(-1.95588048853217,-0.129400253566584,
6.53315866052935));
#35680=CARTESIAN_POINT('Ctrl Pts',(-1.95470932084261,-0.00171584046685047,
6.52586969212424));
#35681=CARTESIAN_POINT('Ctrl Pts',(-1.95421427783755,-0.00177812761388513,
6.42413030787576));
#35682=CARTESIAN_POINT('Ctrl Pts',(-1.95554703085897,-0.145994290672205,
6.43235765531965));
#35683=CARTESIAN_POINT('Ctrl Pts',(-1.94093747105224,-0.289942854151266,
6.44058500276354));
#35684=CARTESIAN_POINT('Ctrl Pts',(-1.90937423221194,-0.430072724152966,
6.44881235020743));
#35685=CARTESIAN_POINT('Ctrl Pts',(-1.7671897452975,-1.06132269721135,6.48587449015115));
#35686=CARTESIAN_POINT('Ctrl Pts',(-1.28096816978468,-1.61508080649208,
6.52293663009487));
#35687=CARTESIAN_POINT('Ctrl Pts',(-0.67340953434779,-1.83771382585667,
6.55999877003859));
#35688=CARTESIAN_POINT('Ctrl Pts',(-0.0658508989108841,-2.06034684522128,
6.59706090998232));
#35689=CARTESIAN_POINT('Ctrl Pts',(0.663044796450101,-1.95185477466974,
6.63412304992604));
#35690=CARTESIAN_POINT('Ctrl Pts',(1.17942751209788,-1.56192933591821,6.67118518986976));
#35691=CARTESIAN_POINT('Ctrl Pts',(1.69581022774564,-1.17200389716668,6.70824732981348));
#35692=CARTESIAN_POINT('Ctrl Pts',(1.9996799636802,-0.500645090215166,6.7453094697572));
#35693=CARTESIAN_POINT('Ctrl Pts',(1.95185778931935,0.144650188277344,6.78237160970092));
#35694=CARTESIAN_POINT('Ctrl Pts',(1.90403561495849,0.789945466769872,6.81943374964464));
#35695=CARTESIAN_POINT('Ctrl Pts',(1.5045215303022,1.4091772168034,6.85649588958836));
#35696=CARTESIAN_POINT('Ctrl Pts',(0.936301652358751,1.71872386452436,6.89355802953208));
#35697=CARTESIAN_POINT('Ctrl Pts',(0.368081774415317,2.02827051224532,6.9306201694758));
#35698=CARTESIAN_POINT('Ctrl Pts',(-0.368843896815252,2.02813205765373,
6.96768230941953));
#35699=CARTESIAN_POINT('Ctrl Pts',(-0.936947418561655,1.71837191595589,
7.00474444936325));
#35700=CARTESIAN_POINT('Ctrl Pts',(-1.50505094030807,1.40861177425805,7.04180658930697));
#35701=CARTESIAN_POINT('Ctrl Pts',(-1.90433231257031,0.78922994545395,7.07886872925069));
#35702=CARTESIAN_POINT('Ctrl Pts',(-1.95191200566454,0.143916742729559,
7.11593086919441));
#35703=CARTESIAN_POINT('Ctrl Pts',(-1.95542076848464,0.0963281429343837,
7.11866401542153));
#35704=CARTESIAN_POINT('Ctrl Pts',(-1.95701686505733,0.0485985200318871,
7.12139716164864));
#35705=CARTESIAN_POINT('Ctrl Pts',(-1.95675615924934,0.000851174274233985,
7.12413030787576));
#35706=CARTESIAN_POINT('Origin',(0.,0.,0.));
#35707=CARTESIAN_POINT('',(-1.95128545551857,0.000980157954364874,7.92586969212424));
#35708=CARTESIAN_POINT('',(-1.95166123101285,0.00126544742759004,7.82413030787576));
#35709=CARTESIAN_POINT('',(-1.954,-2.39295984553393E-16,0.));
#35710=CARTESIAN_POINT('Ctrl Pts',(-1.95128545551857,0.000980157954364874,
7.92586969212424));
#35711=CARTESIAN_POINT('Ctrl Pts',(-1.95247914943593,0.263701155015296,
7.91093859580443));
#35712=CARTESIAN_POINT('Ctrl Pts',(-1.90313505751618,0.525992349613935,
7.89600749948463));
#35713=CARTESIAN_POINT('Ctrl Pts',(-1.80112460177197,0.765888339627252,
7.88107640316483));
#35714=CARTESIAN_POINT('Ctrl Pts',(-1.54808334564134,1.36096050365993,7.84403918633635));
#35715=CARTESIAN_POINT('Ctrl Pts',(-0.970981193167941,1.81823294990903,
7.80700196950786));
#35716=CARTESIAN_POINT('Ctrl Pts',(-0.333818027149729,1.92852282969788,
7.76996475267938));
#35717=CARTESIAN_POINT('Ctrl Pts',(0.303345138868501,2.03881270948674,7.73292753585091));
#35718=CARTESIAN_POINT('Ctrl Pts',(1.00056931843154,1.80212002281537,7.69589031902244));
#35719=CARTESIAN_POINT('Ctrl Pts',(1.43890387011628,1.32672168613705,7.65885310219396));
#35720=CARTESIAN_POINT('Ctrl Pts',(1.87723842180101,0.851323349458752,7.62181588536548));
#35721=CARTESIAN_POINT('Ctrl Pts',(2.05668334560742,0.13721936277351,7.58477866853699));
#35722=CARTESIAN_POINT('Ctrl Pts',(1.8951501609247,-0.488917833023672,7.54774145170851));
#35723=CARTESIAN_POINT('Ctrl Pts',(1.73361697624198,-1.11505502882086,7.51070423488003));
#35724=CARTESIAN_POINT('Ctrl Pts',(1.23110568307013,-1.65322543373001,7.47366701805156));
#35725=CARTESIAN_POINT('Ctrl Pts',(0.61749399359133,-1.85723879665063,7.43662980122308));
#35726=CARTESIAN_POINT('Ctrl Pts',(0.00388230411252383,-2.06125215957126,
7.3995925843946));
#35727=CARTESIAN_POINT('Ctrl Pts',(-0.72082978167322,-1.93110848050335,
7.36255536756612));
#35728=CARTESIAN_POINT('Ctrl Pts',(-1.22511706515588,-1.52634300095596,
7.32551815073764));
#35729=CARTESIAN_POINT('Ctrl Pts',(-1.6773779241913,-1.16333645789233,7.2923019978665));
#35730=CARTESIAN_POINT('Ctrl Pts',(-1.95234952088687,-0.579449614967985,
7.25908584499537));
#35731=CARTESIAN_POINT('Ctrl Pts',(-1.95636369417486,0.00113518110994186,
7.22586969212423));
#35732=CARTESIAN_POINT('Ctrl Pts',(-1.95675615924934,0.000851174274233985,
7.12413030787576));
#35733=CARTESIAN_POINT('Ctrl Pts',(-1.95348162971424,-0.598867317271105,
7.15845930159236));
#35734=CARTESIAN_POINT('Ctrl Pts',(-1.65727828481393,-1.20138176331325,
7.19278829530897));
#35735=CARTESIAN_POINT('Ctrl Pts',(-1.17884051406102,-1.56237241050387,
7.22711728902557));
#35736=CARTESIAN_POINT('Ctrl Pts',(-0.662311315437018,-1.95210378436822,
7.2641794289693));
#35737=CARTESIAN_POINT('Ctrl Pts',(0.0666250957372189,-2.06032195545224,
7.30124156891302));
#35738=CARTESIAN_POINT('Ctrl Pts',(0.674100031098693,-1.83746065393738,
7.33830370885674));
#35739=CARTESIAN_POINT('Ctrl Pts',(1.28157496646017,-1.61459935242253,7.37536584880046));
#35740=CARTESIAN_POINT('Ctrl Pts',(1.76758842600887,-1.0606585783088,7.41242798874417));
#35741=CARTESIAN_POINT('Ctrl Pts',(1.9095357026966,-0.429355222190436,7.44949012868789));
#35742=CARTESIAN_POINT('Ctrl Pts',(2.05148297938434,0.201948133927931,7.48655226863161));
#35743=CARTESIAN_POINT('Ctrl Pts',(1.84936407321109,0.910614072050953,7.52361440857534));
#35744=CARTESIAN_POINT('Ctrl Pts',(1.39575382755531,1.37205822017881,7.56067654851907));
#35745=CARTESIAN_POINT('Ctrl Pts',(0.942143581899539,1.83350236830666,7.59773868846279));
#35746=CARTESIAN_POINT('Ctrl Pts',(0.237041996761252,2.04772472643938,7.6348008284065));
#35747=CARTESIAN_POINT('Ctrl Pts',(-0.396599106844383,1.91660680765389,
7.67186296835022));
#35748=CARTESIAN_POINT('Ctrl Pts',(-1.03024021045003,1.78548888886839,7.70892510829394));
#35749=CARTESIAN_POINT('Ctrl Pts',(-1.59242083252301,1.30903069316467,7.74598724823766));
#35750=CARTESIAN_POINT('Ctrl Pts',(-1.82565005336597,0.705460409477194,
7.78304938818139));
#35751=CARTESIAN_POINT('Ctrl Pts',(-1.9118230851659,0.482454556858425,7.79674302807951));
#35752=CARTESIAN_POINT('Ctrl Pts',(-1.95308968355645,0.242096139413284,
7.81043666797764));
#35753=CARTESIAN_POINT('Ctrl Pts',(-1.95166123101285,0.00126544742759004,
7.82413030787576));
#35754=CARTESIAN_POINT('Origin',(0.,0.,0.));
#35755=CARTESIAN_POINT('',(-1.95279013340439,-0.00168009551267251,8.62586969212423));
#35756=CARTESIAN_POINT('',(-1.95215444869335,-0.00150235120299324,8.52413030787576));
#35757=CARTESIAN_POINT('',(-1.954,-2.39295984553393E-16,0.));
#35758=CARTESIAN_POINT('Ctrl Pts',(-1.95279013340439,-0.00168009551267251,
8.62586969212423));
#35759=CARTESIAN_POINT('Ctrl Pts',(-1.94903607268958,0.455640131522026,
8.59982856344197));
#35760=CARTESIAN_POINT('Ctrl Pts',(-1.78871895344458,0.915331173731693,
8.57378743475971));
#35761=CARTESIAN_POINT('Ctrl Pts',(-1.49539281844263,1.26270942713959,8.54774630607745));
#35762=CARTESIAN_POINT('Ctrl Pts',(-1.07820722729247,1.75677110357261,8.51070908924897));
#35763=CARTESIAN_POINT('Ctrl Pts',(-0.391968436807465,2.02364430724413,
8.47367187242049));
#35764=CARTESIAN_POINT('Ctrl Pts',(0.24939826400162,1.94124580780539,8.43663465559201));
#35765=CARTESIAN_POINT('Ctrl Pts',(0.890764964810705,1.85884730836666,8.39959743876353));
#35766=CARTESIAN_POINT('Ctrl Pts',(1.48725957594388,1.42717710581768,8.36256022193505));
#35767=CARTESIAN_POINT('Ctrl Pts',(1.76601098282085,0.843706103134459,8.32552300510657));
#35768=CARTESIAN_POINT('Ctrl Pts',(2.04476238969783,0.260235100451228,8.28848578827809));
#35769=CARTESIAN_POINT('Ctrl Pts',(2.00577059231861,-0.475036702366233,
8.25144857144961));
#35770=CARTESIAN_POINT('Ctrl Pts',(1.66687269277466,-1.02575348200379,8.21441135462113));
#35771=CARTESIAN_POINT('Ctrl Pts',(1.32797479323072,-1.57647026164133,8.17737413779266));
#35772=CARTESIAN_POINT('Ctrl Pts',(0.689170791522051,-1.94263201809897,
8.14033692096418));
#35773=CARTESIAN_POINT('Ctrl Pts',(0.0426865627857745,-1.95673519857469,
8.1032997041357));
#35774=CARTESIAN_POINT('Ctrl Pts',(-0.60379766595052,-1.97083837905041,
8.06626248730722));
#35775=CARTESIAN_POINT('Ctrl Pts',(-1.25796212171444,-1.6328829835442,8.02922527047874));
#35776=CARTESIAN_POINT('Ctrl Pts',(-1.62055416970245,-1.09746934488294,
7.99218805365026));
#35777=CARTESIAN_POINT('Ctrl Pts',(-1.83697171385623,-0.777901098892797,
7.97008193314158));
#35778=CARTESIAN_POINT('Ctrl Pts',(-1.94951814111497,-0.387989405753114,
7.94797581263291));
#35779=CARTESIAN_POINT('Ctrl Pts',(-1.95128545551857,0.000980157954364874,
7.92586969212424));
#35780=CARTESIAN_POINT('Ctrl Pts',(-1.95166123101285,0.00126544742759004,
7.82413030787576));
#35781=CARTESIAN_POINT('Ctrl Pts',(-1.94922354508138,-0.409717467160323,
7.84749880792136));
#35782=CARTESIAN_POINT('Ctrl Pts',(-1.82244856716882,-0.822075748123473,
7.87086730796695));
#35783=CARTESIAN_POINT('Ctrl Pts',(-1.58232634722073,-1.15191832939155,
7.89423580801255));
#35784=CARTESIAN_POINT('Ctrl Pts',(-1.20149560061961,-1.67504441290151,
7.93129794795627));
#35785=CARTESIAN_POINT('Ctrl Pts',(-0.535556287804454,-1.99061420825021,
7.96836008789999));
#35786=CARTESIAN_POINT('Ctrl Pts',(0.110476940437387,-1.95408990384897,
8.00542222784371));
#35787=CARTESIAN_POINT('Ctrl Pts',(0.756510168679237,-1.91756559944773,
8.04248436778743));
#35788=CARTESIAN_POINT('Ctrl Pts',(1.38263731234777,-1.52894719529654,8.07954650773116));
#35789=CARTESIAN_POINT('Ctrl Pts',(1.70207855773424,-0.966230350379699,
8.11660864767487));
#35790=CARTESIAN_POINT('Ctrl Pts',(2.02151980312072,-0.403513505462853,
8.1536707876186));
#35791=CARTESIAN_POINT('Ctrl Pts',(2.03427515022513,0.333301780219651,8.19073292756232));
#35792=CARTESIAN_POINT('Ctrl Pts',(1.73450237337761,0.906738122863988,8.22779506750604));
#35793=CARTESIAN_POINT('Ctrl Pts',(1.43472959653009,1.48017446550833,8.26485720744976));
#35794=CARTESIAN_POINT('Ctrl Pts',(0.822428695730641,1.89023186511451,8.30191934739348));
#35795=CARTESIAN_POINT('Ctrl Pts',(0.178046765554912,1.94909513773745,8.3389814873372));
#35796=CARTESIAN_POINT('Ctrl Pts',(-0.466335164620799,2.00795841036038,
8.37604362728092));
#35797=CARTESIAN_POINT('Ctrl Pts',(-1.14279812417278,1.71562755600011,8.41310576722464));
#35798=CARTESIAN_POINT('Ctrl Pts',(-1.54150740386038,1.20599644714809,8.45016790716836));
#35799=CARTESIAN_POINT('Ctrl Pts',(-1.80673309918174,0.866984359672774,
8.47482204073749));
#35800=CARTESIAN_POINT('Ctrl Pts',(-1.94905131081074,0.431815751432988,
8.49947617430663));
#35801=CARTESIAN_POINT('Ctrl Pts',(-1.95215444869335,-0.00150235120299324,
8.52413030787576));
#35802=CARTESIAN_POINT('Origin',(0.,0.,0.));
#35803=CARTESIAN_POINT('',(-1.95719986784682,3.71606954582295E-5,9.32586969212424));
#35804=CARTESIAN_POINT('',(-1.95707453392556,-0.000466568259871601,9.22413030787576));
#35805=CARTESIAN_POINT('',(-1.954,-2.39295984553393E-16,0.));
#35806=CARTESIAN_POINT('Ctrl Pts',(-1.95719986784682,3.71606954581456E-5,
9.32586969212423));
#35807=CARTESIAN_POINT('Ctrl Pts',(-1.95720042510874,0.00202653151786848,
9.32575574790799));
#35808=CARTESIAN_POINT('Ctrl Pts',(-1.95719765412071,0.00401590074103218,
9.32564180369175));
#35809=CARTESIAN_POINT('Ctrl Pts',(-1.95719155021855,0.00600525973720184,
9.32552785947551));
#35810=CARTESIAN_POINT('Ctrl Pts',(-1.95520749560565,0.65264027922361,9.28849064264703));
#35811=CARTESIAN_POINT('Ctrl Pts',(-1.60108272580438,1.29819476052309,9.25145342581855));
#35812=CARTESIAN_POINT('Ctrl Pts',(-1.0568144211536,1.64735485073218,9.21441620899007));
#35813=CARTESIAN_POINT('Ctrl Pts',(-0.512546116502833,1.99651494094127,
9.17737899216159));
#35814=CARTESIAN_POINT('Ctrl Pts',(0.221865722997436,2.04928064005996,9.14034177533311));
#35815=CARTESIAN_POINT('Ctrl Pts',(0.810458692323854,1.78151382429043,9.10330455850463));
#35816=CARTESIAN_POINT('Ctrl Pts',(1.39905166165026,1.51374700852089,9.06626734167615));
#35817=CARTESIAN_POINT('Ctrl Pts',(1.84182576080283,0.925447677863139,9.02923012484767));
#35818=CARTESIAN_POINT('Ctrl Pts',(1.93623051178265,0.285737974246437,8.99219290801919));
#35819=CARTESIAN_POINT('Ctrl Pts',(2.03063526276248,-0.353971729370283,
8.95515569119071));
#35820=CARTESIAN_POINT('Ctrl Pts',(1.77667066556955,-1.04509180594595,8.91811847436223));
#35821=CARTESIAN_POINT('Ctrl Pts',(1.29051481285208,-1.47146399547075,8.88108125753376));
#35822=CARTESIAN_POINT('Ctrl Pts',(0.804358960134614,-1.89783618499555,
8.84404404070528));
#35823=CARTESIAN_POINT('Ctrl Pts',(0.0860118518926114,-2.05946048746948,
8.8070068238768));
#35824=CARTESIAN_POINT('Ctrl Pts',(-0.535913025040727,-1.88240059832962,
8.76996960704832));
#35825=CARTESIAN_POINT('Ctrl Pts',(-1.15783790197406,-1.70534070918976,
8.73293239021984));
#35826=CARTESIAN_POINT('Ctrl Pts',(-1.68334054759872,-1.18959662843613,
8.69589517339136));
#35827=CARTESIAN_POINT('Ctrl Pts',(-1.87202567450341,-0.571099513462055,
8.65885795656288));
#35828=CARTESIAN_POINT('Ctrl Pts',(-1.92804495632289,-0.387472087407564,
8.64786186841667));
#35829=CARTESIAN_POINT('Ctrl Pts',(-1.95437531748109,-0.194787452297348,
8.63686578027045));
#35830=CARTESIAN_POINT('Ctrl Pts',(-1.95279013340439,-0.00168009551267234,
8.62586969212424));
#35831=CARTESIAN_POINT('Ctrl Pts',(-1.95215444869335,-0.00150235120299324,
8.52413030787576));
#35832=CARTESIAN_POINT('Ctrl Pts',(-1.95371620524508,-0.21958398707372,
8.53653831425035));
#35833=CARTESIAN_POINT('Ctrl Pts',(-1.92001564940553,-0.437196901383431,
8.54894632062494));
#35834=CARTESIAN_POINT('Ctrl Pts',(-1.84897391479539,-0.641847309864828,
8.56135432699953));
#35835=CARTESIAN_POINT('Ctrl Pts',(-1.63677554621959,-1.25312859468192,
8.59841646694325));
#35836=CARTESIAN_POINT('Ctrl Pts',(-1.0914232092448,-1.74875980097234,8.63547860688697));
#35837=CARTESIAN_POINT('Ctrl Pts',(-0.462700104058479,-1.90173108515756,
8.67254074683069));
#35838=CARTESIAN_POINT('Ctrl Pts',(0.166023001127845,-2.05470236934278,
8.70960288677441));
#35839=CARTESIAN_POINT('Ctrl Pts',(0.878116874525705,-1.86501373142281,
8.74666502671813));
#35840=CARTESIAN_POINT('Ctrl Pts',(1.34742707561642,-1.41954668207959,8.78372716666185));
#35841=CARTESIAN_POINT('Ctrl Pts',(1.81673727670714,-0.974079632736377,
8.82078930660557));
#35842=CARTESIAN_POINT('Ctrl Pts',(2.04326380549072,-0.272834171969915,
8.85785144654929));
#35843=CARTESIAN_POINT('Ctrl Pts',(1.92325259761237,0.363004067433246,8.89491358649301));
#35844=CARTESIAN_POINT('Ctrl Pts',(1.80324138973402,0.998842306836407,8.93197572643673));
#35845=CARTESIAN_POINT('Ctrl Pts',(1.33669244519374,1.56927332487627,8.96903786638045));
#35846=CARTESIAN_POINT('Ctrl Pts',(0.737295301650971,1.81302734225987,9.00610000632417));
#35847=CARTESIAN_POINT('Ctrl Pts',(0.137898158108199,2.05678135964346,9.0431621462679));
#35848=CARTESIAN_POINT('Ctrl Pts',(-0.59434718443707,1.9738583763708,9.08022428621162));
#35849=CARTESIAN_POINT('Ctrl Pts',(-1.12405647662483,1.60223891616111,9.11728642615534));
#35850=CARTESIAN_POINT('Ctrl Pts',(-1.63307724594775,1.24513356361944,9.15290105339548));
#35851=CARTESIAN_POINT('Ctrl Pts',(-1.95507366281261,0.621442230158499,
9.18851568063562));
#35852=CARTESIAN_POINT('Ctrl Pts',(-1.95707453392556,-0.000466568259871601,
9.22413030787576));
#35853=CARTESIAN_POINT('Origin',(0.,0.,0.));
#35854=CARTESIAN_POINT('',(-1.95268202714777,0.00165579016441021,10.0258696921242));
#35855=CARTESIAN_POINT('',(-1.9535343393295,0.00178280253715055,9.92413030787576));
#35856=CARTESIAN_POINT('',(-1.954,-2.39295984553393E-16,0.));
#35857=CARTESIAN_POINT('Ctrl Pts',(-1.95268202714777,0.00165579016441021,
10.0258696921242));
#35858=CARTESIAN_POINT('Ctrl Pts',(-1.9542709496717,0.198793394721131,10.0146457155455));
#35859=CARTESIAN_POINT('Ctrl Pts',(-1.92681564478375,0.395498739780043,
10.0034217389668));
#35860=CARTESIAN_POINT('Ctrl Pts',(-1.86848643290836,0.582577638715851,
9.99219776238813));
#35861=CARTESIAN_POINT('Ctrl Pts',(-1.67600993827966,1.1999062383733,9.95516054555966));
#35862=CARTESIAN_POINT('Ctrl Pts',(-1.14735119634562,1.71241362792136,9.91812332873117));
#35863=CARTESIAN_POINT('Ctrl Pts',(-0.524351231736321,1.8856531990772,9.88108611190269));
#35864=CARTESIAN_POINT('Ctrl Pts',(0.0986487328729629,2.05889277023303,
9.84404889507421));
#35865=CARTESIAN_POINT('Ctrl Pts',(0.815989920157508,1.89286452299667,9.80701167824573));
#35866=CARTESIAN_POINT('Ctrl Pts',(1.29952003507049,1.46351732792493,9.76997446141725));
#35867=CARTESIAN_POINT('Ctrl Pts',(1.78305014998348,1.03417013285319,9.73293724458878));
#35868=CARTESIAN_POINT('Ctrl Pts',(2.0327691925249,0.341503989946047,9.69590002776029));
#35869=CARTESIAN_POINT('Ctrl Pts',(1.9344406978275,-0.297614493697593,9.65886281093182));
#35870=CARTESIAN_POINT('Ctrl Pts',(1.8361122031301,-0.936732977341234,9.62182559410334));
#35871=CARTESIAN_POINT('Ctrl Pts',(1.38973617119388,-1.52230380172138,9.58478837727486));
#35872=CARTESIAN_POINT('Ctrl Pts',(0.799511084736072,-1.78645358874384,
9.54775116044638));
#35873=CARTESIAN_POINT('Ctrl Pts',(0.209285998278261,-2.0506033757663,9.5107139436179));
#35874=CARTESIAN_POINT('Ctrl Pts',(-0.524788142701144,-1.99333212543108,
9.47367672678942));
#35875=CARTESIAN_POINT('Ctrl Pts',(-1.06690354347858,-1.6408387214268,9.43663950996094));
#35876=CARTESIAN_POINT('Ctrl Pts',(-1.60735113766186,-1.28942975594381,
9.3997162373487));
#35877=CARTESIAN_POINT('Ctrl Pts',(-1.95701928883641,-0.644612332051665,
9.36279296473647));
#35878=CARTESIAN_POINT('Ctrl Pts',(-1.95719986784682,3.71606954582295E-5,
9.32586969212424));
#35879=CARTESIAN_POINT('Ctrl Pts',(-1.95707453392556,-0.000466568259871601,
9.22413030787576));
#35880=CARTESIAN_POINT('Ctrl Pts',(-1.95715585687005,-0.0257432861687418,
9.22557782057934));
#35881=CARTESIAN_POINT('Ctrl Pts',(-1.95670857405052,-0.0510170594794435,
9.22702533328292));
#35882=CARTESIAN_POINT('Ctrl Pts',(-1.95572375776859,-0.0762698699047084,
9.2284728459865));
#35883=CARTESIAN_POINT('Ctrl Pts',(-1.93050850489432,-0.722843258614067,
9.26553498593022));
#35884=CARTESIAN_POINT('Ctrl Pts',(-1.55290475731554,-1.35567409888606,
9.30259712587394));
#35885=CARTESIAN_POINT('Ctrl Pts',(-0.995863227266852,-1.68491214354887,
9.33965926581766));
#35886=CARTESIAN_POINT('Ctrl Pts',(-0.438821697218168,-2.01415018821168,
9.37672140576139));
#35887=CARTESIAN_POINT('Ctrl Pts',(0.297657615300397,-2.03979543726533,
9.4137835457051));
#35888=CARTESIAN_POINT('Ctrl Pts',(0.876251218790847,-1.75010180082627,
9.45084568564882));
#35889=CARTESIAN_POINT('Ctrl Pts',(1.45484482228131,-1.46040816438721,9.48790782559255));
#35890=CARTESIAN_POINT('Ctrl Pts',(1.87555271674363,-0.855375642455424,
9.52496996553627));
#35891=CARTESIAN_POINT('Ctrl Pts',(1.94568154283725,-0.21212227253196,9.56203210547999));
#35892=CARTESIAN_POINT('Ctrl Pts',(2.01581036893087,0.431131097391505,9.59909424542371));
#35893=CARTESIAN_POINT('Ctrl Pts',(1.73536012665579,1.11260531530666,9.63615638536743));
#35894=CARTESIAN_POINT('Ctrl Pts',(1.23278314419194,1.52017044141902,9.67321852531115));
#35895=CARTESIAN_POINT('Ctrl Pts',(0.730206161728088,1.92773556753138,9.71028066525487));
#35896=CARTESIAN_POINT('Ctrl Pts',(0.00550243907548716,2.06139160184095,
9.74734280519859));
#35897=CARTESIAN_POINT('Ctrl Pts',(-0.609398062732146,1.85992111567971,
9.78440494514231));
#35898=CARTESIAN_POINT('Ctrl Pts',(-1.22429856453979,1.65845062951848,9.82146708508603));
#35899=CARTESIAN_POINT('Ctrl Pts',(-1.72939584550245,1.12185362288641,9.85852922502976));
#35900=CARTESIAN_POINT('Ctrl Pts',(-1.89334427223443,0.495903289718102,
9.89559136497348));
#35901=CARTESIAN_POINT('Ctrl Pts',(-1.93542598326109,0.335236538822793,
9.90510434594091));
#35902=CARTESIAN_POINT('Ctrl Pts',(-1.95503184094814,0.168682937546108,
9.91461732690834));
#35903=CARTESIAN_POINT('Ctrl Pts',(-1.9535343393295,0.00178280253715055,
9.92413030787576));
#35904=CARTESIAN_POINT('Origin',(0.,0.,0.));
#35905=CARTESIAN_POINT('',(-1.95129684289216,-0.00113636086278679,10.7258696921242));
#35906=CARTESIAN_POINT('',(-1.95093054978418,-0.000550606481354719,10.6241303078758));
#35907=CARTESIAN_POINT('',(-1.954,-2.39295984553393E-16,0.));
#35908=CARTESIAN_POINT('Ctrl Pts',(-1.95129684289216,-0.00113636086278679,
10.7258696921242));
#35909=CARTESIAN_POINT('Ctrl Pts',(-1.94942963316978,0.391854106201406,
10.7035356831831));
#35910=CARTESIAN_POINT('Ctrl Pts',(-1.83442754086643,0.785903964976412,
10.6812016742419));
#35911=CARTESIAN_POINT('Ctrl Pts',(-1.61381630858742,1.10744756631717,10.6588676653008));
#35912=CARTESIAN_POINT('Ctrl Pts',(-1.24796949325566,1.64067382739912,10.6218304484723));
#35913=CARTESIAN_POINT('Ctrl Pts',(-0.591690439027595,1.97450300329055,
10.5847932316438));
#35914=CARTESIAN_POINT('Ctrl Pts',(0.0547076636758263,1.95640786233593,
10.5477560148153));
#35915=CARTESIAN_POINT('Ctrl Pts',(0.701105766379276,1.9383127213813,10.5107187979868));
#35916=CARTESIAN_POINT('Ctrl Pts',(1.33762291755807,1.56829326358058,10.4736815811584));
#35917=CARTESIAN_POINT('Ctrl Pts',(1.67312833478204,1.01552035674769,10.4366443643299));
#35918=CARTESIAN_POINT('Ctrl Pts',(2.00863375200599,0.462747449914819,10.3996071475014));
#35919=CARTESIAN_POINT('Ctrl Pts',(2.04312743527515,-0.272778905950186,
10.3625699306729));
#35920=CARTESIAN_POINT('Ctrl Pts',(1.7608042651717,-0.854535269464722,10.3255327138444));
#35921=CARTESIAN_POINT('Ctrl Pts',(1.47848109506825,-1.43629163297926,10.288495497016));
#35922=CARTESIAN_POINT('Ctrl Pts',(0.879341071592168,-1.86427800414334,
10.2514582801875));
#35923=CARTESIAN_POINT('Ctrl Pts',(0.237478981470821,-1.94273555725334,
10.214421063359));
#35924=CARTESIAN_POINT('Ctrl Pts',(-0.404383108650536,-2.02119311036335,
10.1773838465305));
#35925=CARTESIAN_POINT('Ctrl Pts',(-1.08896726541717,-1.75012184541928,
10.140346629702));
#35926=CARTESIAN_POINT('Ctrl Pts',(-1.5031122201388,-1.25351130806383,10.1033094128736));
#35927=CARTESIAN_POINT('Ctrl Pts',(-1.7917522457641,-0.907396556226723,
10.0774961726238));
#35928=CARTESIAN_POINT('Ctrl Pts',(-1.94902777514884,-0.451727225472274,
10.051682932374));
#35929=CARTESIAN_POINT('Ctrl Pts',(-1.95268202714777,0.00165579016441021,
10.0258696921242));
#35930=CARTESIAN_POINT('Ctrl Pts',(-1.9535343393295,0.00178280253715055,
9.92413030787576));
#35931=CARTESIAN_POINT('Ctrl Pts',(-1.94919764294582,-0.481552375812319,
9.95167946685205));
#35932=CARTESIAN_POINT('Ctrl Pts',(-1.76787653021499,-0.967793777264111,
9.97922862582834));
#35933=CARTESIAN_POINT('Ctrl Pts',(-1.44290486192301,-1.32238333502052,
10.0067777848046));
#35934=CARTESIAN_POINT('Ctrl Pts',(-1.00571745237828,-1.79941596688631,
10.0438399247484));
#35935=CARTESIAN_POINT('Ctrl Pts',(-0.308543060787511,-2.03817757091334,
10.0809020646921));
#35936=CARTESIAN_POINT('Ctrl Pts',(0.329297761185238,-1.92930969998698,
10.1179642046358));
#35937=CARTESIAN_POINT('Ctrl Pts',(0.967138583157977,-1.82044182906063,
10.1550263445795));
#35938=CARTESIAN_POINT('Ctrl Pts',(1.5456458355127,-1.36394448318089,10.1920884845232));
#35939=CARTESIAN_POINT('Ctrl Pts',(1.79984980484802,-0.76890421197536,10.229150624467));
#35940=CARTESIAN_POINT('Ctrl Pts',(2.05405377418334,-0.173863940769825,
10.2662127644107));
#35941=CARTESIAN_POINT('Ctrl Pts',(1.98395446049928,0.5597192557615,10.3032749043544));
#35942=CARTESIAN_POINT('Ctrl Pts',(1.62166047466929,1.09585000349956,10.3403370442981));
#35943=CARTESIAN_POINT('Ctrl Pts',(1.2593664888393,1.63198075123761,10.3773991842419));
#35944=CARTESIAN_POINT('Ctrl Pts',(0.604877830863377,1.9706590501824,10.4144613241856));
#35945=CARTESIAN_POINT('Ctrl Pts',(-0.042038551539475,1.95675976549601,
10.4515234641293));
#35946=CARTESIAN_POINT('Ctrl Pts',(-0.688954933942345,1.94286048080962,
10.488585604073));
#35947=CARTESIAN_POINT('Ctrl Pts',(-1.32829904077215,1.57638361249205,10.5256477440167));
#35948=CARTESIAN_POINT('Ctrl Pts',(-1.66723158702796,1.02518946943711,10.5627098839605));
#35949=CARTESIAN_POINT('Ctrl Pts',(-1.85446111291195,0.720704641366568,
10.5831833585989));
#35950=CARTESIAN_POINT('Ctrl Pts',(-1.95001820365716,0.359852200961074,
10.6036568332373));
#35951=CARTESIAN_POINT('Ctrl Pts',(-1.95093054978418,-0.000550606481354719,
10.6241303078758));
#35952=CARTESIAN_POINT('Origin',(0.,0.,-1.29405622560369));
#35953=CARTESIAN_POINT('',(-1.55334812646815,-0.000904610707407963,10.9559437743963));
#35954=CARTESIAN_POINT('',(-1.55659711405804,-0.00105088068675666,11.0940562256037));
#35955=CARTESIAN_POINT('',(-1.5555,-2.01987159101623E-13,-1.29405622560369));
#35956=CARTESIAN_POINT('',(0.499806597877791,1.47301514408978,11.4445));
#35957=CARTESIAN_POINT('Ctrl Pts',(-1.55334812646815,-0.000904610707408108,
10.9559437743963));
#35958=CARTESIAN_POINT('Ctrl Pts',(-1.55432667860164,-0.206859868644216,
10.9706469822836));
#35959=CARTESIAN_POINT('Ctrl Pts',(-1.42041322258558,-0.930327919713715,
11.0223874069994));
#35960=CARTESIAN_POINT('Ctrl Pts',(-0.324962964057439,-1.80887727526569,
11.1111650485437));
#35961=CARTESIAN_POINT('Ctrl Pts',(1.34445241673909,-1.25560970886474,11.2222766990291));
#35962=CARTESIAN_POINT('Ctrl Pts',(1.78171768593789,0.450698535437549,11.3333883495146));
#35963=CARTESIAN_POINT('Ctrl Pts',(0.989503531151977,1.30685679928735,11.4074627831715));
#35964=CARTESIAN_POINT('Ctrl Pts',(0.499806597877626,1.47301514408983,11.4445));
#35965=CARTESIAN_POINT('',(1.55548765964692,0.00619602180124784,11.4445));
#35966=CARTESIAN_POINT('Origin',(0.,0.,11.4445));
#35967=CARTESIAN_POINT('Ctrl Pts',(-1.55659711405804,-0.0010508806867568,
11.0940562256037));
#35968=CARTESIAN_POINT('Ctrl Pts',(-1.55726922058417,-0.079449137192624,
11.099684397238));
#35969=CARTESIAN_POINT('Ctrl Pts',(-1.51630179095532,-0.673453815214831,
11.142374708816));
#35970=CARTESIAN_POINT('Ctrl Pts',(-0.75277483453787,-1.67898453189698,
11.2221271603377));
#35971=CARTESIAN_POINT('Ctrl Pts',(1.00462758039806,-1.53944373403644,11.3333135801688));
#35972=CARTESIAN_POINT('Ctrl Pts',(1.55754888396286,-0.511266487217653,
11.4074378600563));
#35973=CARTESIAN_POINT('Ctrl Pts',(1.55548765964692,0.00619602180124784,
11.4445));
#35974=CARTESIAN_POINT('Origin',(0.,0.,-1.29405622560369));
#35975=CARTESIAN_POINT('',(-1.55445081536763,0.00131810726739325,10.2559437743963));
#35976=CARTESIAN_POINT('',(-1.55305653540906,-0.000438315446397164,10.3940562256037));
#35977=CARTESIAN_POINT('',(-1.5555,-2.01987159101623E-13,-1.29405622560369));
#35978=CARTESIAN_POINT('Ctrl Pts',(-1.55445081536763,0.00131810726739319,
10.2559437743963));
#35979=CARTESIAN_POINT('Ctrl Pts',(-1.55154181384031,-0.359601688445403,
10.2817570146461));
#35980=CARTESIAN_POINT('Ctrl Pts',(-1.24670140973274,-1.24280598265434,
10.3446074717243));
#35981=CARTESIAN_POINT('Ctrl Pts',(0.223056668548975,-1.82477852394609,
10.4444951456311));
#35982=CARTESIAN_POINT('Ctrl Pts',(1.65390974917898,-0.802670846854376,
10.5556067961165));
#35983=CARTESIAN_POINT('Ctrl Pts',(1.57153269033781,0.953897085409752,10.6667184466019));
#35984=CARTESIAN_POINT('Ctrl Pts',(0.0514163720288116,1.83756944970195,
10.7778300970874));
#35985=CARTESIAN_POINT('Ctrl Pts',(-1.30849536725084,1.14582374749785,10.8742385396855));
#35986=CARTESIAN_POINT('Ctrl Pts',(-1.55186171668149,0.311939131113674,
10.9336097654551));
#35987=CARTESIAN_POINT('Ctrl Pts',(-1.55334812646815,-0.000904610707408108,
10.9559437743963));
#35988=CARTESIAN_POINT('Ctrl Pts',(-1.55305653540906,-0.000438315446397077,
10.3940562256037));
#35989=CARTESIAN_POINT('Ctrl Pts',(-1.55364500629154,-0.232901140548306,
10.410644890909));
#35990=CARTESIAN_POINT('Ctrl Pts',(-1.39557528484751,-0.983968830408974,
10.464295696158));
#35991=CARTESIAN_POINT('Ctrl Pts',(-0.231259578302998,-1.82421227428175,
10.5550086413507));
#35992=CARTESIAN_POINT('Ctrl Pts',(1.40774638007895,-1.1829694620695,10.6661950611819));
#35993=CARTESIAN_POINT('Ctrl Pts',(1.75706993010233,0.541796064983141,10.7773814810131));
#35994=CARTESIAN_POINT('Ctrl Pts',(0.497080432048737,1.77049779856472,10.8885679008442));
#35995=CARTESIAN_POINT('Ctrl Pts',(-1.13185991314487,1.39680492671116,10.9941261490411));
#35996=CARTESIAN_POINT('Ctrl Pts',(-1.55284332390808,0.436812153822664,
11.0626222572943));
#35997=CARTESIAN_POINT('Ctrl Pts',(-1.55659711405804,-0.0010508806867568,
11.0940562256037));
#35998=CARTESIAN_POINT('Origin',(0.,0.,-1.29405622560369));
#35999=CARTESIAN_POINT('',(-1.55804728476752,2.95821195149996E-5,9.5559437743963));
#36000=CARTESIAN_POINT('',(-1.55512930646214,0.00141921665610299,9.69405622560371));
#36001=CARTESIAN_POINT('',(-1.5555,-2.01987159101623E-13,-1.29405622560369));
#36002=CARTESIAN_POINT('Ctrl Pts',(-1.55804728476752,2.95821195150548E-5,
9.5559437743963));
#36003=CARTESIAN_POINT('Ctrl Pts',(-1.55790353315504,-0.513149683984934,
9.59286704700854));
#36004=CARTESIAN_POINT('Ctrl Pts',(-1.00033131917675,-1.54135965233235,
9.66682753644926));
#36005=CARTESIAN_POINT('Ctrl Pts',(0.750970673805211,-1.67799333720618,
9.77782524271844));
#36006=CARTESIAN_POINT('Ctrl Pts',(1.81699613594968,-0.279545920640164,
9.88893689320389));
#36007=CARTESIAN_POINT('Ctrl Pts',(1.22062258834496,1.37466418983892,10.0000485436893));
#36008=CARTESIAN_POINT('Ctrl Pts',(-0.492515922639386,1.77116921324136,
10.1111601941748));
#36009=CARTESIAN_POINT('Ctrl Pts',(-1.46173837715872,0.831558022400444,
10.1964586044104));
#36010=CARTESIAN_POINT('Ctrl Pts',(-1.55571569202373,0.15825134364817,10.2447197978176));
#36011=CARTESIAN_POINT('Ctrl Pts',(-1.55445081536763,0.00131810726739319,
10.2559437743963));
#36012=CARTESIAN_POINT('Ctrl Pts',(-1.55512930646214,0.00141921665610296,
9.69405622560371));
#36013=CARTESIAN_POINT('Ctrl Pts',(-1.55167703869094,-0.383344278698275,
9.72160538457999));
#36014=CARTESIAN_POINT('Ctrl Pts',(-1.21314953523015,-1.29115961930375,
9.7862166835));
#36015=CARTESIAN_POINT('Ctrl Pts',(0.309373610575528,-1.81257875466721,
9.88789012236375));
#36016=CARTESIAN_POINT('Ctrl Pts',(1.69095195914933,-0.722381792257861,
9.99907654219489));
#36017=CARTESIAN_POINT('Ctrl Pts',(1.52354231364944,1.0295455294481,10.1102629620261));
#36018=CARTESIAN_POINT('Ctrl Pts',(-0.0394931635484403,1.83836962465064,
10.2214493818572));
#36019=CARTESIAN_POINT('Ctrl Pts',(-1.33855689695156,1.09373648628768,10.3160471363831));
#36020=CARTESIAN_POINT('Ctrl Pts',(-1.5523302537302,0.286463714736223,10.3735827509653));
#36021=CARTESIAN_POINT('Ctrl Pts',(-1.55305653540906,-0.000438315446397077,
10.3940562256037));
#36022=CARTESIAN_POINT('Origin',(0.,0.,-1.29405622560369));
#36023=CARTESIAN_POINT('',(-1.55453687436568,-0.00133745576774406,8.85594377439631));
#36024=CARTESIAN_POINT('',(-1.55794751152569,-0.000371416033132788,8.99405622560372));
#36025=CARTESIAN_POINT('',(-1.5555,-2.01987159101623E-13,-1.29405622560369));
#36026=CARTESIAN_POINT('Ctrl Pts',(-1.55453687436568,-0.00133745576774402,
8.85594377439631));
#36027=CARTESIAN_POINT('Ctrl Pts',(-1.55579877499581,-0.155062375664632,
8.86693986254252));
#36028=CARTESIAN_POINT('Ctrl Pts',(-1.46423861786649,-0.825096309536398,
8.91497316751722));
#36029=CARTESIAN_POINT('Ctrl Pts',(-0.503376402892206,-1.7681153483915,
9.00004368932038));
#36030=CARTESIAN_POINT('Ctrl Pts',(1.2121644264892,-1.38212772940753,9.11115533980582));
#36031=CARTESIAN_POINT('Ctrl Pts',(1.81867711471885,0.26839009932345,9.22226699029127));
#36032=CARTESIAN_POINT('Ctrl Pts',(0.761253709552246,1.67335367481701,9.33337864077668));
#36033=CARTESIAN_POINT('Ctrl Pts',(-0.99265255914171,1.54733978795034,9.44449029126215));
#36034=CARTESIAN_POINT('Ctrl Pts',(-1.55732851093913,0.517959404958592,
9.51867866913534));
#36035=CARTESIAN_POINT('Ctrl Pts',(-1.55804772838109,0.00161323939398619,
9.55582983018006));
#36036=CARTESIAN_POINT('Ctrl Pts',(-1.55804728476752,2.95821195150548E-5,
9.5559437743963));
#36037=CARTESIAN_POINT('Ctrl Pts',(-1.55794751152569,-0.000371416033132616,
8.99405622560372));
#36038=CARTESIAN_POINT('Ctrl Pts',(-1.55801224941728,-0.020493184051098,
8.99550373830729));
#36039=CARTESIAN_POINT('Ctrl Pts',(-1.54853952527048,-0.55575068168544,
9.03401339095459));
#36040=CARTESIAN_POINT('Ctrl Pts',(-0.935609375970031,-1.5829679799695,
9.1095851835456));
#36041=CARTESIAN_POINT('Ctrl Pts',(0.823234386500799,-1.64421340203127,
9.22077160337675));
#36042=CARTESIAN_POINT('Ctrl Pts',(1.82795976495949,-0.199287985657338,
9.33195802320793));
#36043=CARTESIAN_POINT('Ctrl Pts',(1.15819463928053,1.42819381470141,9.44314444303908));
#36044=CARTESIAN_POINT('Ctrl Pts',(-0.572526917402423,1.74738822826618,
9.55433086287024));
#36045=CARTESIAN_POINT('Ctrl Pts',(-1.47990815776177,0.783419353749631,
9.63796812372513));
#36046=CARTESIAN_POINT('Ctrl Pts',(-1.5563214066504,0.1342816322173,9.68454324463628));
#36047=CARTESIAN_POINT('Ctrl Pts',(-1.55512930646214,0.00141921665610296,
9.69405622560371));
#36048=CARTESIAN_POINT('Origin',(0.,0.,-1.29405622560369));
#36049=CARTESIAN_POINT('',(-1.55333906144275,0.000780263919018194,8.15594377439631));
#36050=CARTESIAN_POINT('',(-1.55403083159801,-0.00119596074553197,8.29405622560371));
#36051=CARTESIAN_POINT('',(-1.5555,-2.01987159101623E-13,-1.29405622560369));
#36052=CARTESIAN_POINT('Ctrl Pts',(-1.55333906144275,0.000780263919018167,
8.15594377439631));
#36053=CARTESIAN_POINT('Ctrl Pts',(-1.55193217426013,-0.308862600127516,
8.17804989490498));
#36054=CARTESIAN_POINT('Ctrl Pts',(-1.3122308335565,-1.13929638534857,8.23719323224213));
#36055=CARTESIAN_POINT('Ctrl Pts',(0.0400949547363229,-1.83793690702293,
8.33337378640777));
#36056=CARTESIAN_POINT('Ctrl Pts',(1.56567267939011,-0.963477420579929,
8.44448543689319));
#36057=CARTESIAN_POINT('Ctrl Pts',(1.65879203582308,0.792482593671729,8.55559708737864));
#36058=CARTESIAN_POINT('Ctrl Pts',(0.234256671005791,1.82338791618694,8.66670873786407));
#36059=CARTESIAN_POINT('Ctrl Pts',(-1.24241507899534,1.24912116508194,8.7668243002033));
#36060=CARTESIAN_POINT('Ctrl Pts',(-1.55154841917538,0.362716593952071,
8.82990264571404));
#36061=CARTESIAN_POINT('Ctrl Pts',(-1.55453687436568,-0.00133745576774402,
8.85594377439631));
#36062=CARTESIAN_POINT('Ctrl Pts',(-1.55403083159801,-0.00119596074553188,
8.29405622560371));
#36063=CARTESIAN_POINT('Ctrl Pts',(-1.55527408252746,-0.17480188940304,
8.30646423197829));
#36064=CARTESIAN_POINT('Ctrl Pts',(-1.4483135129372,-0.865473027753662,
8.3559343782966));
#36065=CARTESIAN_POINT('Ctrl Pts',(-0.434704832044991,-1.78666848096071,
8.44246666455862));
#36066=CARTESIAN_POINT('Ctrl Pts',(1.26590215885116,-1.33365823077974,8.55365308438979));
#36067=CARTESIAN_POINT('Ctrl Pts',(1.8068878531032,0.341040818691465,8.66483950422094));
#36068=CARTESIAN_POINT('Ctrl Pts',(0.69268588294083,1.70333168137465,8.77602592405212));
#36069=CARTESIAN_POINT('Ctrl Pts',(-1.03328002592178,1.50787500329959,8.88576483117969));
#36070=CARTESIAN_POINT('Ctrl Pts',(-1.55635469933735,0.494704907375218,
8.95844159836357));
#36071=CARTESIAN_POINT('Ctrl Pts',(-1.55794751152569,-0.000371416033132616,
8.99405622560372));
#36072=CARTESIAN_POINT('Origin',(0.,0.,-1.29405622560369));
#36073=CARTESIAN_POINT('',(-1.55738164088485,0.00090367155389158,7.45594377439631));
#36074=CARTESIAN_POINT('',(-1.55363820104426,0.00100737127591941,7.59405622560371));
#36075=CARTESIAN_POINT('',(-1.5555,-2.01987159101623E-13,-1.29405622560369));
#36076=CARTESIAN_POINT('Ctrl Pts',(-1.55738164088485,0.000903671553891608,
7.45594377439631));
#36077=CARTESIAN_POINT('Ctrl Pts',(-1.55418612064456,-0.461276292775272,
7.48915992726744));
#36078=CARTESIAN_POINT('Ctrl Pts',(-1.09121796390773,-1.44436334125619,
7.55941329696705));
#36079=CARTESIAN_POINT('Ctrl Pts',(0.580004387659595,-1.74448118065669,
7.66670388349515));
#36080=CARTESIAN_POINT('Ctrl Pts',(1.7800908511122,-0.459234407622611,7.77781553398057));
#36081=CARTESIAN_POINT('Ctrl Pts',(1.35154441460109,1.24617309179735,7.88892718446602));
#36082=CARTESIAN_POINT('Ctrl Pts',(-0.313551099181417,1.81143738163968,
8.00003883495145));
#36083=CARTESIAN_POINT('Ctrl Pts',(-1.41757073229054,0.936656796997624,
8.08904436492822));
#36084=CARTESIAN_POINT('Ctrl Pts',(-1.55428931266511,0.209921774117757,
8.1410126780765));
#36085=CARTESIAN_POINT('Ctrl Pts',(-1.55333906144275,0.000780263919018167,
8.15594377439631));
#36086=CARTESIAN_POINT('Ctrl Pts',(-1.55363820104426,0.00100737127591942,
7.59405622560371));
#36087=CARTESIAN_POINT('Ctrl Pts',(-1.55169765832855,-0.326159426902871,
7.6174247256493));
#36088=CARTESIAN_POINT('Ctrl Pts',(-1.29071878250434,-1.17503987929593,
7.67785536563862));
#36089=CARTESIAN_POINT('Ctrl Pts',(0.103792628149562,-1.8358593744105,7.77534814557165));
#36090=CARTESIAN_POINT('Ctrl Pts',(1.59909575810308,-0.907769413831382,
7.8865345654028));
#36091=CARTESIAN_POINT('Ctrl Pts',(1.62955779866738,0.851876712390422,7.99772098523398));
#36092=CARTESIAN_POINT('Ctrl Pts',(0.167274199086701,1.83116681231986,8.10890740506512));
#36093=CARTESIAN_POINT('Ctrl Pts',(-1.26795424285233,1.21093838634352,8.20768581852172));
#36094=CARTESIAN_POINT('Ctrl Pts',(-1.55156054962447,0.343750973057136,
8.26940209203457));
#36095=CARTESIAN_POINT('Ctrl Pts',(-1.55403083159801,-0.00119596074553188,
8.29405622560371));
#36096=CARTESIAN_POINT('Origin',(0.,0.,-1.29405622560369));
#36097=CARTESIAN_POINT('',(-1.55606466149984,-0.00136591087330588,6.7559437743963));
#36098=CARTESIAN_POINT('',(-1.55769406638298,0.000677585252333857,6.89405622560371));
#36099=CARTESIAN_POINT('',(-1.5555,-2.01987159101623E-13,-1.29405622560369));
#36100=CARTESIAN_POINT('Ctrl Pts',(-1.55606466149984,-0.00136591087330577,
6.7559437743963));
#36101=CARTESIAN_POINT('Ctrl Pts',(-1.55699698050756,-0.10301028373747,
6.76323274280142));
#36102=CARTESIAN_POINT('Ctrl Pts',(-1.50160999329305,-0.720125819190329,
6.80755892803501));
#36103=CARTESIAN_POINT('Ctrl Pts',(-0.677079673289082,-1.70914680334463,
6.8889223300971));
#36104=CARTESIAN_POINT('Ctrl Pts',(1.06838781720774,-1.49605051766532,7.00003398058251));
#36105=CARTESIAN_POINT('Ctrl Pts',(1.83637062036826,0.0858057341481814,
7.11114563106797));
#36106=CARTESIAN_POINT('Ctrl Pts',(0.924229284360448,1.589156980696,7.22225728155339));
#36107=CARTESIAN_POINT('Ctrl Pts',(-0.833503847528551,1.63856370505402,
7.33336893203883));
#36108=CARTESIAN_POINT('Ctrl Pts',(-1.53115801604342,0.622214122864029,
7.41126442965314));
#36109=CARTESIAN_POINT('Ctrl Pts',(-1.55774924177056,0.0540711533618156,
7.45212271043896));
#36110=CARTESIAN_POINT('Ctrl Pts',(-1.55738164088485,0.000903671553891608,
7.45594377439631));
#36111=CARTESIAN_POINT('Ctrl Pts',(-1.55769406638298,0.000677585252333878,
6.89405622560371));
#36112=CARTESIAN_POINT('Ctrl Pts',(-1.55508734647919,-0.476733936548398,
6.92838521932031));
#36113=CARTESIAN_POINT('Ctrl Pts',(-1.06472330039144,-1.47419539900055,
6.99977635298063));
#36114=CARTESIAN_POINT('Ctrl Pts',(0.633314188332071,-1.72628667698419,
7.10822962658467));
#36115=CARTESIAN_POINT('Ctrl Pts',(1.7940008868909,-0.403377453646542,7.21941604641583));
#36116=CARTESIAN_POINT('Ctrl Pts',(1.31130494233742,1.28904301731096,7.33060246624699));
#36117=CARTESIAN_POINT('Ctrl Pts',(-0.372603218894873,1.80064416072257,
7.44178888607816));
#36118=CARTESIAN_POINT('Ctrl Pts',(-1.43301362666466,0.901927254173143,
7.52960680586373));
#36119=CARTESIAN_POINT('Ctrl Pts',(-1.55477533406966,0.192722899107996,
7.58036258570558));
#36120=CARTESIAN_POINT('Ctrl Pts',(-1.55363820104426,0.00100737127591942,
7.59405622560371));
#36121=CARTESIAN_POINT('Origin',(0.,0.,-1.29405622560369));
#36122=CARTESIAN_POINT('',(-1.55295085115974,-2.74912889200857E-5,6.0559437743963));
#36123=CARTESIAN_POINT('',(-1.55567057787938,-0.00141549514015751,6.19405622560371));
#36124=CARTESIAN_POINT('',(-1.5555,-2.01987159101623E-13,-1.29405622560369));
#36125=CARTESIAN_POINT('Ctrl Pts',(-1.55295114066544,-2.74881667468134E-5,
6.0559437743963));
#36126=CARTESIAN_POINT('Ctrl Pts',(-1.55299180574127,-0.257905198155464,
6.07434277516388));
#36127=CARTESIAN_POINT('Ctrl Pts',(-1.37005956536857,-1.03483686203599,
6.12977899275993));
#36128=CARTESIAN_POINT('Ctrl Pts',(-0.143272298638598,-1.83278278249422,
6.22225242718446));
#36129=CARTESIAN_POINT('Ctrl Pts',(1.46185859526926,-1.11471481859797,6.33336407766989));
#36130=CARTESIAN_POINT('Ctrl Pts',(1.72951224644592,0.623223129190563,6.44447572815534));
#36131=CARTESIAN_POINT('Ctrl Pts',(0.414808152398764,1.79096450999678,6.55558737864077));
#36132=CARTESIAN_POINT('Ctrl Pts',(-1.1682689842466,1.35101180160119,6.6594100607211));
#36133=CARTESIAN_POINT('Ctrl Pts',(-1.55225961585962,0.413472223515983,
6.72619552597294));
#36134=CARTESIAN_POINT('Ctrl Pts',(-1.55606466149984,-0.00136591087330577,
6.7559437743963));
#36135=CARTESIAN_POINT('Ctrl Pts',(-1.55567057787938,-0.00141549514015748,
6.19405622560371));
#36136=CARTESIAN_POINT('Ctrl Pts',(-1.55673152840384,-0.11622012238534,
6.2022835730476));
#36137=CARTESIAN_POINT('Ctrl Pts',(-1.49271086742403,-0.747018195902368,
6.2475730604352));
#36138=CARTESIAN_POINT('Ctrl Pts',(-0.632665469493242,-1.72652453095426,
6.32992468776653));
#36139=CARTESIAN_POINT('Ctrl Pts',(1.10806726459172,-1.46742614445027,6.44111110759769));
#36140=CARTESIAN_POINT('Ctrl Pts',(1.83376231205259,0.135898253011021,6.55229752742886));
#36141=CARTESIAN_POINT('Ctrl Pts',(0.879651525947856,1.61473395492061,6.66348394726001));
#36142=CARTESIAN_POINT('Ctrl Pts',(-0.880258220622017,1.61440330069759,
6.77467036709119));
#36143=CARTESIAN_POINT('Ctrl Pts',(-1.53940153309356,0.591912849892102,
6.85152779320574));
#36144=CARTESIAN_POINT('Ctrl Pts',(-1.55790160368306,0.0386873070159844,
6.89132307937659));
#36145=CARTESIAN_POINT('Ctrl Pts',(-1.55769406638298,0.000677585252333878,
6.89405622560371));
#36146=CARTESIAN_POINT('Origin',(0.,0.,-1.29405622560369));
#36147=CARTESIAN_POINT('',(-1.55596383579478,0.00138071545366175,5.3559437743963));
#36148=CARTESIAN_POINT('',(-1.5529563387483,0.000151106445085702,5.49405622560371));
#36149=CARTESIAN_POINT('',(-1.5555,-2.01987159101623E-13,-1.29405622560369));
#36150=CARTESIAN_POINT('Ctrl Pts',(-1.55596383579478,0.00138071545366179,
5.3559437743963));
#36151=CARTESIAN_POINT('Ctrl Pts',(-1.55217514150148,-0.410190199764792,
5.38545280752634));
#36152=CARTESIAN_POINT('Ctrl Pts',(-1.17330640529453,-1.34449549172498,
5.45199905748485));
#36153=CARTESIAN_POINT('Ctrl Pts',(0.403262995152723,-1.79359935217008,
5.55558252427184));
#36154=CARTESIAN_POINT('Ctrl Pts',(1.72546185411942,-0.634350903950841,
5.66669417475728));
#36155=CARTESIAN_POINT('Ctrl Pts',(1.46900873501267,1.1052750860401,5.77780582524271));
#36156=CARTESIAN_POINT('Ctrl Pts',(-0.13146340126236,1.83366765077345,5.88891747572816));
#36157=CARTESIAN_POINT('Ctrl Pts',(-1.36655195880861,1.04159698732297,5.98163012544601));
#36158=CARTESIAN_POINT('Ctrl Pts',(-1.55290994688111,0.261203028467153,
6.0373055583354));
#36159=CARTESIAN_POINT('Ctrl Pts',(-1.55295114066544,-2.74881667468134E-5,
6.0559437743963));
#36160=CARTESIAN_POINT('Ctrl Pts',(-1.5529563387483,0.000151106445085633,
5.49405622560371));
#36161=CARTESIAN_POINT('Ctrl Pts',(-1.55272340811799,-0.268780222436924,
5.5132440667186));
#36162=CARTESIAN_POINT('Ctrl Pts',(-1.35831396530156,-1.05747938365068,
5.56949404777722));
#36163=CARTESIAN_POINT('Ctrl Pts',(-0.103102773360761,-1.83589824620028,
5.66280616877956));
#36164=CARTESIAN_POINT('Ctrl Pts',(1.4869956060099,-1.08166382022474,5.77399258861071));
#36165=CARTESIAN_POINT('Ctrl Pts',(1.71494149863546,0.663421591850831,5.88517900844189));
#36166=CARTESIAN_POINT('Ctrl Pts',(0.371926577693494,1.80078404398782,5.99636542827304));
#36167=CARTESIAN_POINT('Ctrl Pts',(-1.18720103315053,1.32645343006727,6.09932450066032));
#36168=CARTESIAN_POINT('Ctrl Pts',(-1.55195221197423,0.40094597399841,6.16522143310387));
#36169=CARTESIAN_POINT('Ctrl Pts',(-1.55567057787938,-0.00141549514015748,
6.19405622560371));
#36170=CARTESIAN_POINT('Origin',(0.,0.,-1.29405622560369));
#36171=CARTESIAN_POINT('',(-1.55745492001379,-0.000856371120316566,4.6559437743963));
#36172=CARTESIAN_POINT('',(-1.55622585425313,0.00134239099646036,4.79405622560371));
#36173=CARTESIAN_POINT('',(-1.5555,-2.01987159101623E-13,-1.29405622560369));
#36174=CARTESIAN_POINT('Ctrl Pts',(-1.55745492001379,-0.000856371120316864,
4.65594377439631));
#36175=CARTESIAN_POINT('Ctrl Pts',(-1.5577850741697,-0.0506891626144068,
4.65952562306032));
#36176=CARTESIAN_POINT('Ctrl Pts',(-1.53301192978291,-0.615473136307116,
4.70014468855281));
#36177=CARTESIAN_POINT('Ctrl Pts',(-0.844041411881997,-1.63316067010957,
4.77780097087378));
#36178=CARTESIAN_POINT('Ctrl Pts',(0.913973507436636,-1.59507746114991,
4.88891262135923));
#36179=CARTESIAN_POINT('Ctrl Pts',(1.83577980123458,-0.0976329900371924,
5.00002427184466));
#36180=CARTESIAN_POINT('Ctrl Pts',(1.0780025055099,1.48913742733129,5.1111359223301));
#36181=CARTESIAN_POINT('Ctrl Pts',(-0.666056105926533,1.7134727727987,5.22224757281553));
#36182=CARTESIAN_POINT('Ctrl Pts',(-1.49938299705611,0.726891414718789,
5.30385019017093));
#36183=CARTESIAN_POINT('Ctrl Pts',(-1.55693038683329,0.106378444150779,
5.34841559069786));
#36184=CARTESIAN_POINT('Ctrl Pts',(-1.55596383579478,0.00138071545366179,
5.3559437743963));
#36185=CARTESIAN_POINT('Ctrl Pts',(-1.55622585425313,0.00134239099646029,
4.79405622560371));
#36186=CARTESIAN_POINT('Ctrl Pts',(-1.55239700220769,-0.418962472451577,
4.82420456038961));
#36187=CARTESIAN_POINT('Ctrl Pts',(-1.15964303797854,-1.36226320639006,
4.89141503511923));
#36188=CARTESIAN_POINT('Ctrl Pts',(0.435376164803608,-1.7865050090601,4.99568764979258));
#36189=CARTESIAN_POINT('Ctrl Pts',(1.73732980498774,-0.602360109052031,
5.10687406962374));
#36190=CARTESIAN_POINT('Ctrl Pts',(1.44781397169404,1.13357278356683,5.21806048945491));
#36191=CARTESIAN_POINT('Ctrl Pts',(-0.167962271460079,1.83110382765203,
5.32924690928607));
#36192=CARTESIAN_POINT('Ctrl Pts',(-1.37758975876034,1.02035875886683,5.42124548800234));
#36193=CARTESIAN_POINT('Ctrl Pts',(-1.55317332364345,0.250672199885809,
5.47618192677488));
#36194=CARTESIAN_POINT('Ctrl Pts',(-1.5529563387483,0.000151106445085633,
5.49405622560371));
#36195=CARTESIAN_POINT('Origin',(0.,0.,-1.29405622560369));
#36196=CARTESIAN_POINT('',(-1.55339129538237,-0.00082587420025254,3.9559437743963));
#36197=CARTESIAN_POINT('',(-1.5573160577951,-0.00094952305265919,4.09405622560371));
#36198=CARTESIAN_POINT('',(-1.5555,-2.01987159101623E-13,-1.29405622560369));
#36199=CARTESIAN_POINT('Ctrl Pts',(-1.55339129538237,-0.000825874200252562,
3.9559437743963));
#36200=CARTESIAN_POINT('Ctrl Pts',(-1.55438295724494,-0.206599346759669,
3.97063565542278));
#36201=CARTESIAN_POINT('Ctrl Pts',(-1.42062281789543,-0.929876204718288,
4.02236475327773));
#36202=CARTESIAN_POINT('Ctrl Pts',(-0.325213021862407,-1.80938005122649,
4.11113106796117));
#36203=CARTESIAN_POINT('Ctrl Pts',(1.34348911316817,-1.25485325124609,4.2222427184466));
#36204=CARTESIAN_POINT('Ctrl Pts',(1.78301209192838,0.447758371671112,4.33335436893204));
#36205=CARTESIAN_POINT('Ctrl Pts',(0.591229481908682,1.74070887258225,4.44446601941748));
#36206=CARTESIAN_POINT('Ctrl Pts',(-1.0856218085317,1.45071736103991,4.55199582123889));
#36207=CARTESIAN_POINT('Ctrl Pts',(-1.55437119708937,0.464594445617744,
4.62248840623184));
#36208=CARTESIAN_POINT('Ctrl Pts',(-1.55745492001379,-0.000856371120316864,
4.65594377439631));
#36209=CARTESIAN_POINT('Ctrl Pts',(-1.5573160577951,-0.000949523052659442,
4.0940562256037));
#36210=CARTESIAN_POINT('Ctrl Pts',(-1.55772052747877,-0.0572626470532979,
4.0981029141169));
#36211=CARTESIAN_POINT('Ctrl Pts',(-1.52938259291224,-0.628915705084586,
4.13921174257381));
#36212=CARTESIAN_POINT('Ctrl Pts',(-0.822616502622442,-1.64452261823584,
4.21738271097444));
#36213=CARTESIAN_POINT('Ctrl Pts',(0.936204134582059,-1.58261630557358,
4.3285691308056));
#36214=CARTESIAN_POINT('Ctrl Pts',(1.83742116834086,-0.0709647969689106,
4.43975555063676));
#36215=CARTESIAN_POINT('Ctrl Pts',(1.0554806974386,1.50569354438759,4.55094197046793));
#36216=CARTESIAN_POINT('Ctrl Pts',(-0.693325883166112,1.70307127625589,
4.66212839029909));
#36217=CARTESIAN_POINT('Ctrl Pts',(-1.50503746143118,0.709862178387775,
4.74316647534435));
#36218=CARTESIAN_POINT('Ctrl Pts',(-1.55710391061042,0.0977293375193425,
4.78714242044589));
#36219=CARTESIAN_POINT('Ctrl Pts',(-1.55622585425313,0.00134239099646029,
4.79405622560371));
#36220=CARTESIAN_POINT('Origin',(0.,0.,-1.29405622560369));
#36221=CARTESIAN_POINT('',(-1.55444674488022,0.00131742778884735,3.2559437743963));
#36222=CARTESIAN_POINT('',(-1.5533186684889,-0.000770198572060954,3.39405622560371));
#36223=CARTESIAN_POINT('',(-1.5555,-2.01987159101623E-13,-1.29405622560369));
#36224=CARTESIAN_POINT('Ctrl Pts',(-1.55444674488022,0.00131742778884739,
3.2559437743963));
#36225=CARTESIAN_POINT('Ctrl Pts',(-1.55154236665719,-0.359445316439912,
3.28174568778523));
#36226=CARTESIAN_POINT('Ctrl Pts',(-1.24691611905359,-1.24248704432008,
3.34458481800264));
#36227=CARTESIAN_POINT('Ctrl Pts',(0.222506403513669,-1.8248590575151,3.44446116504855));
#36228=CARTESIAN_POINT('Ctrl Pts',(1.65365282072159,-0.803151310699741,
3.55557281553397));
#36229=CARTESIAN_POINT('Ctrl Pts',(1.57184646516792,0.953372104320743,3.66668446601942));
#36230=CARTESIAN_POINT('Ctrl Pts',(0.0519332482321354,1.83764050268212,
3.77779611650485));
#36231=CARTESIAN_POINT('Ctrl Pts',(-1.30823935507303,1.14600960175539,3.87421588596382));
#36232=CARTESIAN_POINT('Ctrl Pts',(-1.55188304621527,0.312141358191517,
3.9335984385943));
#36233=CARTESIAN_POINT('Ctrl Pts',(-1.55339129538237,-0.000825874200252562,
3.9559437743963));
#36234=CARTESIAN_POINT('Ctrl Pts',(-1.5533186684889,-0.000770198572060919,
3.39405622560371));
#36235=CARTESIAN_POINT('Ctrl Pts',(-1.5542597194186,-0.210984061911746,
3.4090634077879));
#36236=CARTESIAN_POINT('Ctrl Pts',(-1.41654850766895,-0.939166341982764,
3.46113272991582));
#36237=CARTESIAN_POINT('Ctrl Pts',(-0.308692884081366,-1.81269447386996,
3.55026419198746));
#36238=CARTESIAN_POINT('Ctrl Pts',(1.35606994996762,-1.24186426112907,3.66145061181863));
#36239=CARTESIAN_POINT('Ctrl Pts',(1.77861387826841,0.466567491694538,3.77263703164979));
#36240=CARTESIAN_POINT('Ctrl Pts',(0.571870330903418,1.74760318061885,3.88382345148095));
#36241=CARTESIAN_POINT('Ctrl Pts',(-1.09574509035902,1.43939945308724,3.99096318279893));
#36242=CARTESIAN_POINT('Ctrl Pts',(-1.55401613758806,0.458488658137791,
4.06104077417318));
#36243=CARTESIAN_POINT('Ctrl Pts',(-1.5573160577951,-0.000949523052659442,
4.0940562256037));
#36244=CARTESIAN_POINT('Origin',(0.,0.,-1.29405622560369));
#36245=CARTESIAN_POINT('',(-1.55804712705668,3.25009013604671E-5,2.5559437743963));
#36246=CARTESIAN_POINT('',(-1.55449947323643,0.00133480041304715,2.69405622560371));
#36247=CARTESIAN_POINT('',(-1.5555,-2.01987159101623E-13,-1.29405622560369));
#36248=CARTESIAN_POINT('Ctrl Pts',(-1.55804712705668,3.25009013604029E-5,
2.5559437743963));
#36249=CARTESIAN_POINT('Ctrl Pts',(-1.55788927539753,-0.512989453804214,
2.59285572014769));
#36250=CARTESIAN_POINT('Ctrl Pts',(-1.0006227616332,-1.54106832868198,2.66680488272757));
#36251=CARTESIAN_POINT('Ctrl Pts',(0.750458968510211,-1.67822257683237,
2.77779126213592));
#36252=CARTESIAN_POINT('Ctrl Pts',(1.81691053470019,-0.280099604209337,
2.88890291262136));
#36253=CARTESIAN_POINT('Ctrl Pts',(1.22104229764526,1.37429086670804,3.0000145631068));
#36254=CARTESIAN_POINT('Ctrl Pts',(-0.491976593161155,1.77132117679823,
3.11112621359223));
#36255=CARTESIAN_POINT('Ctrl Pts',(-1.46161229246342,0.831876851886141,
3.19643595068874));
#36256=CARTESIAN_POINT('Ctrl Pts',(-1.55571144064704,0.158409610837222,
3.24470847095676));
#36257=CARTESIAN_POINT('Ctrl Pts',(-1.55444674488022,0.00131742778884739,
3.2559437743963));
#36258=CARTESIAN_POINT('Ctrl Pts',(-1.55449947323643,0.00133480041304701,
2.69405622560371));
#36259=CARTESIAN_POINT('Ctrl Pts',(-1.55153406972295,-0.361714100102126,
2.72002390145891));
#36260=CARTESIAN_POINT('Ctrl Pts',(-1.2437032104418,-1.24745277135715,2.78305371725784));
#36261=CARTESIAN_POINT('Ctrl Pts',(0.231926238140432,-1.82410602009977,
2.88314567300049));
#36262=CARTESIAN_POINT('Ctrl Pts',(1.65866396469461,-0.793716828903688,
2.99433209283165));
#36263=CARTESIAN_POINT('Ctrl Pts',(1.56599354026699,0.96375141196464,3.10551851266282));
#36264=CARTESIAN_POINT('Ctrl Pts',(0.0388050940998321,1.83838154825996,
3.21670493249398));
#36265=CARTESIAN_POINT('Ctrl Pts',(-1.31300314367493,1.13822266482633,3.31288417014094));
#36266=CARTESIAN_POINT('Ctrl Pts',(-1.55193567478298,0.308165737536199,
3.37200126784418));
#36267=CARTESIAN_POINT('Ctrl Pts',(-1.5533186684889,-0.000770198572060919,
3.39405622560371));
#36268=CARTESIAN_POINT('Origin',(0.,0.,-1.29405622560369));
#36269=CARTESIAN_POINT('',(-1.55454118234884,-0.00133834695600709,1.8559437743963));
#36270=CARTESIAN_POINT('',(-1.55805467550008,3.4854191793785E-5,1.9940562256037));
#36271=CARTESIAN_POINT('',(-1.5555,-2.01987159101623E-13,-1.29405622560369));
#36272=CARTESIAN_POINT('Ctrl Pts',(-1.55454118234884,-0.00133834695600729,
1.8559437743963));
#36273=CARTESIAN_POINT('Ctrl Pts',(-1.55580288786201,-0.154903851691022,
1.86692853568168));
#36274=CARTESIAN_POINT('Ctrl Pts',(-1.46436232298065,-0.824775316270878,
1.91495051379553));
#36275=CARTESIAN_POINT('Ctrl Pts',(-0.503915664640746,-1.76796168665343,
2.00000970873786));
#36276=CARTESIAN_POINT('Ctrl Pts',(1.21174280763407,-1.38249741391359,2.1111213592233));
#36277=CARTESIAN_POINT('Ctrl Pts',(1.81875888824183,0.267835396201195,2.22223300970874));
#36278=CARTESIAN_POINT('Ctrl Pts',(0.761764071097843,1.67312138149853,2.33334466019417));
#36279=CARTESIAN_POINT('Ctrl Pts',(-0.992180579104728,1.54764252547341,
2.44445631067961));
#36280=CARTESIAN_POINT('Ctrl Pts',(-1.55725669913861,0.518277207581445,
2.51865601541365));
#36281=CARTESIAN_POINT('Ctrl Pts',(-1.55804766277071,0.0017735852989955,
2.55581850331921));
#36282=CARTESIAN_POINT('Ctrl Pts',(-1.55804712705668,3.25009013604029E-5,
2.5559437743963));
#36283=CARTESIAN_POINT('Ctrl Pts',(-1.55805467550008,3.48541917938314E-5,
1.9940562256037));
#36284=CARTESIAN_POINT('Ctrl Pts',(-1.55788564535512,-0.513206116891616,
2.03098439512992));
#36285=CARTESIAN_POINT('Ctrl Pts',(-1.00003893378143,-1.54186484140614,
2.10497470459985));
#36286=CARTESIAN_POINT('Ctrl Pts',(0.752488571272716,-1.67777039880966,
2.21602715401351));
#36287=CARTESIAN_POINT('Ctrl Pts',(1.81781810074028,-0.276929424335053,
2.32721357384467));
#36288=CARTESIAN_POINT('Ctrl Pts',(1.21794738393109,1.37759091140133,2.43839999367584));
#36289=CARTESIAN_POINT('Ctrl Pts',(-0.497615974795104,1.77017821004958,
2.549586413507));
#36290=CARTESIAN_POINT('Ctrl Pts',(-1.46313162187878,0.828233020270418,
2.63480515748296));
#36291=CARTESIAN_POINT('Ctrl Pts',(-1.55576641614544,0.156444291597347,
2.68296176151519));
#36292=CARTESIAN_POINT('Ctrl Pts',(-1.55449947323643,0.00133480041304701,
2.69405622560371));
#36293=CARTESIAN_POINT('Origin',(0.,0.,-1.29405622560369));
#36294=CARTESIAN_POINT('',(-1.55333634177863,0.000779921548230329,1.1559437743963));
#36295=CARTESIAN_POINT('',(-1.55460191805193,-0.00135568056800359,1.2940562256037));
#36296=CARTESIAN_POINT('',(-1.5555,-2.01987159101623E-13,-1.29405622560369));
#36297=CARTESIAN_POINT('Ctrl Pts',(-1.55333634177863,0.000779921548230561,
1.1559437743963));
#36298=CARTESIAN_POINT('Ctrl Pts',(-1.55193438638927,-0.308706275100063,
1.17803856804414));
#36299=CARTESIAN_POINT('Ctrl Pts',(-1.31241956589738,-1.1389814578602,1.23717057852045));
#36300=CARTESIAN_POINT('Ctrl Pts',(0.0395347168138628,-1.83794704008407,
1.33333980582524));
#36301=CARTESIAN_POINT('Ctrl Pts',(1.56537855283131,-0.963955976349113,
1.44445145631068));
#36302=CARTESIAN_POINT('Ctrl Pts',(1.65903376979378,0.791977165381959,1.55556310679611));
#36303=CARTESIAN_POINT('Ctrl Pts',(0.234812759114929,1.82331608910266,1.66667475728155));
#36304=CARTESIAN_POINT('Ctrl Pts',(-1.24220109658982,1.24943524423025,1.76680164648161));
#36305=CARTESIAN_POINT('Ctrl Pts',(-1.55154880719052,0.362871523529771,
1.8298913188532));
#36306=CARTESIAN_POINT('Ctrl Pts',(-1.55454118234884,-0.00133834695600729,
1.8559437743963));
#36307=CARTESIAN_POINT('Ctrl Pts',(-1.55460191805193,-0.00135568056800364,
1.2940562256037));
#36308=CARTESIAN_POINT('Ctrl Pts',(-1.5558637635503,-0.152693971168416,
1.30488274885721));
#36309=CARTESIAN_POINT('Ctrl Pts',(-1.46605510259419,-0.820638709603335,
1.35277141205443));
#36310=CARTESIAN_POINT('Ctrl Pts',(-0.510374815939226,-1.76654153931159,
1.43772221519537));
#36311=CARTESIAN_POINT('Ctrl Pts',(1.20797626960931,-1.38634273102519,1.54890863502654));
#36312=CARTESIAN_POINT('Ctrl Pts',(1.81976886629041,0.263806680570579,1.6600950548577));
#36313=CARTESIAN_POINT('Ctrl Pts',(0.764574137846417,1.67229745635935,1.77128147468886));
#36314=CARTESIAN_POINT('Ctrl Pts',(-0.991003621173195,1.54889135395602,
1.88246789452002));
#36315=CARTESIAN_POINT('Ctrl Pts',(-1.5572087700955,0.518861158146894,1.95672614482497));
#36316=CARTESIAN_POINT('Ctrl Pts',(-1.55805528871865,0.00189682319971778,
1.9939222551862));
#36317=CARTESIAN_POINT('Ctrl Pts',(-1.55805467550008,3.48541917938314E-5,
1.9940562256037));
#36318=CARTESIAN_POINT('Origin',(0.,0.,-1.29405622560369));
#36319=CARTESIAN_POINT('',(-1.55735926886437,0.00101346774827271,0.455943774396301));
#36320=CARTESIAN_POINT('',(-1.55326046963413,0.000729270061605516,0.594056225603705));
#36321=CARTESIAN_POINT('',(-1.5555,-2.01987159101623E-13,-1.29405622560369));
#36322=CARTESIAN_POINT('Ctrl Pts',(-1.55735926886437,0.00101346774827265,
0.455943774396301));
#36323=CARTESIAN_POINT('Ctrl Pts',(-1.5541538777776,-0.460983628495037,
0.489148600406595));
#36324=CARTESIAN_POINT('Ctrl Pts',(-1.09151218308356,-1.44423481489054,
0.559390643245367));
#36325=CARTESIAN_POINT('Ctrl Pts',(0.579488995883613,-1.74456230311225,
0.666669902912619));
#36326=CARTESIAN_POINT('Ctrl Pts',(1.77994191588978,-0.459827600750814,
0.777781553398056));
#36327=CARTESIAN_POINT('Ctrl Pts',(1.35192905881154,1.24578720765632,0.888893203883492));
#36328=CARTESIAN_POINT('Ctrl Pts',(-0.313001003158473,1.81151906168851,
1.00000485436893));
#36329=CARTESIAN_POINT('Ctrl Pts',(-1.41742497137191,0.93698092273704,1.08902171120653));
#36330=CARTESIAN_POINT('Ctrl Pts',(-1.55428446607623,0.210081433596544,
1.14100135121566));
#36331=CARTESIAN_POINT('Ctrl Pts',(-1.55333634177863,0.000779921548230561,
1.1559437743963));
#36332=CARTESIAN_POINT('Ctrl Pts',(-1.55326046963413,0.000729270061605551,
0.594056225603705));
#36333=CARTESIAN_POINT('Ctrl Pts',(-1.55199262831984,-0.304485333833814,
0.615843242528215));
#36334=CARTESIAN_POINT('Ctrl Pts',(-1.31743653601245,-1.13071739766558,
0.674692399396446));
#36335=CARTESIAN_POINT('Ctrl Pts',(0.0255447675030308,-1.83860034663711,
0.770603696208398));
#36336=CARTESIAN_POINT('Ctrl Pts',(1.55899683301632,-0.975032021788082,
0.881790116039561));
#36337=CARTESIAN_POINT('Ctrl Pts',(1.66434877052597,0.781732535368643,0.992976535870723));
#36338=CARTESIAN_POINT('Ctrl Pts',(0.245080507541896,1.82238325373942,1.10416295570189));
#36339=CARTESIAN_POINT('Ctrl Pts',(-1.23863138927055,1.25487925833816,1.20452285227955));
#36340=CARTESIAN_POINT('Ctrl Pts',(-1.55154412248428,0.365378245899198,
1.26782060891349));
#36341=CARTESIAN_POINT('Ctrl Pts',(-1.55460191805193,-0.00135568056800364,
1.2940562256037));
#36342=CARTESIAN_POINT('Origin',(0.,0.,11.5));
#36343=CARTESIAN_POINT('',(-1.77892626630995,-0.0012009523392913,11.2223275485995));
#36344=CARTESIAN_POINT('Ctrl Pts',(1.55548765964692,0.00619602180104861,
11.4445));
#36345=CARTESIAN_POINT('Ctrl Pts',(1.55843889773201,-0.053546881811892,
11.4417867591843));
#36346=CARTESIAN_POINT('Ctrl Pts',(1.55766805736304,-0.113278156040886,
11.439086160746));
#36347=CARTESIAN_POINT('Ctrl Pts',(1.55338999746751,-0.172741258360748,
11.4363936568093));
#36348=CARTESIAN_POINT('Ctrl Pts',(1.54917978268939,-0.231261344159722,
11.4337438528932));
#36349=CARTESIAN_POINT('Ctrl Pts',(1.54157226362346,-0.289522447371128,
11.4311018887755));
#36350=CARTESIAN_POINT('Ctrl Pts',(1.5307259163647,-0.347284232316321,11.4284634295395));
#36351=CARTESIAN_POINT('Ctrl Pts',(1.52490021612,-0.37830876404678,11.427046282158));
#36352=CARTESIAN_POINT('Ctrl Pts',(1.51813939227042,-0.409189253639797,
11.4256301458963));
#36353=CARTESIAN_POINT('Ctrl Pts',(1.51046300038634,-0.439887833717896,
11.4242143490555));
#36354=CARTESIAN_POINT('Ctrl Pts',(1.50749771858011,-0.451746261786366,
11.4236674467248));
#36355=CARTESIAN_POINT('Ctrl Pts',(1.50439653465153,-0.463574222421597,
11.4231207471528));
#36356=CARTESIAN_POINT('Ctrl Pts',(1.50116353235453,-0.47535996619676,11.4225746575513));
#36357=CARTESIAN_POINT('Ctrl Pts',(1.48455611813741,-0.535901441503565,
11.4197694828629));
#36358=CARTESIAN_POINT('Ctrl Pts',(1.46445634965142,-0.595403551134085,
11.4169769764437));
#36359=CARTESIAN_POINT('Ctrl Pts',(1.4410621824655,-0.653580209875647,11.414192092755));
#36360=CARTESIAN_POINT('Ctrl Pts',(1.41747802435967,-0.712229338392404,
11.4113845922059));
#36361=CARTESIAN_POINT('Ctrl Pts',(1.39054537943373,-0.769532412755046,
11.4085848387028));
#36362=CARTESIAN_POINT('Ctrl Pts',(1.36041578548535,-0.825184282227088,
11.4057876627772));
#36363=CARTESIAN_POINT('Ctrl Pts',(1.35261592294621,-0.839591277975912,
11.4050635379265));
#36364=CARTESIAN_POINT('Ctrl Pts',(1.34460155997405,-0.853887506909652,
11.4043395858183));
#36365=CARTESIAN_POINT('Ctrl Pts',(1.33637481784576,-0.868067413704247,
11.4036157167661));
#36366=CARTESIAN_POINT('Ctrl Pts',(1.33123141939554,-0.87693275912219,11.4031631503791));
#36367=CARTESIAN_POINT('Ctrl Pts',(1.32600576325494,-0.885751206456736,
11.4027106878625));
#36368=CARTESIAN_POINT('Ctrl Pts',(1.32070341258855,-0.894513477947337,
11.4022587210796));
#36369=CARTESIAN_POINT('Ctrl Pts',(1.28755838481391,-0.949286492822766,
11.3994334738427));
#36370=CARTESIAN_POINT('Ctrl Pts',(1.25136992677528,-1.00195372283142,11.3966231054397));
#36371=CARTESIAN_POINT('Ctrl Pts',(1.21232687524415,-1.05222079285711,11.3938225048748));
#36372=CARTESIAN_POINT('Ctrl Pts',(1.17352218779371,-1.10218097437215,11.3910390024248));
#36373=CARTESIAN_POINT('Ctrl Pts',(1.13189715922074,-1.14977118940024,11.3882651489085));
#36374=CARTESIAN_POINT('Ctrl Pts',(1.08759128036108,-1.19468014867466,11.3854959263702));
#36375=CARTESIAN_POINT('Ctrl Pts',(1.05692354853581,-1.22576532190738,11.3835791203762));
#36376=CARTESIAN_POINT('Ctrl Pts',(1.0249704261144,-1.25556541150052,11.3816645331574));
#36377=CARTESIAN_POINT('Ctrl Pts',(0.991767007145199,-1.28396712328559,
11.379750500582));
#36378=CARTESIAN_POINT('Ctrl Pts',(0.971829282858114,-1.30102155672743,
11.378601177562));
#36379=CARTESIAN_POINT('Ctrl Pts',(0.951440575196337,-1.31757160665078,
11.3774520545279));
#36380=CARTESIAN_POINT('Ctrl Pts',(0.930607078503626,-1.33359088746794,
11.3763027711782));
#36381=CARTESIAN_POINT('Ctrl Pts',(0.921822018225176,-1.34034589118487,
11.3758181418501));
#36382=CARTESIAN_POINT('Ctrl Pts',(0.912957575551233,-1.34700657088378,
11.3753334724466));
#36383=CARTESIAN_POINT('Ctrl Pts',(0.904026617991894,-1.35356212132308,
11.3748494000991));
#36384=CARTESIAN_POINT('Ctrl Pts',(0.898865665597572,-1.35735039189889,
11.3745696681303));
#36385=CARTESIAN_POINT('Ctrl Pts',(0.893681522170691,-1.36110432047063,
11.3742900812105));
#36386=CARTESIAN_POINT('Ctrl Pts',(0.888474357058895,-1.36482361432558,
11.3740106343829));
#36387=CARTESIAN_POINT('Ctrl Pts',(0.838811308516624,-1.4002961732508,11.3713454257582));
#36388=CARTESIAN_POINT('Ctrl Pts',(0.787057395286918,-1.43262124116857,
11.368692960317));
#36389=CARTESIAN_POINT('Ctrl Pts',(0.733560484100527,-1.46184200007972,
11.3660489378073));
#36390=CARTESIAN_POINT('Ctrl Pts',(0.677705393253366,-1.49235082960671,
11.3632883650152));
#36391=CARTESIAN_POINT('Ctrl Pts',(0.619949541746925,-1.51947609806138,
11.3605369959002));
#36392=CARTESIAN_POINT('Ctrl Pts',(0.560651932851881,-1.54322365588157,
11.3577899361005));
#36393=CARTESIAN_POINT('Ctrl Pts',(0.511114145446654,-1.56306259192994,
11.3554950161722));
#36394=CARTESIAN_POINT('Ctrl Pts',(0.460499386969577,-1.58054347420583,
11.3532031037542));
#36395=CARTESIAN_POINT('Ctrl Pts',(0.409004561176526,-1.5956447160272,11.3509113452381));
#36396=CARTESIAN_POINT('Ctrl Pts',(0.394571471762801,-1.59987732717035,
11.3502690058367));
#36397=CARTESIAN_POINT('Ctrl Pts',(0.38006920116156,-1.60392285642947,11.3496266785255));
#36398=CARTESIAN_POINT('Ctrl Pts',(0.365502000908426,-1.60778049339754,
11.3489843004725));
#36399=CARTESIAN_POINT('Ctrl Pts',(0.352945849497182,-1.61110557117631,
11.3484306047756));
#36400=CARTESIAN_POINT('Ctrl Pts',(0.340339686983491,-1.61429135213649,
11.3478767954507));
#36401=CARTESIAN_POINT('Ctrl Pts',(0.327707338901135,-1.61733252206154,
11.3473237518226));
#36402=CARTESIAN_POINT('Ctrl Pts',(0.26442068399392,-1.63256844418037,11.3445530649309));
#36403=CARTESIAN_POINT('Ctrl Pts',(0.200363163100888,-1.64421053384351,
11.3417964693365));
#36404=CARTESIAN_POINT('Ctrl Pts',(0.135902532141567,-1.65227549235515,
11.3390491503551));
#36405=CARTESIAN_POINT('Ctrl Pts',(0.0706504004584388,-1.66043947907059,
11.3362680975283));
#36406=CARTESIAN_POINT('Ctrl Pts',(0.00498413291330568,-1.6649382180869,
11.333496550525));
#36407=CARTESIAN_POINT('Ctrl Pts',(-0.0607337043444866,-1.66573959706564,
11.3307295151184));
#36408=CARTESIAN_POINT('Ctrl Pts',(-0.114943810254912,-1.66640064802417,
11.3284470102656));
#36409=CARTESIAN_POINT('Ctrl Pts',(-0.169189647051337,-1.66454499730668,
11.326167575313));
#36410=CARTESIAN_POINT('Ctrl Pts',(-0.223269283792523,-1.66012780789457,
11.3238884070273));
#36411=CARTESIAN_POINT('Ctrl Pts',(-0.242921115785065,-1.65852265909112,
11.3230601871106));
#36412=CARTESIAN_POINT('Ctrl Pts',(-0.262550978640708,-1.65657902103982,
11.3222320024074));
#36413=CARTESIAN_POINT('Ctrl Pts',(-0.282149042864747,-1.65429391513469,
11.3214037184036));
#36414=CARTESIAN_POINT('Ctrl Pts',(-0.293822649715497,-1.65293278948249,
11.3209103501959));
#36415=CARTESIAN_POINT('Ctrl Pts',(-0.305486007024825,-1.65145026241138,
11.3204169024293));
#36416=CARTESIAN_POINT('Ctrl Pts',(-0.317120120921591,-1.64984824722041,
11.3199240638241));
#36417=CARTESIAN_POINT('Ctrl Pts',(-0.382649500838262,-1.64082486451904,
11.3171481404934));
#36418=CARTESIAN_POINT('Ctrl Pts',(-0.447374851901241,-1.62800143931766,
11.3143862955204));
#36419=CARTESIAN_POINT('Ctrl Pts',(-0.510936115769287,-1.6113566500933,
11.3116336908415));
#36420=CARTESIAN_POINT('Ctrl Pts',(-0.573549739883189,-1.59496001930709,
11.3089221249567));
#36421=CARTESIAN_POINT('Ctrl Pts',(-0.635034780101342,-1.57485515271455,
11.3062195258916));
#36422=CARTESIAN_POINT('Ctrl Pts',(-0.695044280650932,-1.55097228857054,
11.3035212687658));
#36423=CARTESIAN_POINT('Ctrl Pts',(-0.755213263935446,-1.52702595273528,
11.3008158406849));
#36424=CARTESIAN_POINT('Ctrl Pts',(-0.813899721511821,-1.49928127162975,
11.2981147776525));
#36425=CARTESIAN_POINT('Ctrl Pts',(-0.870916818143125,-1.46801413582731,
11.2954134178164));
#36426=CARTESIAN_POINT('Ctrl Pts',(-0.88517189274549,-1.46019691292752,
11.2947380399339));
#36427=CARTESIAN_POINT('Ctrl Pts',(-0.8993225020166,-1.4521592870016,11.294062643499));
#36428=CARTESIAN_POINT('Ctrl Pts',(-0.913365468395192,-1.44390514150358,
11.2933871556582));
#36429=CARTESIAN_POINT('Ctrl Pts',(-0.922789553247202,-1.43836587255875,
11.2929338429778));
#36430=CARTESIAN_POINT('Ctrl Pts',(-0.932156968408698,-1.43273389293101,
11.2924808828034));
#36431=CARTESIAN_POINT('Ctrl Pts',(-0.941465939330546,-1.42701150822941,
11.2920283046203));
#36432=CARTESIAN_POINT('Ctrl Pts',(-0.997258564244995,-1.39271482109252,
11.2893158109378));
#36433=CARTESIAN_POINT('Ctrl Pts',(-1.05096555773083,-1.35516769400791,
11.2866164406656));
#36434=CARTESIAN_POINT('Ctrl Pts',(-1.10242222381511,-1.31470157532149,
11.2839256753843));
#36435=CARTESIAN_POINT('Ctrl Pts',(-1.15490559840975,-1.27342804116106,
11.2811812215953));
#36436=CARTESIAN_POINT('Ctrl Pts',(-1.20504870548191,-1.22911724367845,
11.2784457196118));
#36437=CARTESIAN_POINT('Ctrl Pts',(-1.25265335579406,-1.18207076364008,
11.2757143751156));
#36438=CARTESIAN_POINT('Ctrl Pts',(-1.28397500867159,-1.15111636092502,
11.2739172770666));
#36439=CARTESIAN_POINT('Ctrl Pts',(-1.31419725536704,-1.11897666094205,
11.2721219788063));
#36440=CARTESIAN_POINT('Ctrl Pts',(-1.34325581778868,-1.08572815742637,
11.2703271147686));
#36441=CARTESIAN_POINT('Ctrl Pts',(-1.36209363901681,-1.06417411919684,
11.2691635565932));
#36442=CARTESIAN_POINT('Ctrl Pts',(-1.38044228251278,-1.04215395727969,
11.2680001809021));
#36443=CARTESIAN_POINT('Ctrl Pts',(-1.39828252264694,-1.01968718394611,
11.2668366156616));
#36444=CARTESIAN_POINT('Ctrl Pts',(-1.40805056143521,-1.00738598666853,
11.2661995306046));
#36445=CARTESIAN_POINT('Ctrl Pts',(-1.41766921695113,-0.994946604236495,
11.2655621759649));
#36446=CARTESIAN_POINT('Ctrl Pts',(-1.42711662985222,-0.982397385607975,
11.264925758661));
#36447=CARTESIAN_POINT('Ctrl Pts',(-1.46820629310292,-0.927817028752221,
11.262157786839));
#36448=CARTESIAN_POINT('Ctrl Pts',(-1.50612185513061,-0.871087521735772,
11.2594035844773));
#36449=CARTESIAN_POINT('Ctrl Pts',(-1.54066769776793,-0.812525394359864,
11.2566583590267));
#36450=CARTESIAN_POINT('Ctrl Pts',(-1.57505516312501,-0.754231748217875,
11.2539257192103));
#36451=CARTESIAN_POINT('Ctrl Pts',(-1.60610442219133,-0.694121381542228,
11.2512019741836));
#36452=CARTESIAN_POINT('Ctrl Pts',(-1.63358497140864,-0.632471603998023,
11.2484823970106));
#36453=CARTESIAN_POINT('Ctrl Pts',(-1.65966108961598,-0.573972522557314,
11.2459018075444));
#36454=CARTESIAN_POINT('Ctrl Pts',(-1.68252420078453,-0.514086499095208,
11.2433249708101));
#36455=CARTESIAN_POINT('Ctrl Pts',(-1.70193725006908,-0.453031690747441,
11.2407478481942));
#36456=CARTESIAN_POINT('Ctrl Pts',(-1.70639988231082,-0.438996535720931,
11.2401554244947));
#36457=CARTESIAN_POINT('Ctrl Pts',(-1.71068001578898,-0.424899564800969,
11.239562985688));
#36458=CARTESIAN_POINT('Ctrl Pts',(-1.71477442803653,-0.410743347710776,
11.2389704827146));
#36459=CARTESIAN_POINT('Ctrl Pts',(-1.7181060933816,-0.399224288308597,
11.238488356953));
#36460=CARTESIAN_POINT('Ctrl Pts',(-1.72131496051192,-0.387664952239154,
11.2380061462914));
#36461=CARTESIAN_POINT('Ctrl Pts',(-1.72439513423882,-0.376083269559728,
11.2375245092466));
#36462=CARTESIAN_POINT('Ctrl Pts',(-1.73399637264737,-0.339981897872015,
11.2360231938976));
#36463=CARTESIAN_POINT('Ctrl Pts',(-1.74235845090443,-0.303626928305512,
11.234525913273));
#36464=CARTESIAN_POINT('Ctrl Pts',(-1.74944665354966,-0.267065873422436,
11.2330319031487));
#36465=CARTESIAN_POINT('Ctrl Pts',(-1.76197449586933,-0.202447076028902,
11.2303913574139));
#36466=CARTESIAN_POINT('Ctrl Pts',(-1.77052625497235,-0.137185361680741,
11.227761027999));
#36467=CARTESIAN_POINT('Ctrl Pts',(-1.77528061829343,-0.0715870718432795,
11.2251366955952));
#36468=CARTESIAN_POINT('Ctrl Pts',(-1.77697828156189,-0.0481635764959884,
11.2241996126621));
#36469=CARTESIAN_POINT('Ctrl Pts',(-1.7781912975682,-0.0246970169190114,
11.2232632943623));
#36470=CARTESIAN_POINT('Ctrl Pts',(-1.77892626630995,-0.00120095233929127,
11.2223275485995));
#36471=CARTESIAN_POINT('',(1.88128289424299,-0.51655738433239,11.046));
#36472=CARTESIAN_POINT('Ctrl Pts',(1.88079991776263,-0.516378774142054,
11.046));
#36473=CARTESIAN_POINT('Ctrl Pts',(1.89035995045861,-0.445151004206684,
11.0555631104642));
#36474=CARTESIAN_POINT('Ctrl Pts',(1.8961423315859,-0.373654493774377,11.0651669654983));
#36475=CARTESIAN_POINT('Ctrl Pts',(1.89809144951916,-0.302224012343752,
11.0748303404806));
#36476=CARTESIAN_POINT('Ctrl Pts',(1.89999077178002,-0.23261842246626,11.0842468375051));
#36477=CARTESIAN_POINT('Ctrl Pts',(1.89824990827702,-0.163074621232238,
11.0937198521185));
#36478=CARTESIAN_POINT('Ctrl Pts',(1.89277099599951,-0.0939167257851171,
11.1032667571406));
#36479=CARTESIAN_POINT('Ctrl Pts',(1.88910201129244,-0.0476047485319078,
11.1096598962807));
#36480=CARTESIAN_POINT('Ctrl Pts',(1.8837557967888,-0.00146614169388357,
11.1160861707414));
#36481=CARTESIAN_POINT('Ctrl Pts',(1.87669176161129,0.0443950771863014,
11.1225507975725));
#36482=CARTESIAN_POINT('Ctrl Pts',(1.87063241478827,0.0837336455737761,
11.1280959874063));
#36483=CARTESIAN_POINT('Ctrl Pts',(1.8633089856103,0.122868068816038,11.1336693960131));
#36484=CARTESIAN_POINT('Ctrl Pts',(1.85469071090361,0.161728394728602,11.1392743160301));
#36485=CARTESIAN_POINT('Ctrl Pts',(1.85223436103037,0.172804226014781,11.1408718103131));
#36486=CARTESIAN_POINT('Ctrl Pts',(1.84967323324123,0.183855475695868,11.142471538338));
#36487=CARTESIAN_POINT('Ctrl Pts',(1.84700939076218,0.19487013146115,11.1440720571876));
#36488=CARTESIAN_POINT('Ctrl Pts',(1.83137216521354,0.259528105007685,11.1534673853433));
#36489=CARTESIAN_POINT('Ctrl Pts',(1.81217652429567,0.323030635926077,11.1629048835303));
#36490=CARTESIAN_POINT('Ctrl Pts',(1.78934255453511,0.385087390709459,11.1724028038701));
#36491=CARTESIAN_POINT('Ctrl Pts',(1.78198218565347,0.405090947322401,11.1754643914102));
#36492=CARTESIAN_POINT('Ctrl Pts',(1.77424343060636,0.424944079046285,11.1785322571122));
#36493=CARTESIAN_POINT('Ctrl Pts',(1.76612263817241,0.444636415640588,11.181607012295));
#36494=CARTESIAN_POINT('Ctrl Pts',(1.73919119835162,0.509943216945239,11.1918039955137));
#36495=CARTESIAN_POINT('Ctrl Pts',(1.70806080167302,0.573485248201441,11.2020767507448));
#36496=CARTESIAN_POINT('Ctrl Pts',(1.67301702698032,0.634984575310704,11.2124475752393));
#36497=CARTESIAN_POINT('Ctrl Pts',(1.64235372412421,0.688796486531309,11.2215220466721));
#36498=CARTESIAN_POINT('Ctrl Pts',(1.60869302252863,0.741044106677185,11.2306716023846));
#36499=CARTESIAN_POINT('Ctrl Pts',(1.57220891785208,0.791506873950779,11.239911179793));
#36500=CARTESIAN_POINT('Ctrl Pts',(1.56528521292053,0.801083354276364,11.2416646038728));
#36501=CARTESIAN_POINT('Ctrl Pts',(1.55825911602623,0.81059620160376,11.2434214216921));
#36502=CARTESIAN_POINT('Ctrl Pts',(1.55114206425445,0.820030590825838,11.2451792455347));
#36503=CARTESIAN_POINT('Ctrl Pts',(1.51163333781795,0.872403499555923,11.254937412757));
#36504=CARTESIAN_POINT('Ctrl Pts',(1.46925448012712,0.922460374176763,11.2647444648472));
#36505=CARTESIAN_POINT('Ctrl Pts',(1.42425895086728,0.969999034377404,11.2746213834588));
#36506=CARTESIAN_POINT('Ctrl Pts',(1.37955552976012,1.01722907657888,11.2844341817346));
#36507=CARTESIAN_POINT('Ctrl Pts',(1.33226826113497,1.06197396880102,11.2943159423384));
#36508=CARTESIAN_POINT('Ctrl Pts',(1.28262305484525,1.10398985376236,11.3042872409362));
#36509=CARTESIAN_POINT('Ctrl Pts',(1.23402945162958,1.14511574274852,11.3140473238087));
#36510=CARTESIAN_POINT('Ctrl Pts',(1.18317581682196,1.18362727550242,11.3238931915966));
#36511=CARTESIAN_POINT('Ctrl Pts',(1.13026675802768,1.2192467284131,11.3338441399431));
#36512=CARTESIAN_POINT('Ctrl Pts',(1.11612186853279,1.22876935528969,11.3365044606506));
#36513=CARTESIAN_POINT('Ctrl Pts',(1.1018300740637,1.23808499004259,11.3391722917297));
#36514=CARTESIAN_POINT('Ctrl Pts',(1.0873953214649,1.24718768011963,11.3418480018757));
#36515=CARTESIAN_POINT('Ctrl Pts',(1.07843141524914,1.25284040326838,11.3435096039465));
#36516=CARTESIAN_POINT('Ctrl Pts',(1.06941317684967,1.25841040829158,11.3451740914355));
#36517=CARTESIAN_POINT('Ctrl Pts',(1.06035226952456,1.2638900735973,11.346839603865));
#36518=CARTESIAN_POINT('Ctrl Pts',(1.00742079701965,1.29590085828569,11.3565690958694));
#36519=CARTESIAN_POINT('Ctrl Pts',(0.952938092487177,1.32489391547385,11.3663514013733));
#36520=CARTESIAN_POINT('Ctrl Pts',(0.897108858642945,1.35066478023243,11.3762079140514));
#36521=CARTESIAN_POINT('Ctrl Pts',(0.842238965806958,1.37599281162795,11.3858950574554));
#36522=CARTESIAN_POINT('Ctrl Pts',(0.78606756226141,1.39820862213323,11.3956538796688));
#36523=CARTESIAN_POINT('Ctrl Pts',(0.72878604220227,1.41706842320411,11.4055046903548));
#36524=CARTESIAN_POINT('Ctrl Pts',(0.67317444208947,1.43537840719681,11.4150683217683));
#36525=CARTESIAN_POINT('Ctrl Pts',(0.616515828164059,1.45052520284418,11.4247186563809));
#36526=CARTESIAN_POINT('Ctrl Pts',(0.558993687390787,1.46223733220615,11.4344742788813));
#36527=CARTESIAN_POINT('Ctrl Pts',(0.539362537898783,1.46623444634835,11.4378036765901));
#36528=CARTESIAN_POINT('Ctrl Pts',(0.519630929867265,1.46983109384517,11.4411453373854));
#36529=CARTESIAN_POINT('Ctrl Pts',(0.499806597877626,1.47301514408983,11.4445));
#36530=CARTESIAN_POINT('',(1.56060797133591,1.17265290216009,11.046));
#36531=CARTESIAN_POINT('Origin',(0.,0.,11.046));
#36532=CARTESIAN_POINT('Ctrl Pts',(-1.77892626630995,-0.00120095233929127,
11.2223275485995));
#36533=CARTESIAN_POINT('Ctrl Pts',(-1.78091222637221,0.0622877965358305,
11.2197990686688));
#36534=CARTESIAN_POINT('Ctrl Pts',(-1.77941067542291,0.125992016111799,
11.2172747683064));
#36535=CARTESIAN_POINT('Ctrl Pts',(-1.77452381634337,0.189646102027163,
11.2147508586347));
#36536=CARTESIAN_POINT('Ctrl Pts',(-1.77287868795546,0.211074823838332,
11.2139012013432));
#36537=CARTESIAN_POINT('Ctrl Pts',(-1.7708495726434,0.232497857027148,11.2130515883281));
#36538=CARTESIAN_POINT('Ctrl Pts',(-1.76843936997923,0.253904972833394,
11.2122018750387));
#36539=CARTESIAN_POINT('Ctrl Pts',(-1.76712267121633,0.265599725029338,
11.2117376748892));
#36540=CARTESIAN_POINT('Ctrl Pts',(-1.76569197102713,0.277291668505868,
11.2112733675823));
#36541=CARTESIAN_POINT('Ctrl Pts',(-1.7641484990815,0.288972974548762,11.2108091738099));
#36542=CARTESIAN_POINT('Ctrl Pts',(-1.75515036560026,0.357072658062498,
11.2081030167356));
#36543=CARTESIAN_POINT('Ctrl Pts',(-1.74235696629666,0.42456963250346,11.2054102736121));
#36544=CARTESIAN_POINT('Ctrl Pts',(-1.72594903242932,0.491138664005795,
11.2027264834948));
#36545=CARTESIAN_POINT('Ctrl Pts',(-1.70928395222888,0.558750970212142,
11.2000006328234));
#36546=CARTESIAN_POINT('Ctrl Pts',(-1.68888999030711,0.625407040269523,
11.1972840179815));
#36547=CARTESIAN_POINT('Ctrl Pts',(-1.66490278446929,0.690766734877331,
11.1945719649831));
#36548=CARTESIAN_POINT('Ctrl Pts',(-1.64112198461878,0.755564019991226,
11.1918832487577));
#36549=CARTESIAN_POINT('Ctrl Pts',(-1.61380916520598,0.81908815011939,11.1891990162058));
#36550=CARTESIAN_POINT('Ctrl Pts',(-1.5830482712126,0.880993120829078,11.186514712963));
#36551=CARTESIAN_POINT('Ctrl Pts',(-1.57216641681974,0.902892382846704,
11.1855651242728));
#36552=CARTESIAN_POINT('Ctrl Pts',(-1.56085264019442,0.92458881232314,11.1846155267362));
#36553=CARTESIAN_POINT('Ctrl Pts',(-1.54910931637308,0.946066284278751,
11.1836657187303));
#36554=CARTESIAN_POINT('Ctrl Pts',(-1.54396572241992,0.955473450134084,
11.1832497013582));
#36555=CARTESIAN_POINT('Ctrl Pts',(-1.53874121405367,0.964835754579395,
11.1828337685169));
#36556=CARTESIAN_POINT('Ctrl Pts',(-1.5334404792476,0.974144495398925,11.18241823656));
#36557=CARTESIAN_POINT('Ctrl Pts',(-1.49854818334159,1.03541964895223,11.179682981066));
#36558=CARTESIAN_POINT('Ctrl Pts',(-1.46030493742689,1.09447092650475,11.1769608571821));
#36559=CARTESIAN_POINT('Ctrl Pts',(-1.41884997832206,1.15095727599886,11.1742472453603));
#36560=CARTESIAN_POINT('Ctrl Pts',(-1.37811238995456,1.20646613920276,11.1715805921112));
#36561=CARTESIAN_POINT('Ctrl Pts',(-1.33427285188376,1.25949901944966,11.1689221588738));
#36562=CARTESIAN_POINT('Ctrl Pts',(-1.28741864153,1.30971119589593,11.166267561795));
#36563=CARTESIAN_POINT('Ctrl Pts',(-1.26549062822221,1.33321075474058,11.1650251966024));
#36564=CARTESIAN_POINT('Ctrl Pts',(-1.24290170835111,1.35609210845284,11.1637836716393));
#36565=CARTESIAN_POINT('Ctrl Pts',(-1.21965775424868,1.37831740927343,11.1625425375316));
#36566=CARTESIAN_POINT('Ctrl Pts',(-1.19165584264812,1.40509215276722,11.1610473475387));
#36567=CARTESIAN_POINT('Ctrl Pts',(-1.16270333140537,1.43091488294274,11.1595527247918));
#36568=CARTESIAN_POINT('Ctrl Pts',(-1.13285929301872,1.45577404177113,11.1580578836196));
#36569=CARTESIAN_POINT('Ctrl Pts',(-1.12175109882477,1.46502682318719,11.1575014915585));
#36570=CARTESIAN_POINT('Ctrl Pts',(-1.11051936159011,1.47414607111053,11.156945069237));
#36571=CARTESIAN_POINT('Ctrl Pts',(-1.09916702235175,1.48313103947397,11.1563885761416));
#36572=CARTESIAN_POINT('Ctrl Pts',(-1.0900493418525,1.49034735578674,11.1559416262983));
#36573=CARTESIAN_POINT('Ctrl Pts',(-1.08085382696811,1.49747696130526,11.1554946319594));
#36574=CARTESIAN_POINT('Ctrl Pts',(-1.07159363370462,1.50451093778695,11.1550481251347));
#36575=CARTESIAN_POINT('Ctrl Pts',(-1.01611106549685,1.54665509923293,11.152372873695));
#36576=CARTESIAN_POINT('Ctrl Pts',(-0.958209601759993,1.58545013781557,
11.1497101571816));
#36577=CARTESIAN_POINT('Ctrl Pts',(-0.898278760372612,1.62088563165273,
11.1470556568828));
#36578=CARTESIAN_POINT('Ctrl Pts',(-0.837571419107242,1.65678024897295,
11.1443667632881));
#36579=CARTESIAN_POINT('Ctrl Pts',(-0.774780874239298,1.6892280755481,11.1416863001956));
#36580=CARTESIAN_POINT('Ctrl Pts',(-0.71027313016202,1.71817742298682,11.1390097788418));
#36581=CARTESIAN_POINT('Ctrl Pts',(-0.66261429365752,1.73956543207362,11.13703234349));
#36582=CARTESIAN_POINT('Ctrl Pts',(-0.614017264977652,1.75904301818697,
11.135057059686));
#36583=CARTESIAN_POINT('Ctrl Pts',(-0.56462073685077,1.77657345707156,11.1330821172509));
#36584=CARTESIAN_POINT('Ctrl Pts',(-0.539231747042784,1.78558380964183,
11.1320670298498));
#36585=CARTESIAN_POINT('Ctrl Pts',(-0.513631449727103,1.79407954038564,
11.1310520326313));
#36586=CARTESIAN_POINT('Ctrl Pts',(-0.487838223654543,1.802054170041,11.1300368798027));
#36587=CARTESIAN_POINT('Ctrl Pts',(-0.475799003301229,1.80577640018727,
11.1295630480858));
#36588=CARTESIAN_POINT('Ctrl Pts',(-0.463717747565173,1.80938508638487,
11.129089182467));
#36589=CARTESIAN_POINT('Ctrl Pts',(-0.451596312388482,1.81287949077367,
11.1286152579519));
#36590=CARTESIAN_POINT('Ctrl Pts',(-0.439480899976025,1.81637215890158,
11.1281415689151));
#36591=CARTESIAN_POINT('Ctrl Pts',(-0.427332434103985,1.81974856717366,
11.1276680985874));
#36592=CARTESIAN_POINT('Ctrl Pts',(-0.415160020480683,1.8230065701324,11.1271950974533));
#36593=CARTESIAN_POINT('Ctrl Pts',(-0.345659931193023,1.8416085913534,11.1244944316633));
#36594=CARTESIAN_POINT('Ctrl Pts',(-0.275309825422015,1.85637496302517,
11.1218062647546));
#36595=CARTESIAN_POINT('Ctrl Pts',(-0.204481476884407,1.86725830113956,
11.1191261497819));
#36596=CARTESIAN_POINT('Ctrl Pts',(-0.133579826115251,1.87815290272383,
11.1164432610836));
#36597=CARTESIAN_POINT('Ctrl Pts',(-0.0621979169225611,1.88515673586772,
11.1137684409964));
#36598=CARTESIAN_POINT('Ctrl Pts',(0.00930939936232982,1.88817434312463,
11.111097228754));
#36599=CARTESIAN_POINT('Ctrl Pts',(0.0795378313902503,1.89113798149254,
11.1084737902425));
#36600=CARTESIAN_POINT('Ctrl Pts',(0.149888204683991,1.89025686041538,11.1058538316796));
#36601=CARTESIAN_POINT('Ctrl Pts',(0.220026910137412,1.88539116319202,11.1032331273822));
#36602=CARTESIAN_POINT('Ctrl Pts',(0.236366392955163,1.88425765244837,11.1026226092302));
#36603=CARTESIAN_POINT('Ctrl Pts',(0.252694364144288,1.88290767750495,11.102012050607));
#36604=CARTESIAN_POINT('Ctrl Pts',(0.269006539233807,1.88133906123029,11.1014013980884));
#36605=CARTESIAN_POINT('Ctrl Pts',(0.280730896030037,1.88021162011471,11.1009624923038));
#36606=CARTESIAN_POINT('Ctrl Pts',(0.292446914187848,1.8789711508204,11.1005235443156));
#36607=CARTESIAN_POINT('Ctrl Pts',(0.304138944100939,1.87761870427971,11.1000850620809));
#36608=CARTESIAN_POINT('Ctrl Pts',(0.375822773838615,1.86932685519343,11.0973967277121));
#36609=CARTESIAN_POINT('Ctrl Pts',(0.446738242932316,1.85681796775178,11.0947208906731));
#36610=CARTESIAN_POINT('Ctrl Pts',(0.516529562716851,1.84000805096474,11.0920531719144));
#36611=CARTESIAN_POINT('Ctrl Pts',(0.584847521294231,1.82355300752536,11.0894417712386));
#36612=CARTESIAN_POINT('Ctrl Pts',(0.652089317501138,1.80297695165361,11.0868381496919));
#36613=CARTESIAN_POINT('Ctrl Pts',(0.718036401553849,1.77856692481578,11.084238199749));
#36614=CARTESIAN_POINT('Ctrl Pts',(0.785323202313169,1.75366100765569,11.0815854317561));
#36615=CARTESIAN_POINT('Ctrl Pts',(0.851262956271168,1.7247633139281,11.0789364860598));
#36616=CARTESIAN_POINT('Ctrl Pts',(0.915607648721953,1.6921267735849,11.0762869996812));
#36617=CARTESIAN_POINT('Ctrl Pts',(0.930631108062465,1.68450666199239,11.0756683868732));
#36618=CARTESIAN_POINT('Ctrl Pts',(0.945567515715628,1.67668252571399,11.0750497445899));
#36619=CARTESIAN_POINT('Ctrl Pts',(0.960413518624615,1.6686572293506,11.074431017298));
#36620=CARTESIAN_POINT('Ctrl Pts',(0.975205360081844,1.66066121101609,11.073814547258));
#36621=CARTESIAN_POINT('Ctrl Pts',(0.989912270604597,1.65246257743845,11.0731977870787));
#36622=CARTESIAN_POINT('Ctrl Pts',(1.00450295029956,1.6440805277344,11.0725818668126));
#36623=CARTESIAN_POINT('Ctrl Pts',(1.06739734574523,1.60794897253934,11.0699268888682));
#36624=CARTESIAN_POINT('Ctrl Pts',(1.12821828188749,1.56837054324493,11.0672840147147));
#36625=CARTESIAN_POINT('Ctrl Pts',(1.18673956352194,1.52565231730803,11.0646490274931));
#36626=CARTESIAN_POINT('Ctrl Pts',(1.24608357911593,1.48233352805146,11.0619769957398));
#36627=CARTESIAN_POINT('Ctrl Pts',(1.30306365724006,1.43578546725283,11.0593130742375));
#36628=CARTESIAN_POINT('Ctrl Pts',(1.35742307425591,1.38627866511896,11.056652865764));
#36629=CARTESIAN_POINT('Ctrl Pts',(1.41159294455999,1.3369444890372,11.0540019332135));
#36630=CARTESIAN_POINT('Ctrl Pts',(1.4631611896777,1.28467147000892,11.0513546878431));
#36631=CARTESIAN_POINT('Ctrl Pts',(1.51184108762766,1.22968809505141,11.0487067782687));
#36632=CARTESIAN_POINT('Ctrl Pts',(1.52842600119773,1.21095562929319,11.0478046532996));
#36633=CARTESIAN_POINT('Ctrl Pts',(1.54467532477781,1.19190827830405,11.0469024512351));
#36634=CARTESIAN_POINT('Ctrl Pts',(1.56057659382849,1.17255425406029,11.046));
#36635=CARTESIAN_POINT('',(-0.999999999999999,-1.22464679914735E-16,12.));
#36636=CARTESIAN_POINT('',(-1.5,-1.83697019872103E-16,11.5));
#36637=CARTESIAN_POINT('Origin',(0.,0.,12.));
#36638=CARTESIAN_POINT('Ctrl Pts',(1.13509973994371,-1.59049193030953,-0.230074082272069));
#36639=CARTESIAN_POINT('Ctrl Pts',(1.66385127640631,-1.21313337847033,-0.19303686544359));
#36640=CARTESIAN_POINT('Ctrl Pts',(2.30633516687349,0.103782615975306,-0.118962431786632));
#36641=CARTESIAN_POINT('Ctrl Pts',(1.16188988078006,1.99753850566951,-0.00785078130119459));
#36642=CARTESIAN_POINT('Ctrl Pts',(-1.04655428901899,2.05782953697956,0.103260869184242));
#36643=CARTESIAN_POINT('Ctrl Pts',(-2.29698075471667,0.238333788527267,
0.214372519669679));
#36644=CARTESIAN_POINT('Ctrl Pts',(-1.44613108848303,-1.80075271725216,
0.325484170155115));
#36645=CARTESIAN_POINT('Ctrl Pts',(0.727946961077783,-2.19149774367173,
0.436595820640553));
#36646=CARTESIAN_POINT('Ctrl Pts',(2.2359411788162,-0.57762978583554,0.547707471125989));
#36647=CARTESIAN_POINT('Ctrl Pts',(1.69827668332871,1.56494259322429,0.658819121611427));
#36648=CARTESIAN_POINT('Ctrl Pts',(-0.393188016825179,2.27560800163251,
0.769930772096863));
#36649=CARTESIAN_POINT('Ctrl Pts',(-2.12490816724285,0.90434536960108,0.881042422582301));
#36650=CARTESIAN_POINT('Ctrl Pts',(-1.9125222930514,-1.29434912039326,0.992154073067737));
#36651=CARTESIAN_POINT('Ctrl Pts',(0.0496630258143332,-2.30880650358359,
1.10326572355317));
#36652=CARTESIAN_POINT('Ctrl Pts',(1.96640931676781,-1.21090966106477,1.21437737403861));
#36653=CARTESIAN_POINT('Ctrl Pts',(2.08405785032279,0.994871990457256,1.32548902452405));
#36654=CARTESIAN_POINT('Ctrl Pts',(0.294968904732024,2.29042728261432,1.43660067500948));
#36655=CARTESIAN_POINT('Ctrl Pts',(-1.76399147035948,1.49043619583305,1.54771232549492));
#36656=CARTESIAN_POINT('Ctrl Pts',(-2.20904863824581,-0.673178902258552,
1.65882397598036));
#36657=CARTESIAN_POINT('Ctrl Pts',(-0.633012670336293,-2.22089176195486,
1.7699356264658));
#36658=CARTESIAN_POINT('Ctrl Pts',(1.52217643594786,-1.73667627565877,1.88104727695123));
#36659=CARTESIAN_POINT('Ctrl Pts',(2.28470258285089,0.336451535954383,1.99215892743667));
#36660=CARTESIAN_POINT('Ctrl Pts',(0.956918672404541,2.10175453516431,2.10327057792211));
#36661=CARTESIAN_POINT('Ctrl Pts',(-1.24636506047609,1.94412953698174,2.21438222840754));
#36662=CARTESIAN_POINT('Ctrl Pts',(-2.30932995110325,0.00779007092406014,
2.32549387889298));
#36663=CARTESIAN_POINT('Ctrl Pts',(-1.2594528285163,-1.93567664513544,2.43660552937842));
#36664=CARTESIAN_POINT('Ctrl Pts',(0.942717341349318,-2.1081625941051,2.54771717986386));
#36665=CARTESIAN_POINT('Ctrl Pts',(2.28238070382781,-0.351857683462,2.65882883034929));
#36666=CARTESIAN_POINT('Ctrl Pts',(1.53385834111148,1.72636731182735,2.76994048083473));
#36667=CARTESIAN_POINT('Ctrl Pts',(-0.618014955343493,2.22511191222357,
2.88105213132016));
#36668=CARTESIAN_POINT('Ctrl Pts',(-2.20445672440028,0.68806689849701,2.99216378180561));
#36669=CARTESIAN_POINT('Ctrl Pts',(-1.77400663329184,-1.47850125855229,
3.10327543229104));
#36670=CARTESIAN_POINT('Ctrl Pts',(0.279509811935462,-2.29236554058792,
3.21438708277648));
#36671=CARTESIAN_POINT('Ctrl Pts',(2.07729836817097,-1.00890881459812,3.32549873326191));
#36672=CARTESIAN_POINT('Ctrl Pts',(1.97453422882556,1.1976143309821,3.43661038374735));
#36673=CARTESIAN_POINT('Ctrl Pts',(0.0652379087403971,2.30842143506323,
3.54772203423278));
#36674=CARTESIAN_POINT('Ctrl Pts',(-1.90374559216213,1.30721774273047,3.65883368471823));
#36675=CARTESIAN_POINT('Ctrl Pts',(-2.13096254074055,-0.889979863001003,
3.76994533520366));
#36676=CARTESIAN_POINT('Ctrl Pts',(-0.408528604769679,-2.27292100295502,
3.8810569856891));
#36677=CARTESIAN_POINT('Ctrl Pts',(1.6876745272456,-1.57633124585981,3.99216863617453));
#36678=CARTESIAN_POINT('Ctrl Pts',(2.23979789625721,0.562468568463683,4.10328028665997));
#36679=CARTESIAN_POINT('Ctrl Pts',(0.742695215461042,2.18665711155622,4.21439193714541));
#36680=CARTESIAN_POINT('Ctrl Pts',(-1.43391090854028,1.81023893808443,4.32550358763085));
#36681=CARTESIAN_POINT('Ctrl Pts',(-2.29860956455329,-0.222395090620434,
4.43661523811628));
#36682=CARTESIAN_POINT('Ctrl Pts',(-1.06027445761331,-2.05155638019547,
4.54772688860172));
#36683=CARTESIAN_POINT('Ctrl Pts',(1.14812229735204,-2.00371672072451,4.65883853908716));
#36684=CARTESIAN_POINT('Ctrl Pts',(2.30608404475241,-0.122645363248325,
4.76995018957259));
#36685=CARTESIAN_POINT('Ctrl Pts',(1.35417351061808,1.87063615108022,4.88106184005803));
#36686=CARTESIAN_POINT('Ctrl Pts',(-0.83669150175529,2.1524434574405,4.99217349054346));
#36687=CARTESIAN_POINT('Ctrl Pts',(-2.26205440167697,0.464946653328952,
5.10328514102891));
#36688=CARTESIAN_POINT('Ctrl Pts',(-1.61782842764492,-1.64793709991974,
5.21439679151433));
#36689=CARTESIAN_POINT('Ctrl Pts',(0.506574022840452,-2.25309748257175,
5.32550844199978));
#36690=CARTESIAN_POINT('Ctrl Pts',(2.1675039941815,-0.796863816342033,5.43662009248521));
#36691=CARTESIAN_POINT('Ctrl Pts',(1.84535073495005,1.38843299139974,5.54773174297065));
#36692=CARTESIAN_POINT('Ctrl Pts',(-0.1651427104253,2.30343078727826,5.65884339345609));
#36693=CARTESIAN_POINT('Ctrl Pts',(-2.024544512798,1.1109838082922,5.76995504394152));
#36694=CARTESIAN_POINT('Ctrl Pts',(-2.03165894515671,-1.09791959503082,
5.88106669442697));
#36695=CARTESIAN_POINT('Ctrl Pts',(-0.179976902307884,-2.30231922661119,
5.99217834491239));
#36696=CARTESIAN_POINT('Ctrl Pts',(1.83636881720094,-1.40029106752845,6.10328999539785));
#36697=CARTESIAN_POINT('Ctrl Pts',(2.17259204728728,0.782885242326115,6.21440164588326));
#36698=CARTESIAN_POINT('Ctrl Pts',(0.521076907609949,2.24978762618687,6.32551329636872));
#36699=CARTESIAN_POINT('Ctrl Pts',(-1.60717962682088,1.6583242004264,6.43662494685413));
#36700=CARTESIAN_POINT('Ctrl Pts',(-2.26500243885858,-0.450365916286509,
6.5477365973396));
#36701=CARTESIAN_POINT('Ctrl Pts',(-0.850539171717745,-2.14700922773088,
6.65884824782501));
#36702=CARTESIAN_POINT('Ctrl Pts',(1.34209565723166,-1.87932029027199,6.76995989831046));
#36703=CARTESIAN_POINT('Ctrl Pts',(2.30682622449346,0.107788109627418,6.8810715487959));
#36704=CARTESIAN_POINT('Ctrl Pts',(1.16100547839306,1.99627948587589,6.99218319928133));
#36705=CARTESIAN_POINT('Ctrl Pts',(-1.04703729866327,2.05834360634882,7.10329484976677));
#36706=CARTESIAN_POINT('Ctrl Pts',(-2.29712931099768,0.237197038645086,
7.21440650025221));
#36707=CARTESIAN_POINT('Ctrl Pts',(-1.44554186745893,-1.80096480143545,
7.32551815073763));
#36708=CARTESIAN_POINT('Ctrl Pts',(0.72859438989827,-2.19139583863915,7.43662980122308));
#36709=CARTESIAN_POINT('Ctrl Pts',(2.23612826941383,-0.576884623911715,
7.5477414517085));
#36710=CARTESIAN_POINT('Ctrl Pts',(1.6977934979946,1.56542733614398,7.65885310219396));
#36711=CARTESIAN_POINT('Ctrl Pts',(-0.393879040694563,2.27550539615811,
7.76996475267938));
#36712=CARTESIAN_POINT('Ctrl Pts',(-2.12518549811472,0.903688057410859,
7.88107640316484));
#36713=CARTESIAN_POINT('Ctrl Pts',(-1.91212657747833,-1.29492758803799,
7.99218805365025));
#36714=CARTESIAN_POINT('Ctrl Pts',(0.0503667898133586,-2.30879377455661,
8.1032997041357));
#36715=CARTESIAN_POINT('Ctrl Pts',(1.96677879493939,-1.21030850518371,8.21441135462113));
#36716=CARTESIAN_POINT('Ctrl Pts',(2.08375418707704,0.995506903268707,8.32552300510658));
#36717=CARTESIAN_POINT('Ctrl Pts',(0.294270353677539,2.29051751091564,8.436634655592));
#36718=CARTESIAN_POINT('Ctrl Pts',(-1.76444601777748,1.4898978999011,8.54774630607746));
#36719=CARTESIAN_POINT('Ctrl Pts',(-2.2088431932234,-0.673852547682493,
8.65885795656288));
#36720=CARTESIAN_POINT('Ctrl Pts',(-0.632335256349382,-2.2210847899434,
8.76996960704833));
#36721=CARTESIAN_POINT('Ctrl Pts',(1.52270606837662,-1.73621188252162,8.88108125753376));
#36722=CARTESIAN_POINT('Ctrl Pts',(2.28459985995541,0.337148347205355,8.99219290801919));
#36723=CARTESIAN_POINT('Ctrl Pts',(0.956277562497704,2.10204633917866,9.10330455850463));
#36724=CARTESIAN_POINT('Ctrl Pts',(-1.2469579560031,1.94374924182257,9.21441620899007));
#36725=CARTESIAN_POINT('Ctrl Pts',(-2.30933226540692,0.00708579792413808,
9.32552785947551));
#36726=CARTESIAN_POINT('Ctrl Pts',(-1.25886228368054,-1.93606087509586,
9.43663950996094));
#36727=CARTESIAN_POINT('Ctrl Pts',(0.943360139257667,-2.10787462610152,
9.54775116044639));
#36728=CARTESIAN_POINT('Ctrl Pts',(2.28248823506631,-0.351162152961091,
9.65886281093181));
#36729=CARTESIAN_POINT('Ctrl Pts',(1.53333110744206,1.72683627576032,9.76997446141726));
#36730=CARTESIAN_POINT('Ctrl Pts',(-0.618692454411617,2.22492101746939,
9.88108611190268));
#36731=CARTESIAN_POINT('Ctrl Pts',(-2.20466868021367,0.687398848825245,
9.99219776238814));
#36732=CARTESIAN_POINT('Ctrl Pts',(-1.7735514221838,-1.47905058047522,10.1033094128735));
#36733=CARTESIAN_POINT('Ctrl Pts',(0.280201048116106,-2.29226437530741,
10.214421063359));
#36734=CARTESIAN_POINT('Ctrl Pts',(2.07762111854432,-1.0083052618152,10.3255327138444));
#36735=CARTESIAN_POINT('Ctrl Pts',(1.97414006873683,1.19827380577986,10.4366443643299));
#36736=CARTESIAN_POINT('Ctrl Pts',(0.0645886152005097,2.30833217918201,
10.5477560148153));
#36737=CARTESIAN_POINT('Ctrl Pts',(-1.90424854748374,1.30684465150768,10.6588676653008));
#36738=CARTESIAN_POINT('Ctrl Pts',(-2.13049227679005,-0.891025387309722,
10.7699793157862));
#36739=CARTESIAN_POINT('Ctrl Pts',(-0.408214485225542,-2.27228942196666,
10.8810909662716));
#36740=CARTESIAN_POINT('Ctrl Pts',(1.68888461736298,-1.5772814986318,10.9922026167571));
#36741=CARTESIAN_POINT('Ctrl Pts',(2.23817187934597,0.566161966084782,11.1033142672425));
#36742=CARTESIAN_POINT('Ctrl Pts',(1.24300218570944,1.64165746435707,11.1773887008995));
#36743=CARTESIAN_POINT('Ctrl Pts',(0.627850911123727,1.850383536838,11.2144259177279));
#36744=CARTESIAN_POINT('Ctrl Pts',(1.05793541951254,-1.4823699524473,-0.153382721514713));
#36745=CARTESIAN_POINT('Ctrl Pts',(1.55074231467859,-1.13066431478549,-0.116345504686234));
#36746=CARTESIAN_POINT('Ctrl Pts',(2.14955001436596,0.0967274517879858,
-0.0422710710292769));
#36747=CARTESIAN_POINT('Ctrl Pts',(1.08290436090784,1.86174541551099,0.0688405794561606));
#36748=CARTESIAN_POINT('Ctrl Pts',(-0.975409307071879,1.91793784975909,
0.179952229941597));
#36749=CARTESIAN_POINT('Ctrl Pts',(-2.14083151712633,0.22213180716797,0.291063880427034));
#36750=CARTESIAN_POINT('Ctrl Pts',(-1.34782279118508,-1.67833716661673,
0.402175530912471));
#36751=CARTESIAN_POINT('Ctrl Pts',(0.678460972679723,-2.04251926348523,
0.513287181397908));
#36752=CARTESIAN_POINT('Ctrl Pts',(2.08394142450739,-0.538362390807298,
0.624398831883346));
#36753=CARTESIAN_POINT('Ctrl Pts',(1.58282747515632,1.45855746470163,0.735510482368781));
#36754=CARTESIAN_POINT('Ctrl Pts',(-0.366459012269607,2.12091168831785,
0.84662213285422));
#36755=CARTESIAN_POINT('Ctrl Pts',(-1.98045646054783,0.842867780077688,
0.957733783339656));
#36756=CARTESIAN_POINT('Ctrl Pts',(-1.78250862301028,-1.20635899339281,
1.06884543382509));
#36757=CARTESIAN_POINT('Ctrl Pts',(0.0462869228141735,-2.15185334908375,
1.17995708431053));
#36758=CARTESIAN_POINT('Ctrl Pts',(1.83273239545565,-1.12859176615955,1.29106873479597));
#36759=CARTESIAN_POINT('Ctrl Pts',(1.94238315681312,0.927240382098824,1.4021803852814));
#36760=CARTESIAN_POINT('Ctrl Pts',(0.274916856192995,2.13472355144377,1.51329203576684));
#36761=CARTESIAN_POINT('Ctrl Pts',(-1.64407495706399,1.38911602796551,1.62440368625228));
#36762=CARTESIAN_POINT('Ctrl Pts',(-2.0588770445336,-0.62741605808422,1.73551533673771));
#36763=CARTESIAN_POINT('Ctrl Pts',(-0.589980335104445,-2.06991507018771,
1.84662698722315));
#36764=CARTESIAN_POINT('Ctrl Pts',(1.41869855984326,-1.61861665507704,1.95773863770859));
#36765=CARTESIAN_POINT('Ctrl Pts',(2.1293880179812,0.313579489369987,2.06885028819403));
#36766=CARTESIAN_POINT('Ctrl Pts',(0.891867138635642,1.95887681727571,2.17996193867946));
#36767=CARTESIAN_POINT('Ctrl Pts',(-1.16163690001897,1.8119671998123,2.2910735891649));
#36768=CARTESIAN_POINT('Ctrl Pts',(-2.1523412125303,0.0072605002547781,
2.40218523965033));
#36769=CARTESIAN_POINT('Ctrl Pts',(-1.1738349588193,-1.80408893734178,2.51329689013577));
#36770=CARTESIAN_POINT('Ctrl Pts',(0.878631217069615,-1.96484925501419,
2.62440854062121));
#36771=CARTESIAN_POINT('Ctrl Pts',(2.12722398078527,-0.327938323711113,
2.73552019110664));
#36772=CARTESIAN_POINT('Ctrl Pts',(1.42958632662274,1.60900849678758,2.84663184159209));
#36773=CARTESIAN_POINT('Ctrl Pts',(-0.57600216794938,2.07384833374845,2.95774349207752));
#36774=CARTESIAN_POINT('Ctrl Pts',(-2.05459728996263,0.641291965189069,
3.06885514256296));
#36775=CARTESIAN_POINT('Ctrl Pts',(-1.65340928710165,-1.37799243024573,
3.17996679304839));
#36776=CARTESIAN_POINT('Ctrl Pts',(0.260508675794864,-2.13653004623031,
3.29107844353384));
#36777=CARTESIAN_POINT('Ctrl Pts',(1.93608318568785,-0.940322979965331,
3.40219009401926));
#36778=CARTESIAN_POINT('Ctrl Pts',(1.84030497427301,1.11620025542831,3.51330174450471));
#36779=CARTESIAN_POINT('Ctrl Pts',(0.0608030219043116,2.15149445760286,
3.62441339499014));
#36780=CARTESIAN_POINT('Ctrl Pts',(-1.77432856410404,1.21835280406139,3.73552504547559));
#36781=CARTESIAN_POINT('Ctrl Pts',(-1.98609925645444,-0.829478843655077,
3.84663669596101));
#36782=CARTESIAN_POINT('Ctrl Pts',(-0.380756743800589,-2.11840735237885,
3.95774834644646));
#36783=CARTESIAN_POINT('Ctrl Pts',(1.57294605588646,-1.4691719143219,4.06885999693188));
#36784=CARTESIAN_POINT('Ctrl Pts',(2.08753596148093,0.524231836199493,4.17997164741733));
#36785=CARTESIAN_POINT('Ctrl Pts',(0.692206637610257,2.03800769856489,4.29108329790276));
#36786=CARTESIAN_POINT('Ctrl Pts',(-1.33643334165982,1.68717851215016,4.4021949483882));
#36787=CARTESIAN_POINT('Ctrl Pts',(-2.1423496001257,-0.207276625316418,
4.51330659887364));
#36788=CARTESIAN_POINT('Ctrl Pts',(-0.988196775702872,-1.91209114350017,
4.62441824935908));
#36789=CARTESIAN_POINT('Ctrl Pts',(1.07007270071357,-1.86750363419964,4.73552989984451));
#36790=CARTESIAN_POINT('Ctrl Pts',(2.1493159635798,-0.11430790551128,4.84664155032995));
#36791=CARTESIAN_POINT('Ctrl Pts',(1.26211650891535,1.74346990983058,4.95775320081538));
#36792=CARTESIAN_POINT('Ctrl Pts',(-0.779813036479037,2.00611989589323,
5.06886485130082));
#36793=CARTESIAN_POINT('Ctrl Pts',(-2.1082794649543,0.433339481484583,5.17997650178626));
#36794=CARTESIAN_POINT('Ctrl Pts',(-1.50784810891129,-1.53590998727594,
5.29108815227169));
#36795=CARTESIAN_POINT('Ctrl Pts',(0.472137013611209,-2.09993143910453,
5.40219980275713));
#36796=CARTESIAN_POINT('Ctrl Pts',(2.02015661416081,-0.742692845544967,
5.51331145324257));
#36797=CARTESIAN_POINT('Ctrl Pts',(1.71990340163759,1.29404702294652,5.62442310372801));
#36798=CARTESIAN_POINT('Ctrl Pts',(-0.153916274037652,2.14684307510999,
5.73553475421344));
#36799=CARTESIAN_POINT('Ctrl Pts',(-1.88691554856225,1.03545889399597,5.84664640469888));
#36800=CARTESIAN_POINT('Ctrl Pts',(-1.89354634030427,-1.02328278871562,
5.95775805518432));
#36801=CARTESIAN_POINT('Ctrl Pts',(-0.167742034418123,-2.1458070785722,
6.06886970566975));
#36802=CARTESIAN_POINT('Ctrl Pts',(1.71153207655705,-1.30509898455162,6.1799813561552));
#36803=CARTESIAN_POINT('Ctrl Pts',(2.02489878034016,0.729664537947597,6.29109300664062));
#36804=CARTESIAN_POINT('Ctrl Pts',(0.485653989206222,2.09684658745684,6.40220465712607));
#36805=CARTESIAN_POINT('Ctrl Pts',(-1.49792321581985,1.54559097049293,6.5133163076115));
#36806=CARTESIAN_POINT('Ctrl Pts',(-2.11102709394471,-0.41974994603061,
6.62442795809694));
#36807=CARTESIAN_POINT('Ctrl Pts',(-0.79271933890819,-2.0010550862688,6.73553960858237));
#36808=CARTESIAN_POINT('Ctrl Pts',(1.25085971055702,-1.7515636994031,6.84665125906781));
#36809=CARTESIAN_POINT('Ctrl Pts',(2.15000768978506,0.100460651134341,6.95776290955325));
#36810=CARTESIAN_POINT('Ctrl Pts',(1.08208008038219,1.86057198414926,7.06887456003868));
#36811=CARTESIAN_POINT('Ctrl Pts',(-0.975859481618359,1.91841697258389,
7.17998621052413));
#36812=CARTESIAN_POINT('Ctrl Pts',(-2.14096997451993,0.221072333783236,
7.29109786100956));
#36813=CARTESIAN_POINT('Ctrl Pts',(-1.34727362553083,-1.67853483327237,
7.402209511495));
#36814=CARTESIAN_POINT('Ctrl Pts',(0.679064389152043,-2.04242428597833,
7.51332116198043));
#36815=CARTESIAN_POINT('Ctrl Pts',(2.08411579664662,-0.537667885148679,
7.62443281246587));
#36816=CARTESIAN_POINT('Ctrl Pts',(1.58237713686343,1.4590092546951,7.73554446295131));
#36817=CARTESIAN_POINT('Ctrl Pts',(-0.367103060190181,2.1208160579853,7.84665611343674));
#36818=CARTESIAN_POINT('Ctrl Pts',(-1.98071493840836,0.842255152109201,
7.95776776392219));
#36819=CARTESIAN_POINT('Ctrl Pts',(-1.78213980826558,-1.20689813668469,
8.0688794144076));
#36820=CARTESIAN_POINT('Ctrl Pts',(0.0469428447876819,-2.15184148537872,
8.17999106489306));
#36821=CARTESIAN_POINT('Ctrl Pts',(1.83307675642296,-1.12803147698245,8.29110271537848));
#36822=CARTESIAN_POINT('Ctrl Pts',(1.94210013665906,0.927832133403047,8.40221436586394));
#36823=CARTESIAN_POINT('Ctrl Pts',(0.274265792786954,2.13480764600607,8.51332601634936));
#36824=CARTESIAN_POINT('Ctrl Pts',(-1.64449860425235,1.38861432550488,8.6244376668348));
#36825=CARTESIAN_POINT('Ctrl Pts',(-2.05868556570727,-0.628043908949741,
8.73554931732024));
#36826=CARTESIAN_POINT('Ctrl Pts',(-0.589348971863656,-2.07009497609277,
8.84666096780567));
#36827=CARTESIAN_POINT('Ctrl Pts',(1.41919218774748,-1.61818383148359,8.95777261829112));
#36828=CARTESIAN_POINT('Ctrl Pts',(2.12929227820989,0.314228931244718,9.06888426877654));
#36829=CARTESIAN_POINT('Ctrl Pts',(0.891269611515884,1.95914878439144,9.179995919262));
#36830=CARTESIAN_POINT('Ctrl Pts',(-1.16218949038264,1.81161275719849,9.29110756974741));
#36831=CARTESIAN_POINT('Ctrl Pts',(-2.15234336950711,0.00660410388236847,
9.40221922023287));
#36832=CARTESIAN_POINT('Ctrl Pts',(-1.17328455934639,-1.80444704726821,
9.51333087071829));
#36833=CARTESIAN_POINT('Ctrl Pts',(0.879230317440182,-1.96458086313641,
9.62444252120374));
#36834=CARTESIAN_POINT('Ctrl Pts',(2.12732420202743,-0.327290075520782,
9.73555417168917));
#36835=CARTESIAN_POINT('Ctrl Pts',(1.42909493440969,1.60944558045319,9.8466658221746));
#36836=CARTESIAN_POINT('Ctrl Pts',(-0.576633610487541,2.07367041606005,
9.95777747266004));
#36837=CARTESIAN_POINT('Ctrl Pts',(-2.05479483697499,0.640669329675303,
10.0688891231455));
#36838=CARTESIAN_POINT('Ctrl Pts',(-1.65298502134104,-1.37850440914814,
10.1800007736309));
#36839=CARTESIAN_POINT('Ctrl Pts',(0.26115292159373,-2.13643575818697,10.2911124241164));
#36840=CARTESIAN_POINT('Ctrl Pts',(1.93638399542254,-0.939760456828254,
10.4022240746018));
#36841=CARTESIAN_POINT('Ctrl Pts',(1.83993760927049,1.11681489898982,10.5133357250872));
#36842=CARTESIAN_POINT('Ctrl Pts',(0.0601978674766102,2.15141126935532,
10.6244473755726));
#36843=CARTESIAN_POINT('Ctrl Pts',(-1.77479732841649,1.21800507565884,10.7355590260581));
#36844=CARTESIAN_POINT('Ctrl Pts',(-1.98566096114678,-0.830453293000129,
10.8466706765435));
#36845=CARTESIAN_POINT('Ctrl Pts',(-0.380463978169507,-2.11781870639967,
10.957782327029));
#36846=CARTESIAN_POINT('Ctrl Pts',(1.57407388382168,-1.47005756870945,11.0688939775144));
#36847=CARTESIAN_POINT('Ctrl Pts',(2.08602048154327,0.527674155869038,11.1800056279999));
#36848=CARTESIAN_POINT('Ctrl Pts',(1.15850263419028,1.53005724266717,11.2540800616568));
#36849=CARTESIAN_POINT('Ctrl Pts',(0.585169473375027,1.72459407258861,11.2911172784853));
#36850=CARTESIAN_POINT('Ctrl Pts',(0.980771099081375,-1.37424797458507,
-0.0766913607573581));
#36851=CARTESIAN_POINT('Ctrl Pts',(1.43763335295088,-1.04819525110066,-0.0396541439288791));
#36852=CARTESIAN_POINT('Ctrl Pts',(1.99276486185844,0.089672287600667,0.0344202897280782));
#36853=CARTESIAN_POINT('Ctrl Pts',(1.00391884103562,1.72595232535247,0.145531940213516));
#36854=CARTESIAN_POINT('Ctrl Pts',(-0.904264325124765,1.77804616253862,
0.256643590698952));
#36855=CARTESIAN_POINT('Ctrl Pts',(-1.98468227953599,0.20592982580867,0.36775524118439));
#36856=CARTESIAN_POINT('Ctrl Pts',(-1.24951449388714,-1.55592161598129,
0.478866891669827));
#36857=CARTESIAN_POINT('Ctrl Pts',(0.628974984281669,-1.89354078329874,
0.589978542155263));
#36858=CARTESIAN_POINT('Ctrl Pts',(1.93194167019859,-0.499094995779056,
0.7010901926407));
#36859=CARTESIAN_POINT('Ctrl Pts',(1.46737826698393,1.35217233617898,0.812201843126137));
#36860=CARTESIAN_POINT('Ctrl Pts',(-0.339730007714042,1.96621537500318,
0.923313493611574));
#36861=CARTESIAN_POINT('Ctrl Pts',(-1.8360047538528,0.7813901905543,1.03442514409701));
#36862=CARTESIAN_POINT('Ctrl Pts',(-1.65249495296916,-1.11836886639236,
1.14553679458245));
#36863=CARTESIAN_POINT('Ctrl Pts',(0.0429108198140191,-1.99490019458391,
1.25664844506789));
#36864=CARTESIAN_POINT('Ctrl Pts',(1.69905547414348,-1.04627387125433,1.36776009555332));
#36865=CARTESIAN_POINT('Ctrl Pts',(1.80070846330345,0.859608773740392,1.47887174603876));
#36866=CARTESIAN_POINT('Ctrl Pts',(0.254864807653961,1.97901982027321,1.5899833965242));
#36867=CARTESIAN_POINT('Ctrl Pts',(-1.52415844376849,1.28779586009797,1.70109504700963));
#36868=CARTESIAN_POINT('Ctrl Pts',(-1.90870545082139,-0.581653213909888,
1.81220669749507));
#36869=CARTESIAN_POINT('Ctrl Pts',(-0.546947999872595,-1.91893837842057,
1.92331834798051));
#36870=CARTESIAN_POINT('Ctrl Pts',(1.31522068373867,-1.50055703449532,2.03442999846594));
#36871=CARTESIAN_POINT('Ctrl Pts',(1.97407345311151,0.290707442785592,2.14554164895138));
#36872=CARTESIAN_POINT('Ctrl Pts',(0.826815604866742,1.81599909938712,2.25665329943681));
#36873=CARTESIAN_POINT('Ctrl Pts',(-1.07690873956185,1.67980486264285,2.36776494992226));
#36874=CARTESIAN_POINT('Ctrl Pts',(-1.99535247395734,0.00673092958549589,
2.47887660040769));
#36875=CARTESIAN_POINT('Ctrl Pts',(-1.0882170891223,-1.67250122954812,2.58998825089313));
#36876=CARTESIAN_POINT('Ctrl Pts',(0.814545092789914,-1.82153591592328,
2.70109990137857));
#36877=CARTESIAN_POINT('Ctrl Pts',(1.97206725774273,-0.304018963960226,
2.812211551864));
#36878=CARTESIAN_POINT('Ctrl Pts',(1.325314312134,1.49164968174781,2.92332320234944));
#36879=CARTESIAN_POINT('Ctrl Pts',(-0.533989380555266,1.92258475527334,
3.03443485283487));
#36880=CARTESIAN_POINT('Ctrl Pts',(-1.90473785552499,0.594517031881129,
3.14554650332031));
#36881=CARTESIAN_POINT('Ctrl Pts',(-1.53281194091147,-1.27748360193918,
3.25665815380575));
#36882=CARTESIAN_POINT('Ctrl Pts',(0.241507539654265,-1.98069455187271,
3.36776980429119));
#36883=CARTESIAN_POINT('Ctrl Pts',(1.79486800320472,-0.871737145332536,
3.47888145477662));
#36884=CARTESIAN_POINT('Ctrl Pts',(1.70607571972046,1.03478617987453,3.58999310526206));
#36885=CARTESIAN_POINT('Ctrl Pts',(0.0563681350682242,1.99456748014249,
3.7011047557475));
#36886=CARTESIAN_POINT('Ctrl Pts',(-1.64491153604594,1.1294878653923,3.81221640623293));
#36887=CARTESIAN_POINT('Ctrl Pts',(-1.84123597216834,-0.768977824309152,
3.92332805671837));
#36888=CARTESIAN_POINT('Ctrl Pts',(-0.352984882831497,-1.96389370180267,
4.03443970720381));
#36889=CARTESIAN_POINT('Ctrl Pts',(1.45821758452731,-1.36201258278399,4.14555135768924));
#36890=CARTESIAN_POINT('Ctrl Pts',(1.93527402670466,0.485995103935303,4.25666300817468));
#36891=CARTESIAN_POINT('Ctrl Pts',(0.641718059759468,1.88935828557357,4.36777465866012));
#36892=CARTESIAN_POINT('Ctrl Pts',(-1.23895577477937,1.56411808621589,4.47888630914555));
#36893=CARTESIAN_POINT('Ctrl Pts',(-1.98608963569812,-0.1921581600124,4.58999795963099));
#36894=CARTESIAN_POINT('Ctrl Pts',(-0.916119093792434,-1.77262590680487,
4.70110961011643));
#36895=CARTESIAN_POINT('Ctrl Pts',(0.992023104075105,-1.73129054767478,
4.81222126060186));
#36896=CARTESIAN_POINT('Ctrl Pts',(1.99254788240719,-0.105970447774237,
4.9233329110873));
#36897=CARTESIAN_POINT('Ctrl Pts',(1.17005950721263,1.61630366858093,5.03444456157274));
#36898=CARTESIAN_POINT('Ctrl Pts',(-0.722934571202785,1.85979633434597,
5.14555621205818));
#36899=CARTESIAN_POINT('Ctrl Pts',(-1.95450452823164,0.401732309640217,
5.25666786254361));
#36900=CARTESIAN_POINT('Ctrl Pts',(-1.39786779017765,-1.42388287463214,
5.36777951302905));
#36901=CARTESIAN_POINT('Ctrl Pts',(0.437700004381964,-1.9467653956373,5.47889116351449));
#36902=CARTESIAN_POINT('Ctrl Pts',(1.87280923414012,-0.688521874747905,
5.59000281399993));
#36903=CARTESIAN_POINT('Ctrl Pts',(1.59445606832513,1.19966105449332,5.70111446448536));
#36904=CARTESIAN_POINT('Ctrl Pts',(-0.142689837650004,1.99025536294172,
5.81222611497081));
#36905=CARTESIAN_POINT('Ctrl Pts',(-1.74928658432651,0.959933979699734,
5.92333776545623));
#36906=CARTESIAN_POINT('Ctrl Pts',(-1.75543373545183,-0.948645982400418,
6.03444941594168));
#36907=CARTESIAN_POINT('Ctrl Pts',(-0.155507166528361,-1.98929493053321,
6.1455610664271));
#36908=CARTESIAN_POINT('Ctrl Pts',(1.58669533591315,-1.20990690157479,6.25667271691256));
#36909=CARTESIAN_POINT('Ctrl Pts',(1.87720551339304,0.676443833569079,6.36778436739797));
#36910=CARTESIAN_POINT('Ctrl Pts',(0.450231070802491,1.94390554872681,6.47889601788343));
#36911=CARTESIAN_POINT('Ctrl Pts',(-1.38866680481881,1.43285774055946,6.59000766836885));
#36912=CARTESIAN_POINT('Ctrl Pts',(-1.95705174903083,-0.38913397577471,
6.7011193188543));
#36913=CARTESIAN_POINT('Ctrl Pts',(-0.734899506098636,-1.85510094480672,
6.81223096933973));
#36914=CARTESIAN_POINT('Ctrl Pts',(1.15962376388238,-1.62380710853421,6.92334261982516));
#36915=CARTESIAN_POINT('Ctrl Pts',(1.99318915507666,0.0931331926412601,
7.03445427031061));
#36916=CARTESIAN_POINT('Ctrl Pts',(1.00315468237132,1.72486448242263,7.14556592079604));
#36917=CARTESIAN_POINT('Ctrl Pts',(-0.904681664573454,1.77849033881895,
7.25667757128148));
#36918=CARTESIAN_POINT('Ctrl Pts',(-1.98481063804218,0.204947628921387,
7.36778922176691));
#36919=CARTESIAN_POINT('Ctrl Pts',(-1.24900538360275,-1.55610486510929,
7.47890087225236));
#36920=CARTESIAN_POINT('Ctrl Pts',(0.629534388405818,-1.89345273331751,
7.59001252273779));
#36921=CARTESIAN_POINT('Ctrl Pts',(1.93210332387941,-0.498451146385645,
7.70112417322323));
#36922=CARTESIAN_POINT('Ctrl Pts',(1.46696077573226,1.35259117324623,7.81223582370866));
#36923=CARTESIAN_POINT('Ctrl Pts',(-0.340327079685797,1.96612671981249,
7.9233474741941));
#36924=CARTESIAN_POINT('Ctrl Pts',(-1.836244378702,0.780822246807544,8.03445912467955));
#36925=CARTESIAN_POINT('Ctrl Pts',(-1.65215303905282,-1.11886868533138,
8.14557077516496));
#36926=CARTESIAN_POINT('Ctrl Pts',(0.0435188997620014,-1.99488919620082,
8.25668242565042));
#36927=CARTESIAN_POINT('Ctrl Pts',(1.69937471790653,-1.04575444878119,8.36779407613584));
#36928=CARTESIAN_POINT('Ctrl Pts',(1.80044608624107,0.860157363537389,8.47890572662129));
#36929=CARTESIAN_POINT('Ctrl Pts',(0.254261231896373,1.97909778109651,8.59001737710672));
#36930=CARTESIAN_POINT('Ctrl Pts',(-1.52455119072723,1.28733075110866,8.70112902759215));
#36931=CARTESIAN_POINT('Ctrl Pts',(-1.90852793819114,-0.58223527021699,
8.8122406780776));
#36932=CARTESIAN_POINT('Ctrl Pts',(-0.546362687377931,-1.91910516224214,
8.92335232856302));
#36933=CARTESIAN_POINT('Ctrl Pts',(1.31567830711834,-1.50015578044556,9.03446397904849));
#36934=CARTESIAN_POINT('Ctrl Pts',(1.97398469646436,0.291309515284085,9.14557562953389));
#36935=CARTESIAN_POINT('Ctrl Pts',(0.826261660534066,1.81625122960423,9.25668728001935));
#36936=CARTESIAN_POINT('Ctrl Pts',(-1.07742102476217,1.67947627257441,9.36779893050478));
#36937=CARTESIAN_POINT('Ctrl Pts',(-1.99535447360731,0.00612240984059651,
9.47891058099021));
#36938=CARTESIAN_POINT('Ctrl Pts',(-1.08770683501224,-1.67283321944057,
9.59002223147566));
#36939=CARTESIAN_POINT('Ctrl Pts',(0.815100495622697,-1.82128710017129,
9.70113388196108));
#36940=CARTESIAN_POINT('Ctrl Pts',(1.97216016898856,-0.303417998080474,
9.81224553244654));
#36941=CARTESIAN_POINT('Ctrl Pts',(1.32485876137733,1.49205488514605,9.92335718293196));
#36942=CARTESIAN_POINT('Ctrl Pts',(-0.534574766563464,1.9224198146507,10.0344688334174));
#36943=CARTESIAN_POINT('Ctrl Pts',(-1.90492099373632,0.593939810525364,
10.1455804839028));
#36944=CARTESIAN_POINT('Ctrl Pts',(-1.53241862049827,-1.27795823782107,
10.2566921343883));
#36945=CARTESIAN_POINT('Ctrl Pts',(0.242104795071353,-1.98060714106653,
10.3678037848737));
#36946=CARTESIAN_POINT('Ctrl Pts',(1.79514687230076,-0.871215651841315,
10.4789154353591));
#36947=CARTESIAN_POINT('Ctrl Pts',(1.70573514980415,1.03535599219979,10.5900270858446));
#36948=CARTESIAN_POINT('Ctrl Pts',(0.055807119752709,1.99449035952863,10.70113873633));
#36949=CARTESIAN_POINT('Ctrl Pts',(-1.64534610934924,1.12916549981001,10.8122503868155));
#36950=CARTESIAN_POINT('Ctrl Pts',(-1.84082964550351,-0.769881198690536,
10.9233620373009));
#36951=CARTESIAN_POINT('Ctrl Pts',(-0.352713471113472,-1.96334799083268,
11.0344736877863));
#36952=CARTESIAN_POINT('Ctrl Pts',(1.45926315028039,-1.36283363878709,11.1455853382718));
#36953=CARTESIAN_POINT('Ctrl Pts',(1.93386908374058,0.489186345653294,11.2566969887572));
#36954=CARTESIAN_POINT('Ctrl Pts',(1.07400308267113,1.41845702097726,11.3307714224142));
#36955=CARTESIAN_POINT('Ctrl Pts',(0.542488035626326,1.59880460833922,11.3678086392426));
#36956=CARTESIAN_POINT('Ctrl Pts',(0.903606778650208,-1.26612599672284,
-2.77555756156289E-15));
#36957=CARTESIAN_POINT('Ctrl Pts',(1.32452439122316,-0.965726187415828,
0.0370372168284762));
#36958=CARTESIAN_POINT('Ctrl Pts',(1.83597970935092,0.0826171234133487,
0.111111650485434));
#36959=CARTESIAN_POINT('Ctrl Pts',(0.924933321163406,1.59015923519395,0.222223300970871));
#36960=CARTESIAN_POINT('Ctrl Pts',(-0.833119343177651,1.63815447531815,
0.333334951456308));
#36961=CARTESIAN_POINT('Ctrl Pts',(-1.82853304194564,0.18972784444937,0.444446601941745));
#36962=CARTESIAN_POINT('Ctrl Pts',(-1.15120619658919,-1.43350606534586,
0.555558252427182));
#36963=CARTESIAN_POINT('Ctrl Pts',(0.579488995883613,-1.74456230311225,
0.666669902912619));
#36964=CARTESIAN_POINT('Ctrl Pts',(1.77994191588978,-0.459827600750814,
0.777781553398056));
#36965=CARTESIAN_POINT('Ctrl Pts',(1.35192905881154,1.24578720765632,0.888893203883492));
#36966=CARTESIAN_POINT('Ctrl Pts',(-0.313001003158473,1.81151906168851,
1.00000485436893));
#36967=CARTESIAN_POINT('Ctrl Pts',(-1.69155304715778,0.719912601030908,
1.11111650485437));
#36968=CARTESIAN_POINT('Ctrl Pts',(-1.52248128292804,-1.03037873939191,
1.2222281553398));
#36969=CARTESIAN_POINT('Ctrl Pts',(0.0395347168138628,-1.83794704008407,
1.33333980582524));
#36970=CARTESIAN_POINT('Ctrl Pts',(1.56537855283131,-0.963955976349113,
1.44445145631068));
#36971=CARTESIAN_POINT('Ctrl Pts',(1.65903376979378,0.791977165381959,1.55556310679611));
#36972=CARTESIAN_POINT('Ctrl Pts',(0.234812759114929,1.82331608910266,1.66667475728155));
#36973=CARTESIAN_POINT('Ctrl Pts',(-1.404241930473,1.18647569223042,1.77778640776699));
#36974=CARTESIAN_POINT('Ctrl Pts',(-1.75853385710917,-0.535890369735552,
1.88889805825242));
#36975=CARTESIAN_POINT('Ctrl Pts',(-0.503915664640746,-1.76796168665343,
2.00000970873786));
#36976=CARTESIAN_POINT('Ctrl Pts',(1.21174280763407,-1.38249741391359,2.1111213592233));
#36977=CARTESIAN_POINT('Ctrl Pts',(1.81875888824183,0.267835396201195,2.22223300970874));
#36978=CARTESIAN_POINT('Ctrl Pts',(0.761764071097843,1.67312138149853,2.33334466019417));
#36979=CARTESIAN_POINT('Ctrl Pts',(-0.992180579104728,1.54764252547341,
2.44445631067961));
#36980=CARTESIAN_POINT('Ctrl Pts',(-1.83836373538439,0.00620135891621234,
2.55556796116504));
#36981=CARTESIAN_POINT('Ctrl Pts',(-1.0025992194253,-1.54091352175446,2.66667961165049));
#36982=CARTESIAN_POINT('Ctrl Pts',(0.750458968510211,-1.67822257683237,
2.77779126213592));
#36983=CARTESIAN_POINT('Ctrl Pts',(1.81691053470019,-0.280099604209337,
2.88890291262136));
#36984=CARTESIAN_POINT('Ctrl Pts',(1.22104229764526,1.37429086670804,3.0000145631068));
#36985=CARTESIAN_POINT('Ctrl Pts',(-0.491976593161155,1.77132117679823,
3.11112621359223));
#36986=CARTESIAN_POINT('Ctrl Pts',(-1.75487842108734,0.547742098573187,
3.22223786407767));
#36987=CARTESIAN_POINT('Ctrl Pts',(-1.41221459472129,-1.17697477363263,
3.3333495145631));
#36988=CARTESIAN_POINT('Ctrl Pts',(0.222506403513669,-1.8248590575151,3.44446116504855));
#36989=CARTESIAN_POINT('Ctrl Pts',(1.65365282072159,-0.803151310699741,
3.55557281553397));
#36990=CARTESIAN_POINT('Ctrl Pts',(1.57184646516792,0.953372104320743,3.66668446601942));
#36991=CARTESIAN_POINT('Ctrl Pts',(0.0519332482321354,1.83764050268212,
3.77779611650485));
#36992=CARTESIAN_POINT('Ctrl Pts',(-1.51549450798785,1.04062292672322,3.88890776699029));
#36993=CARTESIAN_POINT('Ctrl Pts',(-1.69637268788223,-0.708476804963227,
4.00001941747572));
#36994=CARTESIAN_POINT('Ctrl Pts',(-0.325213021862407,-1.80938005122649,
4.11113106796117));
#36995=CARTESIAN_POINT('Ctrl Pts',(1.34348911316817,-1.25485325124609,4.2222427184466));
#36996=CARTESIAN_POINT('Ctrl Pts',(1.78301209192838,0.447758371671112,4.33335436893204));
#36997=CARTESIAN_POINT('Ctrl Pts',(0.591229481908682,1.74070887258225,4.44446601941748));
#36998=CARTESIAN_POINT('Ctrl Pts',(-1.14147820789891,1.44105766028162,4.55557766990291));
#36999=CARTESIAN_POINT('Ctrl Pts',(-1.82982967127054,-0.177039694708382,
4.66668932038835));
#37000=CARTESIAN_POINT('Ctrl Pts',(-0.844041411881997,-1.63316067010957,
4.77780097087378));
#37001=CARTESIAN_POINT('Ctrl Pts',(0.913973507436636,-1.59507746114991,
4.88891262135923));
#37002=CARTESIAN_POINT('Ctrl Pts',(1.83577980123458,-0.0976329900371924,
5.00002427184466));
#37003=CARTESIAN_POINT('Ctrl Pts',(1.0780025055099,1.48913742733129,5.1111359223301));
#37004=CARTESIAN_POINT('Ctrl Pts',(-0.666056105926533,1.7134727727987,5.22224757281553));
#37005=CARTESIAN_POINT('Ctrl Pts',(-1.80072959150898,0.37012513779585,5.33335922330097));
#37006=CARTESIAN_POINT('Ctrl Pts',(-1.28788747144402,-1.31185576198834,
5.44447087378641));
#37007=CARTESIAN_POINT('Ctrl Pts',(0.403262995152723,-1.79359935217008,
5.55558252427184));
#37008=CARTESIAN_POINT('Ctrl Pts',(1.72546185411942,-0.634350903950841,
5.66669417475728));
#37009=CARTESIAN_POINT('Ctrl Pts',(1.46900873501267,1.1052750860401,5.77780582524271));
#37010=CARTESIAN_POINT('Ctrl Pts',(-0.13146340126236,1.83366765077345,5.88891747572816));
#37011=CARTESIAN_POINT('Ctrl Pts',(-1.61165762009075,0.884409065403499,
6.00002912621358));
#37012=CARTESIAN_POINT('Ctrl Pts',(-1.6173211305994,-0.87400917608522,6.11114077669903));
#37013=CARTESIAN_POINT('Ctrl Pts',(-0.143272298638598,-1.83278278249422,
6.22225242718446));
#37014=CARTESIAN_POINT('Ctrl Pts',(1.46185859526926,-1.11471481859797,6.33336407766989));
#37015=CARTESIAN_POINT('Ctrl Pts',(1.72951224644592,0.623223129190563,6.44447572815534));
#37016=CARTESIAN_POINT('Ctrl Pts',(0.414808152398764,1.79096450999678,6.55558737864077));
#37017=CARTESIAN_POINT('Ctrl Pts',(-1.27941039381778,1.320124510626,6.66669902912621));
#37018=CARTESIAN_POINT('Ctrl Pts',(-1.80307640411694,-0.358518005518811,
6.77781067961165));
#37019=CARTESIAN_POINT('Ctrl Pts',(-0.677079673289082,-1.70914680334463,
6.8889223300971));
#37020=CARTESIAN_POINT('Ctrl Pts',(1.06838781720774,-1.49605051766532,7.00003398058251));
#37021=CARTESIAN_POINT('Ctrl Pts',(1.83637062036826,0.0858057341481814,
7.11114563106797));
#37022=CARTESIAN_POINT('Ctrl Pts',(0.924229284360448,1.589156980696,7.22225728155339));
#37023=CARTESIAN_POINT('Ctrl Pts',(-0.833503847528551,1.63856370505402,
7.33336893203883));
#37024=CARTESIAN_POINT('Ctrl Pts',(-1.82865130156443,0.188822924059537,
7.44448058252428));
#37025=CARTESIAN_POINT('Ctrl Pts',(-1.15073714167466,-1.43367489694622,
7.5555922330097));
#37026=CARTESIAN_POINT('Ctrl Pts',(0.580004387659595,-1.74448118065669,
7.66670388349515));
#37027=CARTESIAN_POINT('Ctrl Pts',(1.7800908511122,-0.459234407622611,7.77781553398057));
#37028=CARTESIAN_POINT('Ctrl Pts',(1.35154441460109,1.24617309179735,7.88892718446602));
#37029=CARTESIAN_POINT('Ctrl Pts',(-0.313551099181417,1.81143738163968,
8.00003883495145));
#37030=CARTESIAN_POINT('Ctrl Pts',(-1.69177381899564,0.719389341505889,
8.11115048543689));
#37031=CARTESIAN_POINT('Ctrl Pts',(-1.52216626984007,-1.03083923397808,
8.22226213592232));
#37032=CARTESIAN_POINT('Ctrl Pts',(0.0400949547363229,-1.83793690702293,
8.33337378640777));
#37033=CARTESIAN_POINT('Ctrl Pts',(1.56567267939011,-0.963477420579929,
8.44448543689319));
#37034=CARTESIAN_POINT('Ctrl Pts',(1.65879203582308,0.792482593671729,8.55559708737864));
#37035=CARTESIAN_POINT('Ctrl Pts',(0.234256671005791,1.82338791618694,8.66670873786407));
#37036=CARTESIAN_POINT('Ctrl Pts',(-1.40460377720211,1.18604717671243,8.77782038834951));
#37037=CARTESIAN_POINT('Ctrl Pts',(-1.75837031067501,-0.536426631484242,
8.88893203883495));
#37038=CARTESIAN_POINT('Ctrl Pts',(-0.503376402892206,-1.7681153483915,
9.00004368932038));
#37039=CARTESIAN_POINT('Ctrl Pts',(1.2121644264892,-1.38212772940753,9.11115533980582));
#37040=CARTESIAN_POINT('Ctrl Pts',(1.81867711471885,0.26839009932345,9.22226699029127));
#37041=CARTESIAN_POINT('Ctrl Pts',(0.761253709552246,1.67335367481701,9.33337864077668));
#37042=CARTESIAN_POINT('Ctrl Pts',(-0.99265255914171,1.54733978795034,9.44449029126215));
#37043=CARTESIAN_POINT('Ctrl Pts',(-1.8383655777075,0.00564071579882353,
9.55560194174756));
#37044=CARTESIAN_POINT('Ctrl Pts',(-1.00212911067809,-1.54121939161292,
9.66671359223301));
#37045=CARTESIAN_POINT('Ctrl Pts',(0.750970673805211,-1.67799333720618,
9.77782524271844));
#37046=CARTESIAN_POINT('Ctrl Pts',(1.81699613594968,-0.279545920640164,
9.88893689320389));
#37047=CARTESIAN_POINT('Ctrl Pts',(1.22062258834496,1.37466418983892,10.0000485436893));
#37048=CARTESIAN_POINT('Ctrl Pts',(-0.492515922639386,1.77116921324136,
10.1111601941748));
#37049=CARTESIAN_POINT('Ctrl Pts',(-1.75504715049764,0.547210291375423,
10.2222718446602));
#37050=CARTESIAN_POINT('Ctrl Pts',(-1.4118522196555,-1.177412066494,10.3333834951456));
#37051=CARTESIAN_POINT('Ctrl Pts',(0.223056668548975,-1.82477852394609,
10.4444951456311));
#37052=CARTESIAN_POINT('Ctrl Pts',(1.65390974917898,-0.802670846854376,
10.5556067961165));
#37053=CARTESIAN_POINT('Ctrl Pts',(1.57153269033781,0.953897085409752,10.6667184466019));
#37054=CARTESIAN_POINT('Ctrl Pts',(0.0514163720288116,1.83756944970195,
10.7778300970874));
#37055=CARTESIAN_POINT('Ctrl Pts',(-1.51589489028199,1.04032592396117,10.8889417475728));
#37056=CARTESIAN_POINT('Ctrl Pts',(-1.69599832986023,-0.709309104380943,
11.0000533980583));
#37057=CARTESIAN_POINT('Ctrl Pts',(-0.324962964057439,-1.80887727526569,
11.1111650485437));
#37058=CARTESIAN_POINT('Ctrl Pts',(1.34445241673909,-1.25560970886474,11.2222766990291));
#37059=CARTESIAN_POINT('Ctrl Pts',(1.78171768593789,0.450698535437549,11.3333883495146));
#37060=CARTESIAN_POINT('Ctrl Pts',(0.989503531151977,1.30685679928735,11.4074627831715));
#37061=CARTESIAN_POINT('Ctrl Pts',(0.499806597877626,1.47301514408983,11.4445));
#37062=CARTESIAN_POINT('',(0.903606778650206,-1.26612599672284,0.));
#37063=CARTESIAN_POINT('Ctrl Pts',(0.903606778650208,-1.26612599672284,
-2.77555756156289E-15));
#37064=CARTESIAN_POINT('Ctrl Pts',(1.32452439122316,-0.965726187415828,
0.0370372168284762));
#37065=CARTESIAN_POINT('Ctrl Pts',(1.83597970935092,0.0826171234133487,
0.111111650485434));
#37066=CARTESIAN_POINT('Ctrl Pts',(0.924933321163406,1.59015923519395,0.222223300970871));
#37067=CARTESIAN_POINT('Ctrl Pts',(-0.833119343177651,1.63815447531815,
0.333334951456308));
#37068=CARTESIAN_POINT('Ctrl Pts',(-1.5310616378989,0.622578531632503,0.411241775931451));
#37069=CARTESIAN_POINT('Ctrl Pts',(-1.55772922446558,0.0543356393242454,
0.452111383578116));
#37070=CARTESIAN_POINT('Ctrl Pts',(-1.55735926886437,0.00101346774827265,
0.455943774396301));
#37071=CARTESIAN_POINT('Ctrl Pts',(0.863567639152676,1.75641488315944,2.28983498828939E-16));
#37072=CARTESIAN_POINT('Ctrl Pts',(0.902605506355985,1.73244147111074,2.48310810971475E-16));
#37073=CARTESIAN_POINT('Ctrl Pts',(0.940681517855526,1.70703362163956,1.53446104133306E-16));
#37074=CARTESIAN_POINT('Ctrl Pts',(0.977705169885396,1.68018661523996,1.12757025938492E-16));
#37075=CARTESIAN_POINT('Ctrl Pts',(1.0358643592122,1.63801357064694,3.49621561433049E-17));
#37076=CARTESIAN_POINT('Ctrl Pts',(1.09142895154027,1.59229038852923,-3.14041157591089E-18));
#37077=CARTESIAN_POINT('Ctrl Pts',(1.14423757319707,1.54335784953327,-1.00613961606655E-16));
#37078=CARTESIAN_POINT('Ctrl Pts',(1.16947625472704,1.51997165369202,-1.47199231391008E-16));
#37079=CARTESIAN_POINT('Ctrl Pts',(1.19408480623982,1.49585194230134,-1.44940981238328E-16));
#37080=CARTESIAN_POINT('Ctrl Pts',(1.21804196717247,1.47103398018765,-1.04083408558608E-16));
#37081=CARTESIAN_POINT('Ctrl Pts',(1.23020142841566,1.45843761915368,-8.33461403619852E-17));
#37082=CARTESIAN_POINT('Ctrl Pts',(1.24219304748387,1.44566136836505,-3.17714931440926E-16));
#37083=CARTESIAN_POINT('Ctrl Pts',(1.25401379483509,1.43270976178997,-3.05311331771918E-16));
#37084=CARTESIAN_POINT('Ctrl Pts',(1.26389181876557,1.42188673377951,-2.94946246493115E-16));
#37085=CARTESIAN_POINT('Ctrl Pts',(1.27364380619492,1.41094858444086,-5.46603369369435E-16));
#37086=CARTESIAN_POINT('Ctrl Pts',(1.28326720497828,1.3998998522991,-5.34294830600857E-16));
#37087=CARTESIAN_POINT('Ctrl Pts',(1.330154786252,1.3460676940429,-4.74324582576826E-16));
#37088=CARTESIAN_POINT('Ctrl Pts',(1.37400431756963,1.2896005558432,-2.78813144032988E-17));
#37089=CARTESIAN_POINT('Ctrl Pts',(1.41465239664765,1.2308327382907,1.45716771982052E-16));
#37090=CARTESIAN_POINT('Ctrl Pts',(1.44369336478921,1.18884614615641,2.69743702909727E-16));
#37091=CARTESIAN_POINT('Ctrl Pts',(1.47109927736379,1.14568453076923,1.23340209484872E-16));
#37092=CARTESIAN_POINT('Ctrl Pts',(1.4967949674738,1.10146499100096,1.52655665885959E-16));
#37093=CARTESIAN_POINT('Ctrl Pts',(1.51164370962241,1.07591189080641,1.69596158676961E-16));
#37094=CARTESIAN_POINT('Ctrl Pts',(1.5259211042574,1.05000546373499,-2.47389032972511E-16));
#37095=CARTESIAN_POINT('Ctrl Pts',(1.53961051084784,1.0237681518455,-2.63677968348475E-16));
#37096=CARTESIAN_POINT('Ctrl Pts',(1.5453767175419,1.01271655786648,-2.70539139983884E-16));
#37097=CARTESIAN_POINT('Ctrl Pts',(1.55103417937643,1.00161467257822,6.72528652799515E-17));
#37098=CARTESIAN_POINT('Ctrl Pts',(1.55658137030158,0.990465869694384,6.24500451351651E-17));
#37099=CARTESIAN_POINT('Ctrl Pts',(1.58759523113096,0.928133884781808,3.5597896440648E-17));
#37100=CARTESIAN_POINT('Ctrl Pts',(1.61517455934254,0.864320573166324,-1.32844578099872E-16));
#37101=CARTESIAN_POINT('Ctrl Pts',(1.639165272121,0.799334213601843,-1.80411241501588E-16));
#37102=CARTESIAN_POINT('Ctrl Pts',(1.66256479067373,0.735949288762567,-2.26805737281603E-16));
#37103=CARTESIAN_POINT('Ctrl Pts',(1.68255047093124,0.671447445488438,-3.92048207771591E-16));
#37104=CARTESIAN_POINT('Ctrl Pts',(1.69893099532196,0.606109731061441,-4.30211422042248E-16));
#37105=CARTESIAN_POINT('Ctrl Pts',(1.70969999791506,0.563154939181291,-4.55300957861645E-16));
#37106=CARTESIAN_POINT('Ctrl Pts',(1.71890982821634,0.519838805550124,-3.77882014063636E-16));
#37107=CARTESIAN_POINT('Ctrl Pts',(1.72649398406889,0.476242912678102,-4.71844785465692E-16));
#37108=CARTESIAN_POINT('Ctrl Pts',(1.73287054571603,0.439588616027976,-5.50846247992205E-16));
#37109=CARTESIAN_POINT('Ctrl Pts',(1.73809775889755,0.402736552578244,-9.42921937940892E-17));
#37110=CARTESIAN_POINT('Ctrl Pts',(1.74213052178609,0.36573694696249,-1.2490009027033E-16));
#37111=CARTESIAN_POINT('Ctrl Pts',(1.74338539139703,0.354223827548557,-1.34424309820125E-16));
#37112=CARTESIAN_POINT('Ctrl Pts',(1.74452450777523,0.342696049837886,-3.03274465566551E-16));
#37113=CARTESIAN_POINT('Ctrl Pts',(1.74554535151306,0.331170337018761,-2.91433543964104E-16));
#37114=CARTESIAN_POINT('Ctrl Pts',(1.75129431083391,0.266262406759456,-2.24750491415529E-16));
#37115=CARTESIAN_POINT('Ctrl Pts',(1.75331011127704,0.201301920292928,9.80627071070611E-17));
#37116=CARTESIAN_POINT('Ctrl Pts',(1.75142561531544,0.136549272921142,2.77555756156289E-17));
#37117=CARTESIAN_POINT('Ctrl Pts',(1.75088296778463,0.11790351037964,7.510378979319E-18));
#37118=CARTESIAN_POINT('Ctrl Pts',(1.75001659332986,0.099275023041261,-5.08054903583662E-16));
#37119=CARTESIAN_POINT('Ctrl Pts',(1.74882170147482,0.0806701752180915,
-4.85722573273506E-16));
#37120=CARTESIAN_POINT('Ctrl Pts',(1.74442082328573,0.0121470962041962,
-4.16579971360731E-16));
#37121=CARTESIAN_POINT('Ctrl Pts',(1.73556771390717,-0.056057442313777,
-1.52368272571946E-16));
#37122=CARTESIAN_POINT('Ctrl Pts',(1.72245534586321,-0.123606275893366,
-5.55111512312578E-17));
#37123=CARTESIAN_POINT('Ctrl Pts',(1.71065390208195,-0.184401836184713,
3.16625666268892E-17));
#37124=CARTESIAN_POINT('Ctrl Pts',(1.69540107690307,-0.244666544752314,
-5.10914177950054E-16));
#37125=CARTESIAN_POINT('Ctrl Pts',(1.67680493801022,-0.304129401844208,
-5.82867087928207E-16));
#37126=CARTESIAN_POINT('Ctrl Pts',(1.67349552259788,-0.314711560692091,
-5.95672007842828E-16));
#37127=CARTESIAN_POINT('Ctrl Pts',(1.67008173945308,-0.325263020743978,
-2.82234476894323E-16));
#37128=CARTESIAN_POINT('Ctrl Pts',(1.66656691458475,-0.335775244456298,
-2.77555756156289E-16));
#37129=CARTESIAN_POINT('Ctrl Pts',(1.64601434320315,-0.39724437487395,-2.5019742521657E-16));
#37130=CARTESIAN_POINT('Ctrl Pts',(1.6219871213203,-0.457449913435399,-1.49651752513019E-16));
#37131=CARTESIAN_POINT('Ctrl Pts',(1.59467186427628,-0.5161179062652,-1.94289029309402E-16));
#37132=CARTESIAN_POINT('Ctrl Pts',(1.56746479951959,-0.57455352257637,-2.38749503483388E-16));
#37133=CARTESIAN_POINT('Ctrl Pts',(1.53699493854014,-0.631464584970275,
-4.11608014004163E-16));
#37134=CARTESIAN_POINT('Ctrl Pts',(1.50340708769257,-0.686547887629179,
-4.71844785465692E-16));
#37135=CARTESIAN_POINT('Ctrl Pts',(1.47050686756616,-0.740503491725204,
-5.30848353445754E-16));
#37136=CARTESIAN_POINT('Ctrl Pts',(1.43461427022078,-0.792706028859038,
8.26037042042841E-17));
#37137=CARTESIAN_POINT('Ctrl Pts',(1.39583852741916,-0.842828743497358,
1.94289029309402E-16));
#37138=CARTESIAN_POINT('Ctrl Pts',(1.38891448399703,-0.851778974428235,
2.14232271779286E-16));
#37139=CARTESIAN_POINT('Ctrl Pts',(1.38189845475662,-0.860662765012678,
1.05754276149716E-16));
#37140=CARTESIAN_POINT('Ctrl Pts',(1.3747909965488,-0.869478087839508,1.11022302462516E-16));
#37141=CARTESIAN_POINT('Ctrl Pts',(1.36801000346398,-0.877888498619479,
1.1604835382339E-16));
#37142=CARTESIAN_POINT('Ctrl Pts',(1.36114891147745,-0.8862326313589,4.78426519390645E-16));
#37143=CARTESIAN_POINT('Ctrl Pts',(1.35421355798306,-0.894502968665375,
4.71844785465692E-16));
#37144=CARTESIAN_POINT('Ctrl Pts',(1.3143417576089,-0.942049678199007,4.34005967100638E-16));
#37145=CARTESIAN_POINT('Ctrl Pts',(1.27196760499602,-0.987223303029092,
-4.84873724376989E-16));
#37146=CARTESIAN_POINT('Ctrl Pts',(1.22722986402911,-1.02975664627632,-3.05311331771918E-16));
#37147=CARTESIAN_POINT('Ctrl Pts',(1.18329662429212,-1.07152512911229,-1.2897793916942E-16));
#37148=CARTESIAN_POINT('Ctrl Pts',(1.13708333146208,-1.1107479710078,1.42267300457324E-16));
#37149=CARTESIAN_POINT('Ctrl Pts',(1.08869802628341,-1.14712822354107,1.94289029309402E-16));
#37150=CARTESIAN_POINT('Ctrl Pts',(1.04185702701945,-1.1823473334721,2.44650389103912E-16));
#37151=CARTESIAN_POINT('Ctrl Pts',(0.99297984330778,-1.21490270865201,1.66616011326585E-16));
#37152=CARTESIAN_POINT('Ctrl Pts',(0.942151955941521,-1.24447758118399,
1.11022302462516E-16));
#37153=CARTESIAN_POINT('Ctrl Pts',(0.929425469464971,-1.25188265416315,
9.71025308430195E-17));
#37154=CARTESIAN_POINT('Ctrl Pts',(0.916576650468056,-1.25910062269163,
1.9641793555709E-16));
#37155=CARTESIAN_POINT('Ctrl Pts',(0.903606778650242,-1.26612599672281,
1.94289029309402E-16));
#37156=CARTESIAN_POINT('Ctrl Pts',(1.88079991776263,-0.516378774142081,
11.046));
#37157=CARTESIAN_POINT('Ctrl Pts',(1.79754570390634,-0.821182550519846,
11.028067538919));
#37158=CARTESIAN_POINT('Ctrl Pts',(1.64446793279769,-1.10682480125595,11.010135077838));
#37159=CARTESIAN_POINT('Ctrl Pts',(1.43091597726206,-1.33587557506818,10.9922026167571));
#37160=CARTESIAN_POINT('Ctrl Pts',(0.9898515831668,-1.80895080641009,10.9551653999286));
#37161=CARTESIAN_POINT('Ctrl Pts',(0.290818548970629,-2.04062011418838,
10.9181281831001));
#37162=CARTESIAN_POINT('Ctrl Pts',(-0.345744266721549,-1.9262440956347,
10.8810909662716));
#37163=CARTESIAN_POINT('Ctrl Pts',(-0.982307082413709,-1.81186807708102,
10.8440537494431));
#37164=CARTESIAN_POINT('Ctrl Pts',(-1.55639967960188,-1.35144673219537,
10.8070165326147));
#37165=CARTESIAN_POINT('Ctrl Pts',(-1.80573868997825,-0.754924386616321,
10.7699793157862));
#37166=CARTESIAN_POINT('Ctrl Pts',(-1.90472245868201,-0.518114150655666,
10.7552761078989));
#37167=CARTESIAN_POINT('Ctrl Pts',(-1.95252608806662,-0.259854826956367,
10.7405729000116));
#37168=CARTESIAN_POINT('Ctrl Pts',(-1.95129684289216,-0.00113636086278679,
10.7258696921242));
#37169=CARTESIAN_POINT('Origin',(0.,0.,-1.29405622560369));
#37170=CARTESIAN_POINT('',(-0.903606778650172,-1.26612599672286,0.));
#37171=CARTESIAN_POINT('Ctrl Pts',(-0.905549614304886,-1.26792015305981,
1.24276674021151E-15));
#37172=CARTESIAN_POINT('Ctrl Pts',(-0.513706458239086,-1.54472437079514,
0.0344950590738082));
#37173=CARTESIAN_POINT('Ctrl Pts',(0.587535178885047,-1.72169358136003,
0.106052258091336));
#37174=CARTESIAN_POINT('Ctrl Pts',(1.77508460417327,-0.479721809770191,
0.214671597052585));
#37175=CARTESIAN_POINT('Ctrl Pts',(1.3650560094313,1.23222299189869,0.325858016883748));
#37176=CARTESIAN_POINT('Ctrl Pts',(-0.295638381403906,1.81478253869214,
0.43704443671491));
#37177=CARTESIAN_POINT('Ctrl Pts',(-1.41307745535963,0.946781319192958,
0.526443839621562));
#37178=CARTESIAN_POINT('Ctrl Pts',(-1.55414936746312,0.214718667413076,
0.578781102584494));
#37179=CARTESIAN_POINT('Ctrl Pts',(-1.55326046963413,0.000729270061605551,
0.594056225603705));
#37180=CARTESIAN_POINT('Origin',(0.,0.,0.));
#37181=CARTESIAN_POINT('Ctrl Pts',(-0.685825729128748,1.39614588036674,
-0.230074082272066));
#37182=CARTESIAN_POINT('Ctrl Pts',(-1.15028016933624,1.16799292759742,-0.193011942328345));
#37183=CARTESIAN_POINT('Ctrl Pts',(-1.82555218707277,0.215691441263552,
-0.118887662440903));
#37184=CARTESIAN_POINT('Ctrl Pts',(-1.16942936218886,-1.42059634545264,
-0.00770124260974049));
#37185=CARTESIAN_POINT('Ctrl Pts',(0.559468948314244,-1.75104601534012,
0.103485177221422));
#37186=CARTESIAN_POINT('Ctrl Pts',(1.77508460417327,-0.479721809770191,
0.214671597052585));
#37187=CARTESIAN_POINT('Ctrl Pts',(1.3650560094313,1.23222299189869,0.325858016883748));
#37188=CARTESIAN_POINT('Ctrl Pts',(-0.295638381403906,1.81478253869214,
0.43704443671491));
#37189=CARTESIAN_POINT('Ctrl Pts',(-1.68540213790592,0.735245708832444,
0.548230856546073));
#37190=CARTESIAN_POINT('Ctrl Pts',(-1.53132379752993,-1.01797781965797,
0.659417276377235));
#37191=CARTESIAN_POINT('Ctrl Pts',(0.0255447675030308,-1.83860034663711,
0.770603696208398));
#37192=CARTESIAN_POINT('Ctrl Pts',(1.55899683301632,-0.975032021788082,
0.881790116039561));
#37193=CARTESIAN_POINT('Ctrl Pts',(1.66434877052597,0.781732535368643,0.992976535870723));
#37194=CARTESIAN_POINT('Ctrl Pts',(0.245080507541896,1.82238325373942,1.10416295570189));
#37195=CARTESIAN_POINT('Ctrl Pts',(-1.39868975820189,1.19365863723167,1.21534937553305));
#37196=CARTESIAN_POINT('Ctrl Pts',(-1.76120077222934,-0.528512641939849,
1.32653579536421));
#37197=CARTESIAN_POINT('Ctrl Pts',(-0.510374815939226,-1.76654153931159,
1.43772221519537));
#37198=CARTESIAN_POINT('Ctrl Pts',(1.20797626960931,-1.38634273102519,1.54890863502654));
#37199=CARTESIAN_POINT('Ctrl Pts',(1.81976886629041,0.263806680570579,1.6600950548577));
#37200=CARTESIAN_POINT('Ctrl Pts',(0.764574137846417,1.67229745635935,1.77128147468886));
#37201=CARTESIAN_POINT('Ctrl Pts',(-0.991003621173195,1.54889135395602,
1.88246789452002));
#37202=CARTESIAN_POINT('Ctrl Pts',(-1.83877909581896,0.00663349951290586,
1.99365431435119));
#37203=CARTESIAN_POINT('Ctrl Pts',(-1.00215313155719,-1.54170088892816,
2.10484073418235));
#37204=CARTESIAN_POINT('Ctrl Pts',(0.752488571272716,-1.67777039880966,
2.21602715401351));
#37205=CARTESIAN_POINT('Ctrl Pts',(1.81781810074028,-0.276929424335053,
2.32721357384467));
#37206=CARTESIAN_POINT('Ctrl Pts',(1.21794738393109,1.37759091140133,2.43839999367584));
#37207=CARTESIAN_POINT('Ctrl Pts',(-0.497615974795104,1.77017821004958,
2.549586413507));
#37208=CARTESIAN_POINT('Ctrl Pts',(-1.75734151264734,0.541205469518692,
2.66077283333817));
#37209=CARTESIAN_POINT('Ctrl Pts',(-1.40726598433086,-1.1835349598584,2.77195925316932));
#37210=CARTESIAN_POINT('Ctrl Pts',(0.231926238140432,-1.82410602009977,
2.88314567300049));
#37211=CARTESIAN_POINT('Ctrl Pts',(1.65866396469461,-0.793716828903688,
2.99433209283165));
#37212=CARTESIAN_POINT('Ctrl Pts',(1.56599354026699,0.96375141196464,3.10551851266282));
#37213=CARTESIAN_POINT('Ctrl Pts',(0.0388050940998321,1.83838154825996,
3.21670493249398));
#37214=CARTESIAN_POINT('Ctrl Pts',(-1.52393050178991,1.02897443019027,3.32789135232514));
#37215=CARTESIAN_POINT('Ctrl Pts',(-1.69067964401488,-0.723017906820314,
3.4390777721563));
#37216=CARTESIAN_POINT('Ctrl Pts',(-0.308692884081366,-1.81269447386996,
3.55026419198746));
#37217=CARTESIAN_POINT('Ctrl Pts',(1.35606994996762,-1.24186426112907,3.66145061181863));
#37218=CARTESIAN_POINT('Ctrl Pts',(1.77861387826841,0.466567491694538,3.77263703164979));
#37219=CARTESIAN_POINT('Ctrl Pts',(0.571870330903418,1.74760318061885,3.88382345148095));
#37220=CARTESIAN_POINT('Ctrl Pts',(-1.15873124952358,1.42775853828764,3.99500987131212));
#37221=CARTESIAN_POINT('Ctrl Pts',(-1.82788473512851,-0.199974866820836,
4.10619629114327));
#37222=CARTESIAN_POINT('Ctrl Pts',(-0.822616502622442,-1.64452261823584,
4.21738271097444));
#37223=CARTESIAN_POINT('Ctrl Pts',(0.936204134582059,-1.58261630557358,
4.3285691308056));
#37224=CARTESIAN_POINT('Ctrl Pts',(1.83742116834086,-0.0709647969689106,
4.43975555063676));
#37225=CARTESIAN_POINT('Ctrl Pts',(1.0554806974386,1.50569354438759,4.55094197046793));
#37226=CARTESIAN_POINT('Ctrl Pts',(-0.693325883166112,1.70307127625589,
4.66212839029909));
#37227=CARTESIAN_POINT('Ctrl Pts',(-1.80701587562324,0.340361833232659,
4.77331481013025));
#37228=CARTESIAN_POINT('Ctrl Pts',(-1.26540093064824,-1.33413381524886,
4.88450122996142));
#37229=CARTESIAN_POINT('Ctrl Pts',(0.435376164803608,-1.7865050090601,4.99568764979258));
#37230=CARTESIAN_POINT('Ctrl Pts',(1.73732980498774,-0.602360109052031,
5.10687406962374));
#37231=CARTESIAN_POINT('Ctrl Pts',(1.44781397169404,1.13357278356683,5.21806048945491));
#37232=CARTESIAN_POINT('Ctrl Pts',(-0.167962271460079,1.83110382765203,
5.32924690928607));
#37233=CARTESIAN_POINT('Ctrl Pts',(-1.62987778710162,0.851264325217889,
5.44043332911723));
#37234=CARTESIAN_POINT('Ctrl Pts',(-1.59875453933454,-0.908370230265797,
5.55161974894839));
#37235=CARTESIAN_POINT('Ctrl Pts',(-0.103102773360761,-1.83589824620028,
5.66280616877956));
#37236=CARTESIAN_POINT('Ctrl Pts',(1.4869956060099,-1.08166382022474,5.77399258861071));
#37237=CARTESIAN_POINT('Ctrl Pts',(1.71494149863546,0.663421591850831,5.88517900844189));
#37238=CARTESIAN_POINT('Ctrl Pts',(0.371926577693494,1.80078404398782,5.99636542827304));
#37239=CARTESIAN_POINT('Ctrl Pts',(-1.311789224034,1.28855018683177,6.10755184810421));
#37240=CARTESIAN_POINT('Ctrl Pts',(-1.79384918603911,-0.404051543769803,
6.21873826793537));
#37241=CARTESIAN_POINT('Ctrl Pts',(-0.632665469493242,-1.72652453095426,
6.32992468776653));
#37242=CARTESIAN_POINT('Ctrl Pts',(1.10806726459172,-1.46742614445027,6.44111110759769));
#37243=CARTESIAN_POINT('Ctrl Pts',(1.83376231205259,0.135898253011021,6.55229752742886));
#37244=CARTESIAN_POINT('Ctrl Pts',(0.879651525947856,1.61473395492061,6.66348394726001));
#37245=CARTESIAN_POINT('Ctrl Pts',(-0.880258220622017,1.61440330069759,
6.77467036709119));
#37246=CARTESIAN_POINT('Ctrl Pts',(-1.83381324808445,0.13520918395534,6.88585678692234));
#37247=CARTESIAN_POINT('Ctrl Pts',(-1.1075157823663,-1.46784241118916,6.99704320675351));
#37248=CARTESIAN_POINT('Ctrl Pts',(0.633314188332071,-1.72628667698419,
7.10822962658467));
#37249=CARTESIAN_POINT('Ctrl Pts',(1.7940008868909,-0.403377453646542,7.21941604641583));
#37250=CARTESIAN_POINT('Ctrl Pts',(1.31130494233742,1.28904301731096,7.33060246624699));
#37251=CARTESIAN_POINT('Ctrl Pts',(-0.372603218894873,1.80064416072257,
7.44178888607816));
#37252=CARTESIAN_POINT('Ctrl Pts',(-1.71519066664489,0.662777133981789,
7.55297530590932));
#37253=CARTESIAN_POINT('Ctrl Pts',(-1.48658905212271,-1.08222250133236,
7.66416172574049));
#37254=CARTESIAN_POINT('Ctrl Pts',(0.103792628149562,-1.8358593744105,7.77534814557165));
#37255=CARTESIAN_POINT('Ctrl Pts',(1.59909575810308,-0.907769413831382,
7.8865345654028));
#37256=CARTESIAN_POINT('Ctrl Pts',(1.62955779866738,0.851876712390422,7.99772098523398));
#37257=CARTESIAN_POINT('Ctrl Pts',(0.167274199086701,1.83116681231986,8.10890740506512));
#37258=CARTESIAN_POINT('Ctrl Pts',(-1.44823982381472,1.1330286690894,8.2200938248963));
#37259=CARTESIAN_POINT('Ctrl Pts',(-1.73710333792674,-0.603012890298399,
8.33128024472746));
#37260=CARTESIAN_POINT('Ctrl Pts',(-0.434704832044991,-1.78666848096071,
8.44246666455862));
#37261=CARTESIAN_POINT('Ctrl Pts',(1.26590215885116,-1.33365823077974,8.55365308438979));
#37262=CARTESIAN_POINT('Ctrl Pts',(1.8068878531032,0.341040818691465,8.66483950422094));
#37263=CARTESIAN_POINT('Ctrl Pts',(0.69268588294083,1.70333168137465,8.77602592405212));
#37264=CARTESIAN_POINT('Ctrl Pts',(-1.05604640517969,1.5052968290502,8.88721234388326));
#37265=CARTESIAN_POINT('Ctrl Pts',(-1.83739437498563,-0.0716552286239433,
8.99839876371444));
#37266=CARTESIAN_POINT('Ctrl Pts',(-0.935609375970031,-1.5829679799695,
9.1095851835456));
#37267=CARTESIAN_POINT('Ctrl Pts',(0.823234386500799,-1.64421340203127,
9.22077160337675));
#37268=CARTESIAN_POINT('Ctrl Pts',(1.82795976495949,-0.199287985657338,
9.33195802320793));
#37269=CARTESIAN_POINT('Ctrl Pts',(1.15819463928053,1.42819381470141,9.44314444303908));
#37270=CARTESIAN_POINT('Ctrl Pts',(-0.572526917402423,1.74738822826618,
9.55433086287024));
#37271=CARTESIAN_POINT('Ctrl Pts',(-1.77878918025408,0.46589901053406,9.66551728270142));
#37272=CARTESIAN_POINT('Ctrl Pts',(-1.35560300066214,-1.24237352171324,
9.77670370253256));
#37273=CARTESIAN_POINT('Ctrl Pts',(0.309373610575528,-1.81257875466721,
9.88789012236375));
#37274=CARTESIAN_POINT('Ctrl Pts',(1.69095195914933,-0.722381792257861,
9.99907654219489));
#37275=CARTESIAN_POINT('Ctrl Pts',(1.52354231364944,1.0295455294481,10.1102629620261));
#37276=CARTESIAN_POINT('Ctrl Pts',(-0.0394931635484403,1.83836962465064,
10.2214493818572));
#37277=CARTESIAN_POINT('Ctrl Pts',(-1.56636075542215,0.963157594965877,
10.3326358016884));
#37278=CARTESIAN_POINT('Ctrl Pts',(-1.65835572967195,-0.794329933758677,
10.4438222215196));
#37279=CARTESIAN_POINT('Ctrl Pts',(-0.231259578302998,-1.82421227428175,
10.5550086413507));
#37280=CARTESIAN_POINT('Ctrl Pts',(1.40774638007895,-1.1829694620695,10.6661950611819));
#37281=CARTESIAN_POINT('Ctrl Pts',(1.75706993010233,0.541796064983141,10.7773814810131));
#37282=CARTESIAN_POINT('Ctrl Pts',(0.497080432048737,1.77049779856472,10.8885679008442));
#37283=CARTESIAN_POINT('Ctrl Pts',(-1.21871201614337,1.37688031013954,10.9997543206754));
#37284=CARTESIAN_POINT('Ctrl Pts',(-1.81724153253684,-0.27712968875509,
11.1109407405065));
#37285=CARTESIAN_POINT('Ctrl Pts',(-0.75277483453787,-1.67898453189698,
11.2221271603377));
#37286=CARTESIAN_POINT('Ctrl Pts',(1.00462758039806,-1.53944373403644,11.3333135801688));
#37287=CARTESIAN_POINT('Ctrl Pts',(1.55754888396286,-0.511266487217653,
11.4074378600563));
#37288=CARTESIAN_POINT('Ctrl Pts',(1.55548765964692,0.00619602180124784,
11.4445));
#37289=CARTESIAN_POINT('Ctrl Pts',(-0.74439243930934,1.51537102412034,-0.153382721514711));
#37290=CARTESIAN_POINT('Ctrl Pts',(-1.24850938769699,1.26773474301532,-0.11632058157099));
#37291=CARTESIAN_POINT('Ctrl Pts',(-1.98144687185762,0.234110607521693,
-0.042196301683548));
#37292=CARTESIAN_POINT('Ctrl Pts',(-1.26929384324154,-1.54190945884872,
0.0689901181476148));
#37293=CARTESIAN_POINT('Ctrl Pts',(0.607245306591998,-1.90057817801302,
0.180176537978778));
#37294=CARTESIAN_POINT('Ctrl Pts',(1.92666956394248,-0.520688088821623,
0.29136295780994));
#37295=CARTESIAN_POINT('Ctrl Pts',(1.48162620545796,1.33744979191402,0.402549377641103));
#37296=CARTESIAN_POINT('Ctrl Pts',(-0.320884689126903,1.9697575395855,0.513735797472264));
#37297=CARTESIAN_POINT('Ctrl Pts',(-1.82932858212653,0.798032683003624,
0.624922217303428));
#37298=CARTESIAN_POINT('Ctrl Pts',(-1.66209258212561,-1.10490895887015,
0.736108637134591));
#37299=CARTESIAN_POINT('Ctrl Pts',(0.0277261860929502,-1.99560929084259,
0.847295056965753));
#37300=CARTESIAN_POINT('Ctrl Pts',(1.69212878157669,-1.0582957656395,0.958481476796916));
#37301=CARTESIAN_POINT('Ctrl Pts',(1.80647734334385,0.848489294255244,1.06966789662808));
#37302=CARTESIAN_POINT('Ctrl Pts',(0.266009379770665,1.97800732458805,1.18085431645924));
#37303=CARTESIAN_POINT('Ctrl Pts',(-1.51813213871049,1.2955921992025,1.29204073629041));
#37304=CARTESIAN_POINT('Ctrl Pts',(-1.91160010957712,-0.573645458357494,
1.40322715612156));
#37305=CARTESIAN_POINT('Ctrl Pts',(-0.553958736254638,-1.91739695630841,
1.51441357595273));
#37306=CARTESIAN_POINT('Ctrl Pts',(1.31113249878304,-1.50473072594935,1.62559999578389));
#37307=CARTESIAN_POINT('Ctrl Pts',(1.9751696791516,0.286334691329668,1.73678641561505));
#37308=CARTESIAN_POINT('Ctrl Pts',(0.829865639814035,1.81510481441338,1.84797283544622));
#37309=CARTESIAN_POINT('Ctrl Pts',(-1.07563127424026,1.68116033596642,1.95915925527738));
#37310=CARTESIAN_POINT('Ctrl Pts',(-1.99580330447296,0.00719997322039096,
2.07034567510854));
#37311=CARTESIAN_POINT('Ctrl Pts',(-1.08773290717609,-1.67335583465575,
2.18153209493971));
#37312=CARTESIAN_POINT('Ctrl Pts',(0.816748015321165,-1.82104512374819,
2.29271851477087));
#37313=CARTESIAN_POINT('Ctrl Pts',(1.97305232620797,-0.300578063700233,
2.40390493460203));
#37314=CARTESIAN_POINT('Ctrl Pts',(1.32195510545613,1.49523153675082,2.51509135443319));
#37315=CARTESIAN_POINT('Ctrl Pts',(-0.54011034229875,1.92134418384253,2.62627777426435));
#37316=CARTESIAN_POINT('Ctrl Pts',(-1.90741128502276,0.587422201459822,
2.73746419409552));
#37317=CARTESIAN_POINT('Ctrl Pts',(-1.52744073944838,-1.28460400121777,
2.84865061392668));
#37318=CARTESIAN_POINT('Ctrl Pts',(0.251731789602741,-1.9798772081443,2.95983703375785));
#37319=CARTESIAN_POINT('Ctrl Pts',(1.80030707836241,-0.861496997406464,
3.071023453589));
#37320=CARTESIAN_POINT('Ctrl Pts',(1.69972297898904,1.04605183790867,3.18220987342017));
#37321=CARTESIAN_POINT('Ctrl Pts',(0.0421188903066005,1.99537180797957,
3.29339629325133));
#37322=CARTESIAN_POINT('Ctrl Pts',(-1.65406792919015,1.11684463493277,3.4045827130825));
#37323=CARTESIAN_POINT('Ctrl Pts',(-1.83505676565636,-0.784760676748056,
3.51576913291366));
#37324=CARTESIAN_POINT('Ctrl Pts',(-0.335053992900935,-1.96749116257395,
3.62695555274482));
#37325=CARTESIAN_POINT('Ctrl Pts',(1.47187277329603,-1.34791438607496,3.73814197257599));
#37326=CARTESIAN_POINT('Ctrl Pts',(1.93050022360002,0.506410445822938,3.84932839240714));
#37327=CARTESIAN_POINT('Ctrl Pts',(0.620705716495424,1.89684133929807,3.96051481223831));
#37328=CARTESIAN_POINT('Ctrl Pts',(-1.25768215554202,1.54968327363698,4.07170123206947));
#37329=CARTESIAN_POINT('Ctrl Pts',(-1.9839786099702,-0.217051901949521,
4.18288765190064));
#37330=CARTESIAN_POINT('Ctrl Pts',(-0.892864584974339,-1.78495811879663,
4.29407407173179));
#37331=CARTESIAN_POINT('Ctrl Pts',(1.01615213578872,-1.71776526041577,4.40526049156296));
#37332=CARTESIAN_POINT('Ctrl Pts',(1.99432941554622,-0.0770249001709277,
4.51644691139412));
#37333=CARTESIAN_POINT('Ctrl Pts',(1.14561442891388,1.6342736102696,4.62763333122529));
#37334=CARTESIAN_POINT('Ctrl Pts',(-0.752533075803338,1.84850659257176,
4.73881975105645));
#37335=CARTESIAN_POINT('Ctrl Pts',(-1.96132763527948,0.369427340688636,
4.85000617088761));
#37336=CARTESIAN_POINT('Ctrl Pts',(-1.3734609908354,-1.44806338245697,4.96119259071877));
#37337=CARTESIAN_POINT('Ctrl Pts',(0.472555507281729,-1.9390652246629,5.07237901054994));
#37338=CARTESIAN_POINT('Ctrl Pts',(1.88569065943703,-0.653799196903168,
5.1835654303811));
#37339=CARTESIAN_POINT('Ctrl Pts',(1.57145135896933,1.23037525956625,5.29475185021226));
#37340=CARTESIAN_POINT('Ctrl Pts',(-0.182305561972616,1.98747259981946,
5.40593827004342));
#37341=CARTESIAN_POINT('Ctrl Pts',(-1.76906267902489,0.923958814363803,
5.51712468987459));
#37342=CARTESIAN_POINT('Ctrl Pts',(-1.73528163328608,-0.985941329968107,
5.62831110970574));
#37343=CARTESIAN_POINT('Ctrl Pts',(-0.111907328205795,-1.99267644208816,
5.73949752953692));
#37344=CARTESIAN_POINT('Ctrl Pts',(1.61397894448518,-1.17403348321834,5.85068394936807));
#37345=CARTESIAN_POINT('Ctrl Pts',(1.86139048335769,0.720075080408093,5.96187036919923));
#37346=CARTESIAN_POINT('Ctrl Pts',(0.403687585131819,1.9545636307293,6.0730567890304));
#37347=CARTESIAN_POINT('Ctrl Pts',(-1.42381065460884,1.39858709874703,6.18424320886156));
#37348=CARTESIAN_POINT('Ctrl Pts',(-1.94703656429618,-0.438555891823412,
6.29542962869273));
#37349=CARTESIAN_POINT('Ctrl Pts',(-0.686692511086116,-1.87396265922711,
6.40661604852388));
#37350=CARTESIAN_POINT('Ctrl Pts',(1.20269167366484,-1.59273833100625,6.51780246835505));
#37351=CARTESIAN_POINT('Ctrl Pts',(1.99035810790665,0.147503407586138,6.62898888818621));
#37352=CARTESIAN_POINT('Ctrl Pts',(0.954770165847204,1.75262562555938,6.74017530801738));
#37353=CARTESIAN_POINT('Ctrl Pts',(-0.9554286697633,1.7522667348191,6.85136172784854));
#37354=CARTESIAN_POINT('Ctrl Pts',(-1.99041339366714,0.146755494853507,
6.9625481476797));
#37355=CARTESIAN_POINT('Ctrl Pts',(-1.20209309711463,-1.59319014522084,
7.07373456751086));
#37356=CARTESIAN_POINT('Ctrl Pts',(0.687396627858533,-1.87370449350154,
7.18492098734203));
#37357=CARTESIAN_POINT('Ctrl Pts',(1.94720121977979,-0.437824237162718,
7.29610740717318));
#37358=CARTESIAN_POINT('Ctrl Pts',(1.42328501723757,1.39912201493195,7.40729382700435));
#37359=CARTESIAN_POINT('Ctrl Pts',(-0.404422008722263,1.95441180200575,
7.51848024683551));
#37360=CARTESIAN_POINT('Ctrl Pts',(-1.86166092929526,0.719375588474842,
7.62966666666667));
#37361=CARTESIAN_POINT('Ctrl Pts',(-1.61353767256008,-1.17463987340584,
7.74085308649784));
#37362=CARTESIAN_POINT('Ctrl Pts',(0.112656093769942,-1.99263425080664,
7.852039506329));
#37363=CARTESIAN_POINT('Ctrl Pts',(1.73565199074082,-0.985289206269375,
7.96322592616017));
#37364=CARTESIAN_POINT('Ctrl Pts',(1.76871536488809,0.924623496894334,8.07441234599133));
#37365=CARTESIAN_POINT('Ctrl Pts',(0.181558731034875,1.98754096312013,8.18559876582249));
#37366=CARTESIAN_POINT('Ctrl Pts',(-1.57191357711808,1.22978467993954,8.29678518565365));
#37367=CARTESIAN_POINT('Ctrl Pts',(-1.88544485301595,-0.6545077229961,8.40797160548482));
#37368=CARTESIAN_POINT('Ctrl Pts',(-0.471826845453332,-1.93924265639472,
8.51915802531597));
#37369=CARTESIAN_POINT('Ctrl Pts',(1.37400502187529,-1.44754718502077,8.63034444514714));
#37370=CARTESIAN_POINT('Ctrl Pts',(1.96118868016023,0.370164308726493,8.7415308649783));
#37371=CARTESIAN_POINT('Ctrl Pts',(0.751838422178375,1.84878923522181,8.85271728480947));
#37372=CARTESIAN_POINT('Ctrl Pts',(-1.14622844578058,1.63384301706618,8.96390370464062));
#37373=CARTESIAN_POINT('Ctrl Pts',(-1.99430033414812,-0.077774291863319,
9.0750901244718));
#37374=CARTESIAN_POINT('Ctrl Pts',(-1.01550658722561,-1.71814696636568,
9.18627654430294));
#37375=CARTESIAN_POINT('Ctrl Pts',(0.893535233606871,-1.78462249679383,
9.29746296413412));
#37376=CARTESIAN_POINT('Ctrl Pts',(1.98406004704164,-0.216306363946107,
9.40864938396527));
#37377=CARTESIAN_POINT('Ctrl Pts',(1.2570997209806,1.55015572087487,9.51983580379645));
#37378=CARTESIAN_POINT('Ctrl Pts',(-0.621418372793996,1.8966080308943,9.63102222362759));
#37379=CARTESIAN_POINT('Ctrl Pts',(-1.93069049565776,0.50568487910749,9.74220864345877));
#37380=CARTESIAN_POINT('Ctrl Pts',(-1.47136594843111,-1.34846713542859,
9.85339506328992));
#37381=CARTESIAN_POINT('Ctrl Pts',(0.335792850651442,-1.96736556142493,
9.9645814831211));
#37382=CARTESIAN_POINT('Ctrl Pts',(1.83535233538869,-0.784070240605622,
10.0757679029522));
#37383=CARTESIAN_POINT('Ctrl Pts',(1.65364659137136,1.11746450372967,10.1869543227834));
#37384=CARTESIAN_POINT('Ctrl Pts',(-0.0428657180698079,1.99535886614283,
10.2981407426146));
#37385=CARTESIAN_POINT('Ctrl Pts',(-1.70012155281541,1.04540731136874,10.4093271624457));
#37386=CARTESIAN_POINT('Ctrl Pts',(-1.79997252133044,-0.862162458906591,
10.5205135822769));
#37387=CARTESIAN_POINT('Ctrl Pts',(-0.251008199743871,-1.97999253599851,
10.6317000021081));
#37388=CARTESIAN_POINT('Ctrl Pts',(1.52796215902707,-1.28399021223231,10.7428864219392));
#37389=CARTESIAN_POINT('Ctrl Pts',(1.90711651044001,0.588063231359589,10.8540728417704));
#37390=CARTESIAN_POINT('Ctrl Pts',(0.539529066393858,1.92169106390877,10.9652592616015));
#37391=CARTESIAN_POINT('Ctrl Pts',(-1.32278503412967,1.49446025304978,11.0764456814327));
#37392=CARTESIAN_POINT('Ctrl Pts',(-1.97242652143987,-0.300795429882017,
11.1876321012639));
#37393=CARTESIAN_POINT('Ctrl Pts',(-0.817058724297523,-1.82236293883171,
11.2988185210951));
#37394=CARTESIAN_POINT('Ctrl Pts',(1.09041866382002,-1.67090592797485,11.4100049409262));
#37395=CARTESIAN_POINT('Ctrl Pts',(1.69055718360052,-0.554926552610627,
11.4841292208136));
#37396=CARTESIAN_POINT('Ctrl Pts',(1.6883199391646,0.00672513670271936,
11.5211913607574));
#37397=CARTESIAN_POINT('Ctrl Pts',(-0.802959149489932,1.63459616787394,
-0.0766913607573554));
#37398=CARTESIAN_POINT('Ctrl Pts',(-1.34673860605774,1.36747655843322,-0.0396292208136346));
#37399=CARTESIAN_POINT('Ctrl Pts',(-2.13734155664247,0.252529773779836,
0.0344950590738073));
#37400=CARTESIAN_POINT('Ctrl Pts',(-1.36915832429422,-1.66322257224481,
0.14568147890497));
#37401=CARTESIAN_POINT('Ctrl Pts',(0.655021664869751,-2.05011034068591,
0.256867898736133));
#37402=CARTESIAN_POINT('Ctrl Pts',(2.0782545237117,-0.561654367873057,0.368054318567295));
#37403=CARTESIAN_POINT('Ctrl Pts',(1.59819640148463,1.44267659192936,0.479240738398458));
#37404=CARTESIAN_POINT('Ctrl Pts',(-0.346130996849898,2.12473254047885,
0.590427158229621));
#37405=CARTESIAN_POINT('Ctrl Pts',(-1.97325502634714,0.860819657174806,
0.701613578060782));
#37406=CARTESIAN_POINT('Ctrl Pts',(-1.79286136672128,-1.19184009808233,
0.812799997891947));
#37407=CARTESIAN_POINT('Ctrl Pts',(0.0299076046828686,-2.15261823504807,
0.923986417723108));
#37408=CARTESIAN_POINT('Ctrl Pts',(1.82526073013706,-1.14155950949091,1.03517283755427));
#37409=CARTESIAN_POINT('Ctrl Pts',(1.94860591616173,0.915246053141843,1.14635925738543));
#37410=CARTESIAN_POINT('Ctrl Pts',(0.286938251999433,2.13363139543668,1.2575456772166));
#37411=CARTESIAN_POINT('Ctrl Pts',(-1.63757451921909,1.39752576117334,1.36873209704776));
#37412=CARTESIAN_POINT('Ctrl Pts',(-2.0619994469249,-0.618778274775138,
1.47991851687892));
#37413=CARTESIAN_POINT('Ctrl Pts',(-0.597542656570052,-2.06825237330522,
1.59110493671008));
#37414=CARTESIAN_POINT('Ctrl Pts',(1.41428872795678,-1.62311872087351,1.70229135654125));
#37415=CARTESIAN_POINT('Ctrl Pts',(2.13057049201279,0.308862702088754,1.81347777637241));
#37416=CARTESIAN_POINT('Ctrl Pts',(0.895157141781652,1.95791217246742,1.92466419620357));
#37417=CARTESIAN_POINT('Ctrl Pts',(-1.16025892730732,1.81342931797682,2.03585061603473));
#37418=CARTESIAN_POINT('Ctrl Pts',(-2.15282751312695,0.00776644692787891,
2.1470370358659));
#37419=CARTESIAN_POINT('Ctrl Pts',(-1.173312682795,-1.80501078038335,2.25822345569706));
#37420=CARTESIAN_POINT('Ctrl Pts',(0.881007459369614,-1.96431984868673,
2.36940987552822));
#37421=CARTESIAN_POINT('Ctrl Pts',(2.12828655167567,-0.324226703065412,
2.48059629535939));
#37422=CARTESIAN_POINT('Ctrl Pts',(1.42596282698117,1.6128721621003,2.59178271519055));
#37423=CARTESIAN_POINT('Ctrl Pts',(-0.582604709802392,2.07251015763547,
2.70296913502171));
#37424=CARTESIAN_POINT('Ctrl Pts',(-2.05748105739819,0.633638933400953,
2.81415555485287));
#37425=CARTESIAN_POINT('Ctrl Pts',(-1.6476154945659,-1.38567304257714,2.92534197468403));
#37426=CARTESIAN_POINT('Ctrl Pts',(0.271537341065049,-2.13564839618882,
3.0365283945152));
#37427=CARTESIAN_POINT('Ctrl Pts',(1.9419501920302,-0.92927716590924,3.14771481434636));
#37428=CARTESIAN_POINT('Ctrl Pts',(1.83345241771109,1.12835226385271,3.25890123417753));
#37429=CARTESIAN_POINT('Ctrl Pts',(0.045432686513366,2.15236206769919,3.37008765400868));
#37430=CARTESIAN_POINT('Ctrl Pts',(-1.78420535659039,1.20471483967528,3.48127407383985));
#37431=CARTESIAN_POINT('Ctrl Pts',(-1.97943388729784,-0.8465034466758,3.59246049367101));
#37432=CARTESIAN_POINT('Ctrl Pts',(-0.361415101720502,-2.12228785127793,
3.70364691350217));
#37433=CARTESIAN_POINT('Ctrl Pts',(1.58767559662444,-1.45396451102085,3.81483333333334));
#37434=CARTESIAN_POINT('Ctrl Pts',(2.08238656893164,0.546253399951339,3.9260197531645));
#37435=CARTESIAN_POINT('Ctrl Pts',(0.669541102087431,2.04607949797729,4.03720617299566));
#37436=CARTESIAN_POINT('Ctrl Pts',(-1.35663306156047,1.67160800898631,4.14839259282683));
#37437=CARTESIAN_POINT('Ctrl Pts',(-2.14007248481188,-0.234128937078206,
4.25957901265799));
#37438=CARTESIAN_POINT('Ctrl Pts',(-0.963112667326238,-1.92539361935742,
4.37076543248915));
#37439=CARTESIAN_POINT('Ctrl Pts',(1.09610013699538,-1.85291421525797,4.48195185232032));
#37440=CARTESIAN_POINT('Ctrl Pts',(2.15123766275159,-0.0830850033729405,
4.59313827215147));
#37441=CARTESIAN_POINT('Ctrl Pts',(1.23574816038915,1.76285367615161,4.70432469198265));
#37442=CARTESIAN_POINT('Ctrl Pts',(-0.811740268440561,1.99394190888763,
4.8155111118138));
#37443=CARTESIAN_POINT('Ctrl Pts',(-2.11563939493572,0.398492848144611,
4.92669753164497));
#37444=CARTESIAN_POINT('Ctrl Pts',(-1.48152105102257,-1.56199294966507,
5.03788395147612));
#37445=CARTESIAN_POINT('Ctrl Pts',(0.509734849759847,-2.0916254402657,5.1490703713073));
#37446=CARTESIAN_POINT('Ctrl Pts',(2.03405151388631,-0.705238284754304,
5.26025679113844));
#37447=CARTESIAN_POINT('Ctrl Pts',(1.69508874624462,1.32717773556567,5.37144321096963));
#37448=CARTESIAN_POINT('Ctrl Pts',(-0.19664885248515,2.1438413719869,5.48262963080077));
#37449=CARTESIAN_POINT('Ctrl Pts',(-1.90824757094816,0.996653303509719,
5.59381605063195));
#37450=CARTESIAN_POINT('Ctrl Pts',(-1.87180872723762,-1.06351242967042,
5.70500247046309));
#37451=CARTESIAN_POINT('Ctrl Pts',(-0.12071188305083,-2.14945463797604,
5.81618889029427));
#37452=CARTESIAN_POINT('Ctrl Pts',(1.74096228296046,-1.26640314621194,5.92737531012542));
#37453=CARTESIAN_POINT('Ctrl Pts',(2.00783946807991,0.776728568965356,6.0385617299566));
#37454=CARTESIAN_POINT('Ctrl Pts',(0.435448592570146,2.10834321747079,6.14974814978775));
#37455=CARTESIAN_POINT('Ctrl Pts',(-1.53583208518367,1.50862401066228,6.26093456961893));
#37456=CARTESIAN_POINT('Ctrl Pts',(-2.10022394255324,-0.473060239877022,
6.37212098945007));
#37457=CARTESIAN_POINT('Ctrl Pts',(-0.74071955267899,-2.02140078749996,
6.48330740928124));
#37458=CARTESIAN_POINT('Ctrl Pts',(1.29731608273796,-1.71805051756223,6.5944938291124));
#37459=CARTESIAN_POINT('Ctrl Pts',(2.14695390376071,0.15910856216126,6.70568024894357));
#37460=CARTESIAN_POINT('Ctrl Pts',(1.02988880574655,1.89051729619815,6.81686666877473));
#37461=CARTESIAN_POINT('Ctrl Pts',(-1.03059911890458,1.89013016894061,6.92805308860589));
#37462=CARTESIAN_POINT('Ctrl Pts',(-2.14701353924984,0.158301805751674,
7.03923950843705));
#37463=CARTESIAN_POINT('Ctrl Pts',(-1.29667041186295,-1.71853787925252,
7.15042592826822));
#37464=CARTESIAN_POINT('Ctrl Pts',(0.741479067384996,-2.0211223100189,7.26161234809938));
#37465=CARTESIAN_POINT('Ctrl Pts',(2.10040155266868,-0.472271020678894,
7.37279876793055));
#37466=CARTESIAN_POINT('Ctrl Pts',(1.53526509213771,1.50920101255294,7.48398518776171));
#37467=CARTESIAN_POINT('Ctrl Pts',(-0.436240798549652,2.10817944328893,
7.59517160759286));
#37468=CARTESIAN_POINT('Ctrl Pts',(-2.00813119194563,0.775974042967894,
7.70635802742404));
#37469=CARTESIAN_POINT('Ctrl Pts',(-1.74048629299744,-1.26705724547931,
7.81754444725519));
#37470=CARTESIAN_POINT('Ctrl Pts',(0.121519559390324,-2.14940912720278,
7.92873086708636));
#37471=CARTESIAN_POINT('Ctrl Pts',(1.87220822337856,-1.06280899870737,8.03991728691751));
#37472=CARTESIAN_POINT('Ctrl Pts',(1.90787293110882,0.997370281398245,8.15110370674869));
#37473=CARTESIAN_POINT('Ctrl Pts',(0.195843262983046,2.1439151139204,8.26229012657984));
#37474=CARTESIAN_POINT('Ctrl Pts',(-1.69558733042143,1.32654069078969,8.37347654641101));
#37475=CARTESIAN_POINT('Ctrl Pts',(-2.03378636810517,-0.706002555693802,
8.48466296624217));
#37476=CARTESIAN_POINT('Ctrl Pts',(-0.508948858861673,-2.09181683182873,
8.59584938607333));
#37477=CARTESIAN_POINT('Ctrl Pts',(1.48210788489943,-1.56143613926181,8.70703580590451));
#37478=CARTESIAN_POINT('Ctrl Pts',(2.11548950721726,0.399287798761521,8.81822222573564));
#37479=CARTESIAN_POINT('Ctrl Pts',(0.810990961415923,1.99424678906897,8.92940864556684));
#37480=CARTESIAN_POINT('Ctrl Pts',(-1.23641048638147,1.76238920508216,9.04059506539797));
#37481=CARTESIAN_POINT('Ctrl Pts',(-2.15120629331062,-0.0838933551026959,
9.15178148522916));
#37482=CARTESIAN_POINT('Ctrl Pts',(-1.09540379848118,-1.85332595276186,
9.26296790506031));
#37483=CARTESIAN_POINT('Ctrl Pts',(0.963836080712942,-1.9250315915564,9.37415432489147));
#37484=CARTESIAN_POINT('Ctrl Pts',(2.14016032912378,-0.233324742234878,
9.48534074472264));
#37485=CARTESIAN_POINT('Ctrl Pts',(1.35600480268067,1.67211762704833,9.5965271645538));
#37486=CARTESIAN_POINT('Ctrl Pts',(-0.67030982818557,2.04582783352242,9.70771358438496));
#37487=CARTESIAN_POINT('Ctrl Pts',(-2.08259181106143,0.545470747680921,
9.81890000421612));
#37488=CARTESIAN_POINT('Ctrl Pts',(-1.58712889620009,-1.45456074914393,
9.93008642404728));
#37489=CARTESIAN_POINT('Ctrl Pts',(0.362212090727357,-2.12215236818265,
10.0412728438785));
#37490=CARTESIAN_POINT('Ctrl Pts',(1.97975271162804,-0.845758688953388,
10.1524592637096));
#37491=CARTESIAN_POINT('Ctrl Pts',(1.78375086909329,1.20538347801125,10.2636456835408));
#37492=CARTESIAN_POINT('Ctrl Pts',(-0.0462382725911752,2.15234810763501,
10.3748321033719));
#37493=CARTESIAN_POINT('Ctrl Pts',(-1.83388235020868,1.12765702777161,10.4860185232031));
#37494=CARTESIAN_POINT('Ctrl Pts',(-1.94158931298892,-0.929994984054507,
10.5972049430343));
#37495=CARTESIAN_POINT('Ctrl Pts',(-0.270756821184746,-2.13577279771527,
10.7083913628654));
#37496=CARTESIAN_POINT('Ctrl Pts',(1.64817793797518,-1.38501096239512,10.8195777826966));
#37497=CARTESIAN_POINT('Ctrl Pts',(2.0571630907777,0.634330397736036,10.9307642025277));
#37498=CARTESIAN_POINT('Ctrl Pts',(0.58197770073898,2.07288432925282,11.0419506223589));
#37499=CARTESIAN_POINT('Ctrl Pts',(-1.42685805211597,1.61204019596003,11.1531370421901));
#37500=CARTESIAN_POINT('Ctrl Pts',(-2.12761151034289,-0.324461171008946,
11.2643234620212));
#37501=CARTESIAN_POINT('Ctrl Pts',(-0.881342614057178,-1.96574134576644,
11.3755098818524));
#37502=CARTESIAN_POINT('Ctrl Pts',(1.17620974724197,-1.80236812191326,11.4866963016836));
#37503=CARTESIAN_POINT('Ctrl Pts',(1.82356548323819,-0.598586618003602,
11.560820581571));
#37504=CARTESIAN_POINT('Ctrl Pts',(1.82115221868229,0.00725425160419088,
11.5978827215147));
#37505=CARTESIAN_POINT('Ctrl Pts',(-0.861525859670525,1.75382131162755,
-1.38777878078145E-16));
#37506=CARTESIAN_POINT('Ctrl Pts',(-1.44496782441849,1.46721837385112,0.0370621399437207));
#37507=CARTESIAN_POINT('Ctrl Pts',(-2.29323624142731,0.270948940037977,
0.111186419831162));
#37508=CARTESIAN_POINT('Ctrl Pts',(-1.4690228053469,-1.78453568564088,0.222372839662325));
#37509=CARTESIAN_POINT('Ctrl Pts',(0.702798023147504,-2.19964250335881,
0.333559259493488));
#37510=CARTESIAN_POINT('Ctrl Pts',(2.22983948348091,-0.602620646924488,
0.44474567932465));
#37511=CARTESIAN_POINT('Ctrl Pts',(1.71476659751129,1.54790339194469,0.555932099155814));
#37512=CARTESIAN_POINT('Ctrl Pts',(-0.371377304572895,2.2797075413722,0.667118518986976));
#37513=CARTESIAN_POINT('Ctrl Pts',(-2.11718147056775,0.923606631345987,
0.778304938818138));
#37514=CARTESIAN_POINT('Ctrl Pts',(-1.92363015131696,-1.2787712372945,0.889491358649302));
#37515=CARTESIAN_POINT('Ctrl Pts',(0.0320890232727887,-2.30962717925356,
1.00067777848046));
#37516=CARTESIAN_POINT('Ctrl Pts',(1.95839267869742,-1.22482325334233,1.11186419831163));
#37517=CARTESIAN_POINT('Ctrl Pts',(2.09073448897961,0.982002812028443,1.22305061814279));
#37518=CARTESIAN_POINT('Ctrl Pts',(0.3078671242282,2.28925546628532,1.33423703797395));
#37519=CARTESIAN_POINT('Ctrl Pts',(-1.75701689972769,1.49945932314417,1.44542345780511));
#37520=CARTESIAN_POINT('Ctrl Pts',(-2.21239878427269,-0.663911091192784,
1.55660987763628));
#37521=CARTESIAN_POINT('Ctrl Pts',(-0.641126576885465,-2.21910779030204,
1.66779629746744));
#37522=CARTESIAN_POINT('Ctrl Pts',(1.51744495713052,-1.74150671579767,1.7789827172986));
#37523=CARTESIAN_POINT('Ctrl Pts',(2.28597130487397,0.331390712847842,1.89016913712977));
#37524=CARTESIAN_POINT('Ctrl Pts',(0.960448643749269,2.10071953052146,2.00135555696093));
#37525=CARTESIAN_POINT('Ctrl Pts',(-1.24488658037438,1.94569829998722,2.11254197679209));
#37526=CARTESIAN_POINT('Ctrl Pts',(-2.30985172178094,0.00833292063536468,
2.22372839662325));
#37527=CARTESIAN_POINT('Ctrl Pts',(-1.2588924584139,-1.93666572611094,2.33491481645442));
#37528=CARTESIAN_POINT('Ctrl Pts',(0.945266903418065,-2.10759457362527,
2.44610123628558));
#37529=CARTESIAN_POINT('Ctrl Pts',(2.28352077714336,-0.347875342430591,
2.55728765611674));
#37530=CARTESIAN_POINT('Ctrl Pts',(1.52997054850621,1.73051278744978,2.6684740759479));
#37531=CARTESIAN_POINT('Ctrl Pts',(-0.625099077306038,2.22367613142842,
2.77966049577907));
#37532=CARTESIAN_POINT('Ctrl Pts',(-2.20755082977362,0.679855665342084,
2.89084691561023));
#37533=CARTESIAN_POINT('Ctrl Pts',(-1.76779024968342,-1.48674208393651,
3.00203333544139));
#37534=CARTESIAN_POINT('Ctrl Pts',(0.291342892527361,-2.29141958423335,
3.11321975527256));
#37535=CARTESIAN_POINT('Ctrl Pts',(2.08359330569799,-0.997057334412016,
3.22440617510372));
#37536=CARTESIAN_POINT('Ctrl Pts',(1.96718185643314,1.21065268979674,3.33559259493488));
#37537=CARTESIAN_POINT('Ctrl Pts',(0.0487464827201324,2.30935232741881,
3.44677901476604));
#37538=CARTESIAN_POINT('Ctrl Pts',(-1.91434278399063,1.29258504441778,3.55796543459721));
#37539=CARTESIAN_POINT('Ctrl Pts',(-2.12381100893932,-0.908246216603541,
3.66915185442837));
#37540=CARTESIAN_POINT('Ctrl Pts',(-0.38777621054007,-2.27708453998192,
3.78033827425954));
#37541=CARTESIAN_POINT('Ctrl Pts',(1.70347841995286,-1.56001463596674,3.89152469409069));
#37542=CARTESIAN_POINT('Ctrl Pts',(2.23427291426326,0.58609635407974,4.00271111392186));
#37543=CARTESIAN_POINT('Ctrl Pts',(0.718376487679439,2.19531765665651,4.11389753375301));
#37544=CARTESIAN_POINT('Ctrl Pts',(-1.45558396757891,1.79353274433565,4.22508395358419));
#37545=CARTESIAN_POINT('Ctrl Pts',(-2.29616635965357,-0.251205972206891,
4.33627037341534));
#37546=CARTESIAN_POINT('Ctrl Pts',(-1.03336074967814,-2.06582911991821,
4.44745679324651));
#37547=CARTESIAN_POINT('Ctrl Pts',(1.17604813820203,-1.98806317010017,4.55864321307767));
#37548=CARTESIAN_POINT('Ctrl Pts',(2.30814590995695,-0.0891451065749571,
4.66982963290884));
#37549=CARTESIAN_POINT('Ctrl Pts',(1.32588189186442,1.89143374203362,4.78101605273999));
#37550=CARTESIAN_POINT('Ctrl Pts',(-0.870947461077787,2.1393772252035,4.89220247257116));
#37551=CARTESIAN_POINT('Ctrl Pts',(-2.26995115459196,0.427558355600586,
5.00338889240232));
#37552=CARTESIAN_POINT('Ctrl Pts',(-1.58958111120973,-1.67592251687317,
5.11457531223348));
#37553=CARTESIAN_POINT('Ctrl Pts',(0.546914192237968,-2.24418565586851,
5.22576173206465));
#37554=CARTESIAN_POINT('Ctrl Pts',(2.1824123683356,-0.756677372605439,5.33694815189581));
#37555=CARTESIAN_POINT('Ctrl Pts',(1.81872613351991,1.4239802115651,5.44813457172697));
#37556=CARTESIAN_POINT('Ctrl Pts',(-0.210992142997687,2.30021014415434,
5.55932099155813));
#37557=CARTESIAN_POINT('Ctrl Pts',(-2.04743246287144,1.06934779265563,5.67050741138931));
#37558=CARTESIAN_POINT('Ctrl Pts',(-2.00833582118916,-1.14108352937273,
5.78169383122044));
#37559=CARTESIAN_POINT('Ctrl Pts',(-0.129516437895867,-2.30623283386393,
5.89288025105164));
#37560=CARTESIAN_POINT('Ctrl Pts',(1.86794562143574,-1.35877280920554,6.00406667088277));
#37561=CARTESIAN_POINT('Ctrl Pts',(2.15428845280213,0.83338205752262,6.11525309071395));
#37562=CARTESIAN_POINT('Ctrl Pts',(0.467209600008474,2.26212280421227,6.22643951054511));
#37563=CARTESIAN_POINT('Ctrl Pts',(-1.64785351575852,1.61866092257753,6.33762593037627));
#37564=CARTESIAN_POINT('Ctrl Pts',(-2.25341132081031,-0.507564587930634,
6.44881235020743));
#37565=CARTESIAN_POINT('Ctrl Pts',(-0.794746594271866,-2.1688389157728,
6.55999877003859));
#37566=CARTESIAN_POINT('Ctrl Pts',(1.39194049181108,-1.84336270411821,6.67118518986976));
#37567=CARTESIAN_POINT('Ctrl Pts',(2.30354969961477,0.170713716736379,6.78237160970093));
#37568=CARTESIAN_POINT('Ctrl Pts',(1.1050074456459,2.02840896683692,6.89355802953208));
#37569=CARTESIAN_POINT('Ctrl Pts',(-1.10576956804586,2.02799360306213,7.00474444936325));
#37570=CARTESIAN_POINT('Ctrl Pts',(-2.30361368483253,0.169848116649841,
7.11593086919441));
#37571=CARTESIAN_POINT('Ctrl Pts',(-1.39124772661127,-1.84388561328419,
7.22711728902557));
#37572=CARTESIAN_POINT('Ctrl Pts',(0.795561506911461,-2.16854012653626,
7.33830370885674));
#37573=CARTESIAN_POINT('Ctrl Pts',(2.25360188555757,-0.506717804195071,
7.44949012868789));
#37574=CARTESIAN_POINT('Ctrl Pts',(1.64724516703786,1.61928001017393,7.56067654851907));
#37575=CARTESIAN_POINT('Ctrl Pts',(-0.468059588377044,2.26194708457211,
7.67186296835021));
#37576=CARTESIAN_POINT('Ctrl Pts',(-2.154601454596,0.832572497460946,7.78304938818139));
#37577=CARTESIAN_POINT('Ctrl Pts',(-1.8674349134348,-1.35947461755279,7.89423580801255));
#37578=CARTESIAN_POINT('Ctrl Pts',(0.130383025010703,-2.30618400359892,
8.00542222784371));
#37579=CARTESIAN_POINT('Ctrl Pts',(2.00876445601631,-1.14032879114536,8.11660864767487));
#37580=CARTESIAN_POINT('Ctrl Pts',(2.04703049732954,1.07011706590215,8.22779506750604));
#37581=CARTESIAN_POINT('Ctrl Pts',(0.210127794931219,2.30028926472067,8.3389814873372));
#37582=CARTESIAN_POINT('Ctrl Pts',(-1.81926108372479,1.42329670163983,8.45016790716836));
#37583=CARTESIAN_POINT('Ctrl Pts',(-2.18212788319439,-0.757497388391501,
8.56135432699953));
#37584=CARTESIAN_POINT('Ctrl Pts',(-0.546070872270014,-2.24439100726275,
8.67254074683069));
#37585=CARTESIAN_POINT('Ctrl Pts',(1.59021074792356,-1.67532509350284,8.78372716666185));
#37586=CARTESIAN_POINT('Ctrl Pts',(2.26979033427429,0.428411288796547,8.89491358649301));
#37587=CARTESIAN_POINT('Ctrl Pts',(0.870143500653468,2.13970434291613,9.00610000632417));
#37588=CARTESIAN_POINT('Ctrl Pts',(-1.32659252698235,1.89093539309814,9.11728642615534));
#37589=CARTESIAN_POINT('Ctrl Pts',(-2.30811225247311,-0.0900124183420705,
9.2284728459865));
#37590=CARTESIAN_POINT('Ctrl Pts',(-1.17530100973675,-1.98850493915805,
9.33965926581767));
#37591=CARTESIAN_POINT('Ctrl Pts',(1.03413692781901,-2.06544068631896,9.45084568564882));
#37592=CARTESIAN_POINT('Ctrl Pts',(2.29626061120593,-0.250343120523647,
9.56203210547999));
#37593=CARTESIAN_POINT('Ctrl Pts',(1.45490988438074,1.79407953322179,9.67321852531115));
#37594=CARTESIAN_POINT('Ctrl Pts',(-0.719201283577143,2.19504763615053,
9.78440494514231));
#37595=CARTESIAN_POINT('Ctrl Pts',(-2.2344931264651,0.585256616254353,9.89559136497349));
#37596=CARTESIAN_POINT('Ctrl Pts',(-1.70289184396906,-1.56065436285928,
10.0067777848046));
#37597=CARTESIAN_POINT('Ctrl Pts',(0.388631330803272,-2.27693917494037,
10.1179642046358));
#37598=CARTESIAN_POINT('Ctrl Pts',(2.1241530878674,-0.907447137301155,10.229150624467));
#37599=CARTESIAN_POINT('Ctrl Pts',(1.91385514681521,1.29330245229283,10.3403370442981));
#37600=CARTESIAN_POINT('Ctrl Pts',(-0.0496108271125438,2.30933734912719,
10.4515234641293));
#37601=CARTESIAN_POINT('Ctrl Pts',(-1.96764314760194,1.20990674417448,10.5627098839605));
#37602=CARTESIAN_POINT('Ctrl Pts',(-2.08320610464741,-0.997827509202423,
10.6738963037916));
#37603=CARTESIAN_POINT('Ctrl Pts',(-0.290505442625618,-2.29155305943203,
10.7850827236228));
#37604=CARTESIAN_POINT('Ctrl Pts',(1.7683937169233,-1.48603171255794,10.8962691434539));
#37605=CARTESIAN_POINT('Ctrl Pts',(2.20720967111538,0.680597564112484,11.0074555632851));
#37606=CARTESIAN_POINT('Ctrl Pts',(0.624426335084105,2.22407759459687,11.1186419831163));
#37607=CARTESIAN_POINT('Ctrl Pts',(-1.53093107010227,1.72962013887028,11.2298284029474));
#37608=CARTESIAN_POINT('Ctrl Pts',(-2.28279649924591,-0.348126912135875,
11.3410148227786));
#37609=CARTESIAN_POINT('Ctrl Pts',(-0.945626503816835,-2.10911975270116,
11.4522012426097));
#37610=CARTESIAN_POINT('Ctrl Pts',(1.26200083066393,-1.93383031585166,11.5633876624409));
#37611=CARTESIAN_POINT('Ctrl Pts',(1.95657378287586,-0.642246683396576,
11.6375119423284));
#37612=CARTESIAN_POINT('Ctrl Pts',(1.95398449819998,0.0077833665056624,
11.6745740822721));
#37613=CARTESIAN_POINT('Ctrl Pts',(-1.95093054978418,-0.000550606481354719,
10.6241303078758));
#37614=CARTESIAN_POINT('Ctrl Pts',(-1.95166977968097,-0.292567552961119,
10.640718973181));
#37615=CARTESIAN_POINT('Ctrl Pts',(-1.89027401228485,-0.584289311968449,
10.6573076384863));
#37616=CARTESIAN_POINT('Ctrl Pts',(-1.7651621681362,-0.845492725344543,
10.6738963037916));
#37617=CARTESIAN_POINT('Ctrl Pts',(-1.48563921730681,-1.42906935927896,
10.7109584437353));
#37618=CARTESIAN_POINT('Ctrl Pts',(-0.888072329966215,-1.8603112093555,
10.7480205836791));
#37619=CARTESIAN_POINT('Ctrl Pts',(-0.246139026371096,-1.94167857658142,
10.7850827236228));
#37620=CARTESIAN_POINT('Ctrl Pts',(0.395794277224022,-2.02304594380734,
10.8221448635665));
#37621=CARTESIAN_POINT('Ctrl Pts',(1.08209399707366,-1.75453882818264,10.8592070035102));
#37622=CARTESIAN_POINT('Ctrl Pts',(1.49837984936383,-1.25918039092522,10.8962691434539));
#37623=CARTESIAN_POINT('Ctrl Pts',(1.91466570165399,-0.763821953667804,
10.9333312833977));
#37624=CARTESIAN_POINT('Ctrl Pts',(2.06093768638468,-0.041612194777677,
10.9703934233414));
#37625=CARTESIAN_POINT('Ctrl Pts',(1.87027645607817,0.576739356414784,11.0074555632851));
#37626=CARTESIAN_POINT('Ctrl Pts',(1.80418088670294,0.791100177355746,11.0203037088567));
#37627=CARTESIAN_POINT('Ctrl Pts',(1.69759382901609,0.992979671982257,11.0331518544284));
#37628=CARTESIAN_POINT('Ctrl Pts',(1.56057659382855,1.17255425406022,11.046));
#37629=CARTESIAN_POINT('Ctrl Pts',(-0.9055496143049,-1.2679201530598,4.59701721133854E-17));
#37630=CARTESIAN_POINT('Ctrl Pts',(-0.937460871048188,-1.25085822491965,
4.11134559556874E-17));
#37631=CARTESIAN_POINT('Ctrl Pts',(-0.968677330061127,-1.23263760516135,
2.44937731663795E-16));
#37632=CARTESIAN_POINT('Ctrl Pts',(-0.999128467894991,-1.21327242330634,
1.95156391047391E-16));
#37633=CARTESIAN_POINT('Ctrl Pts',(-1.04916478169554,-1.18145218981002,
1.19833509668E-16));
#37634=CARTESIAN_POINT('Ctrl Pts',(-1.09713600671012,-1.14654455097205,
1.20483738925504E-16));
#37635=CARTESIAN_POINT('Ctrl Pts',(-1.14296368523792,-1.10887020140839,
3.46944695195361E-17));
#37636=CARTESIAN_POINT('Ctrl Pts',(-1.1691715546085,-1.08732504652154,-1.4366579135275E-17));
#37637=CARTESIAN_POINT('Ctrl Pts',(-1.19467812556179,-1.06487409533188,
1.54611493479508E-16));
#37638=CARTESIAN_POINT('Ctrl Pts',(-1.21946596262297,-1.04157045589269,
1.28369537222284E-16));
#37639=CARTESIAN_POINT('Ctrl Pts',(-1.23288807387334,-1.02895200756582,
1.14160049906282E-16));
#37640=CARTESIAN_POINT('Ctrl Pts',(-1.24610308792281,-1.01607950194371,
2.35779340588765E-16));
#37641=CARTESIAN_POINT('Ctrl Pts',(-1.25908578368524,-1.0029839550804,2.28983498828939E-16));
#37642=CARTESIAN_POINT('Ctrl Pts',(-1.30296735026586,-0.95872095130156,
2.06013524941215E-16));
#37643=CARTESIAN_POINT('Ctrl Pts',(-1.34424080059494,-0.911874911049719,
3.41092537496216E-16));
#37644=CARTESIAN_POINT('Ctrl Pts',(-1.3828175432908,-0.862794893107178,
2.15105711021124E-16));
#37645=CARTESIAN_POINT('Ctrl Pts',(-1.41246270387874,-0.825078255778903,
1.18288316865636E-16));
#37646=CARTESIAN_POINT('Ctrl Pts',(-1.44051505756546,-0.786041114269597,
-3.41744083773187E-17));
#37647=CARTESIAN_POINT('Ctrl Pts',(-1.46692433972057,-0.745823635123971,
-2.77555756156289E-17));
#37648=CARTESIAN_POINT('Ctrl Pts',(-1.479951210132,-0.725985614308893,-2.45893667770833E-17));
#37649=CARTESIAN_POINT('Ctrl Pts',(-1.49257814628919,-0.705860181165347,
1.12314029669873E-16));
#37650=CARTESIAN_POINT('Ctrl Pts',(-1.50479813274716,-0.685463000140721,
1.31838984174237E-16));
#37651=CARTESIAN_POINT('Ctrl Pts',(-1.51107691151866,-0.674982678607113,
1.41871145034493E-16));
#37652=CARTESIAN_POINT('Ctrl Pts',(-1.51724344631134,-0.664438579506566,
2.39743182585592E-16));
#37653=CARTESIAN_POINT('Ctrl Pts',(-1.52329612440982,-0.653835068968427,
2.42861286636753E-16));
#37654=CARTESIAN_POINT('Ctrl Pts',(-1.55541704658302,-0.597563360607725,
2.59408734877987E-16));
#37655=CARTESIAN_POINT('Ctrl Pts',(-1.58434358367058,-0.539605423501723,
2.32306933354682E-17));
#37656=CARTESIAN_POINT('Ctrl Pts',(-1.60998194797531,-0.480314579840224,
1.38777878078145E-17));
#37657=CARTESIAN_POINT('Ctrl Pts',(-1.63611695660561,-0.419875204988797,
4.34370584461709E-18));
#37658=CARTESIAN_POINT('Ctrl Pts',(-1.65883591999594,-0.358049987819819,
-3.99522282745635E-16));
#37659=CARTESIAN_POINT('Ctrl Pts',(-1.67800508733892,-0.295172269836945,
-4.02455846426619E-16));
#37660=CARTESIAN_POINT('Ctrl Pts',(-1.69036857863681,-0.254618180804147,
-4.04347899868101E-16));
#37661=CARTESIAN_POINT('Ctrl Pts',(-1.70125468815875,-0.21362546632645,
2.10692284276142E-16));
#37662=CARTESIAN_POINT('Ctrl Pts',(-1.71061789501208,-0.172277279535232,
2.22044604925031E-16));
#37663=CARTESIAN_POINT('Ctrl Pts',(-1.71585060492304,-0.149169484288187,
2.28388948449886E-16));
#37664=CARTESIAN_POINT('Ctrl Pts',(-1.72060753217063,-0.125950592727189,
-7.81124113857471E-17));
#37665=CARTESIAN_POINT('Ctrl Pts',(-1.72487954070067,-0.102634681883505,
-6.93889390390723E-17));
#37666=CARTESIAN_POINT('Ctrl Pts',(-1.72700542719079,-0.0910319475914671,
-6.50478634353357E-17));
#37667=CARTESIAN_POINT('Ctrl Pts',(-1.7290114810898,-0.0794035343790101,
3.2530658909822E-16));
#37668=CARTESIAN_POINT('Ctrl Pts',(-1.73089565945358,-0.0677563287869385,
3.05311331771918E-16));
#37669=CARTESIAN_POINT('Ctrl Pts',(-1.74172479313661,-0.000815136373784872,
1.90390516006322E-16));
#37670=CARTESIAN_POINT('Ctrl Pts',(-1.74848828323664,0.0664709663887247,
1.66332759660732E-17));
#37671=CARTESIAN_POINT('Ctrl Pts',(-1.75106678678907,0.133744024330042,
0.));
#37672=CARTESIAN_POINT('Ctrl Pts',(-1.75197767455289,0.157509050853062,
-5.87590718476407E-18));
#37673=CARTESIAN_POINT('Ctrl Pts',(-1.75236592486458,0.181272742240003,
-1.43574718418596E-16));
#37674=CARTESIAN_POINT('Ctrl Pts',(-1.75222496230419,0.20502014676713,-1.52655665885959E-16));
#37675=CARTESIAN_POINT('Ctrl Pts',(-1.75184009030703,0.269858008556557,
-1.89868827307373E-16));
#37676=CARTESIAN_POINT('Ctrl Pts',(-1.74751402866387,0.334573792851957,
-3.30194805135327E-16));
#37677=CARTESIAN_POINT('Ctrl Pts',(-1.7394637798186,0.398932034828451,-3.60822483003176E-16));
#37678=CARTESIAN_POINT('Ctrl Pts',(-1.73512917103287,0.433585348839861,
-3.77313774654407E-16));
#37679=CARTESIAN_POINT('Ctrl Pts',(-1.72971393872322,0.468135193807322,
-2.30290250750647E-16));
#37680=CARTESIAN_POINT('Ctrl Pts',(-1.72324590502527,0.502545438383202,
-2.22044604925031E-16));
#37681=CARTESIAN_POINT('Ctrl Pts',(-1.71875224847293,0.526451903350239,
-2.16315955056648E-16));
#37682=CARTESIAN_POINT('Ctrl Pts',(-1.71375034317529,0.550290993458765,
-1.09112752506388E-16));
#37683=CARTESIAN_POINT('Ctrl Pts',(-1.70824837476028,0.574050543226345,
-1.11022302462516E-16));
#37684=CARTESIAN_POINT('Ctrl Pts',(-1.70556019910987,0.585659087356796,
-1.11955278682682E-16));
#37685=CARTESIAN_POINT('Ctrl Pts',(-1.70275214211861,0.597250589985584,
-1.86923780482983E-17));
#37686=CARTESIAN_POINT('Ctrl Pts',(-1.69982665236451,0.608817432227434,
-2.77555756156289E-17));
#37687=CARTESIAN_POINT('Ctrl Pts',(-1.68323412399998,0.674421202576402,
-7.91594003935956E-17));
#37688=CARTESIAN_POINT('Ctrl Pts',(-1.6629277813761,0.739001412074313,-4.05964646411352E-16));
#37689=CARTESIAN_POINT('Ctrl Pts',(-1.63916833994428,0.802303176749866,
-3.88578058618805E-16));
#37690=CARTESIAN_POINT('Ctrl Pts',(-1.61488642929252,0.866996944840365,
-3.70809140417215E-16));
#37691=CARTESIAN_POINT('Ctrl Pts',(-1.58699772603761,0.930356288581554,
-4.09457680297508E-17));
#37692=CARTESIAN_POINT('Ctrl Pts',(-1.55572518982035,0.992113582996803,
0.));
#37693=CARTESIAN_POINT('Ctrl Pts',(-1.52416508821539,1.05443876420538,4.13222832434933E-17));
#37694=CARTESIAN_POINT('Ctrl Pts',(-1.48915832892389,1.11513327578217,-2.91589739144645E-16));
#37695=CARTESIAN_POINT('Ctrl Pts',(-1.45088203376165,1.17391247934435,-2.77555756156289E-16));
#37696=CARTESIAN_POINT('Ctrl Pts',(-1.43586030613212,1.19698067814596,-2.72048047818399E-16));
#37697=CARTESIAN_POINT('Ctrl Pts',(-1.42033446520901,1.21975369583959,-2.46829292445535E-16));
#37698=CARTESIAN_POINT('Ctrl Pts',(-1.40431321996707,1.24221341255695,-2.22044604925031E-16));
#37699=CARTESIAN_POINT('Ctrl Pts',(-1.39827097600966,1.25068385824148,-2.12697320981403E-16));
#37700=CARTESIAN_POINT('Ctrl Pts',(-1.39215941512485,1.25910802930607,-2.5395452896005E-16));
#37701=CARTESIAN_POINT('Ctrl Pts',(-1.38598454691313,1.26747777400967,-2.4980018054066E-16));
#37702=CARTESIAN_POINT('Ctrl Pts',(-1.3431243018081,1.32557282918544,-2.20964521964367E-16));
#37703=CARTESIAN_POINT('Ctrl Pts',(-1.29714727100707,1.38114651172693,8.67497813555755E-17));
#37704=CARTESIAN_POINT('Ctrl Pts',(-1.24829449348075,1.43391808714502,5.55111512312578E-17));
#37705=CARTESIAN_POINT('Ctrl Pts',(-1.19933005104754,1.48681028483588,2.42011176187261E-17));
#37706=CARTESIAN_POINT('Ctrl Pts',(-1.14747626839011,1.53688856046327,-1.29713890200027E-16));
#37707=CARTESIAN_POINT('Ctrl Pts',(-1.09292624810297,1.58385401467225,-2.77555756156289E-17));
#37708=CARTESIAN_POINT('Ctrl Pts',(-1.03954323648884,1.62981471962349,7.20215071969156E-17));
#37709=CARTESIAN_POINT('Ctrl Pts',(-0.983577547054738,1.67279522220595,
1.33536308196711E-16));
#37710=CARTESIAN_POINT('Ctrl Pts',(-0.92517040004714,1.71248622994896,1.66533453693773E-16));
#37711=CARTESIAN_POINT('Ctrl Pts',(-0.904266808925204,1.72669141954621,
1.78342947445829E-16));
#37712=CARTESIAN_POINT('Ctrl Pts',(-0.883050159709791,1.74047492561567,
-1.31748417511445E-16));
#37713=CARTESIAN_POINT('Ctrl Pts',(-0.861525859670525,1.75382131162755,
-1.38777878078145E-16));
#37714=CARTESIAN_POINT('Origin',(0.,0.,0.));
#37715=CARTESIAN_POINT('Origin',(-0.866025403784439,-1.5,-4.));
#37716=CARTESIAN_POINT('',(-0.866025403784439,-1.5,-4.));
#37717=CARTESIAN_POINT('',(0.866025403784439,-1.5,-4.));
#37718=CARTESIAN_POINT('',(-0.43301270189222,-1.5,-4.));
#37719=CARTESIAN_POINT('',(-0.866025403784439,-1.5,-2.));
#37720=CARTESIAN_POINT('',(-0.866025403784439,-1.5,-4.));
#37721=CARTESIAN_POINT('',(0.866025403784439,-1.5,-2.));
#37722=CARTESIAN_POINT('',(-0.866025403784439,-1.5,-2.));
#37723=CARTESIAN_POINT('',(0.866025403784439,-1.5,-4.));
#37724=CARTESIAN_POINT('Origin',(-1.73205080756888,2.12115047744981E-16,
-4.));
#37725=CARTESIAN_POINT('',(-1.73205080756888,2.12115047744981E-16,-4.));
#37726=CARTESIAN_POINT('',(-1.51554445662277,-0.375,-4.));
#37727=CARTESIAN_POINT('',(-1.73205080756888,2.77555756156289E-16,-2.));
#37728=CARTESIAN_POINT('',(-1.73205080756888,2.12115047744981E-16,-4.));
#37729=CARTESIAN_POINT('',(-1.73205080756888,2.12115047744981E-16,-2.));
#37730=CARTESIAN_POINT('Origin',(-0.866025403784438,1.5,-4.));
#37731=CARTESIAN_POINT('',(-0.866025403784438,1.5,-4.));
#37732=CARTESIAN_POINT('',(-1.08253175473055,1.125,-4.));
#37733=CARTESIAN_POINT('',(-0.866025403784438,1.5,-2.));
#37734=CARTESIAN_POINT('',(-0.866025403784438,1.5,-4.));
#37735=CARTESIAN_POINT('',(-0.866025403784438,1.5,-2.));
#37736=CARTESIAN_POINT('Origin',(0.866025403784439,1.5,-4.));
#37737=CARTESIAN_POINT('',(0.866025403784439,1.5,-4.));
#37738=CARTESIAN_POINT('',(0.43301270189222,1.5,-4.));
#37739=CARTESIAN_POINT('',(0.866025403784439,1.5,-2.));
#37740=CARTESIAN_POINT('',(0.866025403784439,1.5,-4.));
#37741=CARTESIAN_POINT('',(0.866025403784439,1.5,-2.));
#37742=CARTESIAN_POINT('Origin',(1.73205080756888,0.,-4.));
#37743=CARTESIAN_POINT('',(1.73205080756888,0.,-4.));
#37744=CARTESIAN_POINT('',(1.51554445662277,0.375,-4.));
#37745=CARTESIAN_POINT('',(1.73205080756888,0.,-2.));
#37746=CARTESIAN_POINT('',(1.73205080756888,0.,-4.));
#37747=CARTESIAN_POINT('',(1.73205080756888,0.,-2.));
#37748=CARTESIAN_POINT('Origin',(0.866025403784439,-1.5,-4.));
#37749=CARTESIAN_POINT('',(1.08253175473055,-1.125,-4.));
#37750=CARTESIAN_POINT('',(0.866025403784439,-1.5,-2.));
#37751=CARTESIAN_POINT('Origin',(0.,2.77555756156289E-16,-2.));
#37752=CARTESIAN_POINT('Origin',(0.,0.,0.));
#37753=CARTESIAN_POINT('',(-3.5,-4.28626379701574E-16,0.));
#37754=CARTESIAN_POINT('Origin',(0.,0.,0.));
#37755=CARTESIAN_POINT('Origin',(0.,0.,-4.));
#37756=CARTESIAN_POINT('',(-3.5,-4.28626379701574E-16,-4.));
#37757=CARTESIAN_POINT('',(-3.5,-4.28626379701574E-16,-4.));
#37758=CARTESIAN_POINT('Origin',(0.,0.,-4.));
#37759=CARTESIAN_POINT('Origin',(0.,0.,-4.));
#37760=CARTESIAN_POINT('Origin',(0.,0.,12.));
#37761=CARTESIAN_POINT('',(0.,0.,0.));
#37762=CARTESIAN_POINT('Origin',(0.,0.,0.));
#37763=CARTESIAN_POINT('',(-2.94437861999191,0.00228824954296311,0.322176117089596));
#37764=CARTESIAN_POINT('',(-2.94436911647834,0.00312614869137163,0.177823882910396));
#37765=CARTESIAN_POINT('',(-2.942,-3.60291088309151E-16,0.));
#37766=CARTESIAN_POINT('',(1.28892185405323,2.64462557919717,0.));
#37767=CARTESIAN_POINT('Ctrl Pts',(-2.94437861999191,0.00228824954296311,
0.322176117089596));
#37768=CARTESIAN_POINT('Ctrl Pts',(-2.94551635113874,0.142778583613822,
0.314557432409286));
#37769=CARTESIAN_POINT('Ctrl Pts',(-2.93631267309395,0.283111895578672,
0.306938747728977));
#37770=CARTESIAN_POINT('Ctrl Pts',(-2.91624915612822,0.42186500989966,0.299320063048668));
#37771=CARTESIAN_POINT('Ctrl Pts',(-2.77830971889191,1.37581174500659,0.246940558544163));
#37772=CARTESIAN_POINT('Ctrl Pts',(-2.1270526803082,2.25506646395135,0.194561054039658));
#37773=CARTESIAN_POINT('Ctrl Pts',(-1.25475282359973,2.66583045735473,0.142181549535154));
#37774=CARTESIAN_POINT('Ctrl Pts',(-0.46548135530728,3.03749657388775,0.0947876996901026));
#37775=CARTESIAN_POINT('Ctrl Pts',(0.504756374147381,3.02561249996607,0.0473938498450515));
#37776=CARTESIAN_POINT('Ctrl Pts',(1.29197400994443,2.64783394680711,3.05745012640912E-16));
#37777=CARTESIAN_POINT('',(-1.28892185405326,2.64462557919716,0.));
#37778=CARTESIAN_POINT('Origin',(0.,0.,0.));
#37779=CARTESIAN_POINT('Ctrl Pts',(-1.28892185405326,2.64462557919716,1.87350135405495E-15));
#37780=CARTESIAN_POINT('Ctrl Pts',(-2.16038499609478,2.21989706654312,0.0524451052237091));
#37781=CARTESIAN_POINT('Ctrl Pts',(-2.79846764402885,1.33473338532309,0.104890210447416));
#37782=CARTESIAN_POINT('Ctrl Pts',(-2.92193100282573,0.379041548713593,
0.157335315671123));
#37783=CARTESIAN_POINT('Ctrl Pts',(-2.93800868581449,0.25458915624929,0.164164838084214));
#37784=CARTESIAN_POINT('Ctrl Pts',(-2.94535953294187,0.128940758021734,
0.170994360497305));
#37785=CARTESIAN_POINT('Ctrl Pts',(-2.94436911647834,0.00312614869137163,
0.177823882910396));
#37786=CARTESIAN_POINT('Origin',(0.,0.,0.));
#37787=CARTESIAN_POINT('',(-2.93740032720055,-0.000139020310086779,1.32217611708959));
#37788=CARTESIAN_POINT('',(-2.93737720095951,0.000230872487724698,1.1778238829104));
#37789=CARTESIAN_POINT('',(-2.942,-3.60291088309151E-16,0.));
#37790=CARTESIAN_POINT('Ctrl Pts',(-2.93740032720055,-0.000139020310086779,
1.32217611708959));
#37791=CARTESIAN_POINT('Ctrl Pts',(-2.93718361365059,0.494770241727901,
1.29550112610298));
#37792=CARTESIAN_POINT('Ctrl Pts',(-2.81848923912434,0.989776479202536,
1.26882613511636));
#37793=CARTESIAN_POINT('Ctrl Pts',(-2.58191143461274,1.4199490257311,1.24215114412975));
#37794=CARTESIAN_POINT('Ctrl Pts',(-2.11736289237333,2.26464377557798,1.18977163962524));
#37795=CARTESIAN_POINT('Ctrl Pts',(-1.19827972440715,2.85935294685526,1.13739213512074));
#37796=CARTESIAN_POINT('Ctrl Pts',(-0.2374000875181,2.93702585155106,1.08501263061624));
#37797=CARTESIAN_POINT('Ctrl Pts',(0.723479549370952,3.01469875624685,1.03263312611173));
#37798=CARTESIAN_POINT('Ctrl Pts',(1.72615565518287,2.57533539436116,0.980253621607226));
#37799=CARTESIAN_POINT('Ctrl Pts',(2.32033868002489,1.8162041612206,0.927874117102722));
#37800=CARTESIAN_POINT('Ctrl Pts',(2.9145217048669,1.05707292808004,0.875494612598217));
#37801=CARTESIAN_POINT('Ctrl Pts',(3.100211648739,-0.0218261763153739,0.823115108093712));
#37802=CARTESIAN_POINT('Ctrl Pts',(2.79403320730894,-0.935902477435646,
0.770735603589208));
#37803=CARTESIAN_POINT('Ctrl Pts',(2.48785476587888,-1.84997877855592,0.718356099084703));
#37804=CARTESIAN_POINT('Ctrl Pts',(1.68980793914667,-2.59923227640105,0.665976594580199));
#37805=CARTESIAN_POINT('Ctrl Pts',(0.75825229618776,-2.84733793424016,0.613597090075694));
#37806=CARTESIAN_POINT('Ctrl Pts',(-0.173303346771145,-3.09544359207927,
0.56121758557119));
#37807=CARTESIAN_POINT('Ctrl Pts',(-1.23836780595674,-2.84240140991237,
0.508838081066685));
#37808=CARTESIAN_POINT('Ctrl Pts',(-1.95858911760509,-2.20156094319437,
0.456458576562181));
#37809=CARTESIAN_POINT('Ctrl Pts',(-2.57405306040479,-1.65393177147606,
0.411697756737986));
#37810=CARTESIAN_POINT('Ctrl Pts',(-2.93769429310237,-0.823111776086056,
0.366936936913791));
#37811=CARTESIAN_POINT('Ctrl Pts',(-2.94437861999191,0.00228824954296311,
0.322176117089596));
#37812=CARTESIAN_POINT('Ctrl Pts',(-2.94436911647834,0.00312614869137163,
0.177823882910396));
#37813=CARTESIAN_POINT('Ctrl Pts',(-2.93775395051561,-0.837211781775621,
0.223439465721013));
#37814=CARTESIAN_POINT('Ctrl Pts',(-2.55902339432207,-1.68496462111194,
0.26905504853163));
#37815=CARTESIAN_POINT('Ctrl Pts',(-1.92306539600717,-2.23328718212897,
0.314670631342247));
#37816=CARTESIAN_POINT('Ctrl Pts',(-1.19189236073203,-2.86370408436305,
0.367115736565955));
#37817=CARTESIAN_POINT('Ctrl Pts',(-0.120702220522052,-3.09831789683223,
0.419560841789662));
#37818=CARTESIAN_POINT('Ctrl Pts',(0.807638005699694,-2.8335361097114,0.47200594701337));
#37819=CARTESIAN_POINT('Ctrl Pts',(1.73597823192144,-2.56875432259058,0.524451052237078));
#37820=CARTESIAN_POINT('Ctrl Pts',(2.52146854415495,-1.80457693587975,0.576896157460787));
#37821=CARTESIAN_POINT('Ctrl Pts',(2.81091642121069,-0.883954119006901,
0.629341262684494));
#37822=CARTESIAN_POINT('Ctrl Pts',(3.10036429826643,0.0366686978659464,
0.681786367908202));
#37823=CARTESIAN_POINT('Ctrl Pts',(2.89376974014439,1.11373694490081,0.734231473131909));
#37824=CARTESIAN_POINT('Ctrl Pts',(2.28393241469019,1.86192138048068,0.786676578355617));
#37825=CARTESIAN_POINT('Ctrl Pts',(1.674095089236,2.61010581606054,0.839121683579324));
#37826=CARTESIAN_POINT('Ctrl Pts',(0.661014996449636,3.02940644018541,0.891566788803033));
#37827=CARTESIAN_POINT('Ctrl Pts',(-0.299207810136722,2.93136603044105,
0.944011894026741));
#37828=CARTESIAN_POINT('Ctrl Pts',(-1.25943061672308,2.83332562069669,0.996456999250449));
#37829=CARTESIAN_POINT('Ctrl Pts',(-2.16679613710945,2.21794417708309,1.04890210447416));
#37830=CARTESIAN_POINT('Ctrl Pts',(-2.61293993368518,1.36206873790977,1.10134720969786));
#37831=CARTESIAN_POINT('Ctrl Pts',(-2.82979902340055,0.946049575313678,
1.12683943410204));
#37832=CARTESIAN_POINT('Ctrl Pts',(-2.93768601866802,0.47320929383844,1.15233165850622));
#37833=CARTESIAN_POINT('Ctrl Pts',(-2.93737720095951,0.000230872487724698,
1.1778238829104));
#37834=CARTESIAN_POINT('Origin',(0.,0.,0.));
#37835=CARTESIAN_POINT('',(-2.94487182720719,-0.00190539986535287,2.32217611708959));
#37836=CARTESIAN_POINT('',(-2.94409804542743,-0.00221960462873976,2.1778238829104));
#37837=CARTESIAN_POINT('',(-2.942,-3.60291088309151E-16,0.));
#37838=CARTESIAN_POINT('Ctrl Pts',(-2.94487182720719,-0.00190539986535287,
2.32217611708959));
#37839=CARTESIAN_POINT('Ctrl Pts',(-2.93849254859689,0.841069663508672,
2.27644481979667));
#37840=CARTESIAN_POINT('Ctrl Pts',(-2.55692453936773,1.68909389771769,2.23071352250375));
#37841=CARTESIAN_POINT('Ctrl Pts',(-1.91797659724234,2.23693579382214,2.18498222521083));
#37842=CARTESIAN_POINT('Ctrl Pts',(-1.18614132044426,2.86442044357863,2.13260272070633));
#37843=CARTESIAN_POINT('Ctrl Pts',(-0.116653199765081,3.09810042098425,
2.08022321620182));
#37844=CARTESIAN_POINT('Ctrl Pts',(0.810201861614963,2.83303510458914,2.02784371169732));
#37845=CARTESIAN_POINT('Ctrl Pts',(1.73705692299501,2.56796978819403,1.97546420719281));
#37846=CARTESIAN_POINT('Ctrl Pts',(2.52127892507592,1.80415917799819,1.92308470268831));
#37847=CARTESIAN_POINT('Ctrl Pts',(2.81068910755427,0.88461468761641,1.8707051981838));
#37848=CARTESIAN_POINT('Ctrl Pts',(3.10009929003262,-0.0349298027653776,
1.8183256936793));
#37849=CARTESIAN_POINT('Ctrl Pts',(2.89469765290841,-1.11020817333311,1.76594618917479));
#37850=CARTESIAN_POINT('Ctrl Pts',(2.28672630753671,-1.85833254788295,1.71356668467029));
#37851=CARTESIAN_POINT('Ctrl Pts',(1.67875496216501,-2.60645692243279,1.66118718016578));
#37852=CARTESIAN_POINT('Ctrl Pts',(0.668213908545816,-3.02742730096473,
1.60880767566128));
#37853=CARTESIAN_POINT('Ctrl Pts',(-0.291083395731117,-2.93219727380604,
1.55642817115678));
#37854=CARTESIAN_POINT('Ctrl Pts',(-1.25038070000804,-2.83696724664735,
1.50404866665227));
#37855=CARTESIAN_POINT('Ctrl Pts',(-2.15843425494271,-2.22553681379804,
1.45166916214777));
#37856=CARTESIAN_POINT('Ctrl Pts',(-2.60745407415374,-1.37248143316515,
1.39928965764326));
#37857=CARTESIAN_POINT('Ctrl Pts',(-2.82780430697652,-0.953856366540085,
1.37358514412537));
#37858=CARTESIAN_POINT('Ctrl Pts',(-2.93760915637607,-0.477042717206063,
1.34788063060748));
#37859=CARTESIAN_POINT('Ctrl Pts',(-2.93740032720055,-0.000139020310086779,
1.32217611708959));
#37860=CARTESIAN_POINT('Ctrl Pts',(-2.93737720095951,0.000230872487724698,
1.1778238829104));
#37861=CARTESIAN_POINT('Ctrl Pts',(-2.9370506885783,-0.499848321024544,
1.20477676372993));
#37862=CARTESIAN_POINT('Ctrl Pts',(-2.81577431600542,-1.00008193824477,
1.23172964454946));
#37863=CARTESIAN_POINT('Ctrl Pts',(-2.57446559490686,-1.43347457044749,
1.25868252536899));
#37864=CARTESIAN_POINT('Ctrl Pts',(-2.10492538678771,-2.27677300489839,
1.31112763059269));
#37865=CARTESIAN_POINT('Ctrl Pts',(-1.1809228977843,-2.86700043906715,1.3635727358164));
#37866=CARTESIAN_POINT('Ctrl Pts',(-0.218377608724914,-2.93852741234213,
1.41601784104011));
#37867=CARTESIAN_POINT('Ctrl Pts',(0.744167680334467,-3.01005438561711,
1.46846294626382));
#37868=CARTESIAN_POINT('Ctrl Pts',(1.74525576944982,-2.56288089799832,1.52090805148753));
#37869=CARTESIAN_POINT('Ctrl Pts',(2.33429173832943,-1.79826479808332,1.57335315671123));
#37870=CARTESIAN_POINT('Ctrl Pts',(2.92332770720905,-1.03364869816832,1.62579826193494));
#37871=CARTESIAN_POINT('Ctrl Pts',(3.10031155585293,0.0484100140428809,
1.67824336715865));
#37872=CARTESIAN_POINT('Ctrl Pts',(2.78557670999694,0.960852278151669,1.73068847238236));
#37873=CARTESIAN_POINT('Ctrl Pts',(2.47084186414094,1.87329454226046,1.78313357760607));
#37874=CARTESIAN_POINT('Ctrl Pts',(1.66438832378506,2.61612035826684,1.83557868282977));
#37875=CARTESIAN_POINT('Ctrl Pts',(0.729213057861966,2.85498007465664,1.88802378805348));
#37876=CARTESIAN_POINT('Ctrl Pts',(-0.205962208061124,3.09383979104644,
1.94046889327719));
#37877=CARTESIAN_POINT('Ctrl Pts',(-1.26985919955142,2.82873340781965,1.9929139985009));
#37878=CARTESIAN_POINT('Ctrl Pts',(-1.98360551176881,2.17898571169394,2.0453591037246));
#37879=CARTESIAN_POINT('Ctrl Pts',(-2.58452748049057,1.63194587688865,2.08951403011987));
#37880=CARTESIAN_POINT('Ctrl Pts',(-2.93724853244873,0.81225677381718,2.13366895651513));
#37881=CARTESIAN_POINT('Ctrl Pts',(-2.94409804542743,-0.00221960462873976,
2.1778238829104));
#37882=CARTESIAN_POINT('Origin',(0.,0.,0.));
#37883=CARTESIAN_POINT('',(-2.94188729812012,0.00254759896953657,3.32217611708959));
#37884=CARTESIAN_POINT('',(-2.94300132914192,0.00247067809074119,3.17782388291039));
#37885=CARTESIAN_POINT('',(-2.942,-3.60291088309151E-16,0.));
#37886=CARTESIAN_POINT('Ctrl Pts',(-2.94188729812012,0.00254759896953657,
3.32217611708959));
#37887=CARTESIAN_POINT('Ctrl Pts',(-2.94391723822425,0.231870355671395,
3.30976801799487));
#37888=CARTESIAN_POINT('Ctrl Pts',(-2.91930872547992,0.460762551320829,
3.29735991890015));
#37889=CARTESIAN_POINT('Ctrl Pts',(-2.86638309031571,0.682908266801983,
3.28495181980542));
#37890=CARTESIAN_POINT('Ctrl Pts',(-2.64296300603654,1.62067338423639,3.23257231530092));
#37891=CARTESIAN_POINT('Ctrl Pts',(-1.91492649555138,2.438214961245,3.18019281079642));
#37892=CARTESIAN_POINT('Ctrl Pts',(-1.00922037183541,2.76839122410029,3.12781330629191));
#37893=CARTESIAN_POINT('Ctrl Pts',(-0.103514248119433,3.09856748695557,
3.07543380178741));
#37894=CARTESIAN_POINT('Ctrl Pts',(0.979861488827348,2.94137843565753,3.0230542972829));
#37895=CARTESIAN_POINT('Ctrl Pts',(1.75438420282982,2.3674145763557,2.9706747927784));
#37896=CARTESIAN_POINT('Ctrl Pts',(2.5289069168323,1.79345071705387,2.91829528827389));
#37897=CARTESIAN_POINT('Ctrl Pts',(2.99457660789046,0.802712049748258,2.86591578376939));
#37898=CARTESIAN_POINT('Ctrl Pts',(2.94227021542597,-0.159880282562335,
2.81353627926488));
#37899=CARTESIAN_POINT('Ctrl Pts',(2.88996382296149,-1.12247261487293,2.76115677476038));
#37900=CARTESIAN_POINT('Ctrl Pts',(2.31968134697434,-2.0569186121885,2.70877727025587));
#37901=CARTESIAN_POINT('Ctrl Pts',(1.48752538566269,-2.54357700727495,2.65639776575137));
#37902=CARTESIAN_POINT('Ctrl Pts',(0.655369424351043,-3.0302354023614,2.60401826124687));
#37903=CARTESIAN_POINT('Ctrl Pts',(-0.438660022285117,-3.06910619521874,
2.55163875674236));
#37904=CARTESIAN_POINT('Ctrl Pts',(-1.30325595742871,-2.64273334365957,
2.49925925223786));
#37905=CARTESIAN_POINT('Ctrl Pts',(-2.1678518925723,-2.21636049210041,2.44687974773335));
#37906=CARTESIAN_POINT('Ctrl Pts',(-2.80301431622333,-1.32474399612474,
2.39450024322885));
#37907=CARTESIAN_POINT('Ctrl Pts',(-2.92350431159035,-0.368291087083228,
2.34212073872434));
#37908=CARTESIAN_POINT('Ctrl Pts',(-2.93879736301763,-0.246894422727957,
2.33547253151276));
#37909=CARTESIAN_POINT('Ctrl Pts',(-2.94579921760659,-0.124453265927633,
2.32882432430118));
#37910=CARTESIAN_POINT('Ctrl Pts',(-2.94487182720719,-0.00190539986535287,
2.32217611708959));
#37911=CARTESIAN_POINT('Ctrl Pts',(-2.94409804542743,-0.00221960462873976,
2.1778238829104));
#37912=CARTESIAN_POINT('Ctrl Pts',(-2.94538405566721,-0.155139230593375,
2.18611406173884));
#37913=CARTESIAN_POINT('Ctrl Pts',(-2.93447780370748,-0.307875103637501,
2.19440424056728));
#37914=CARTESIAN_POINT('Ctrl Pts',(-2.91073286453113,-0.458588216909009,
2.20269441939573));
#37915=CARTESIAN_POINT('Ctrl Pts',(-2.76051827213159,-1.41202544036162,
2.25513952461944));
#37916=CARTESIAN_POINT('Ctrl Pts',(-2.09649345438802,-2.28451087824219,
2.30758462984315));
#37917=CARTESIAN_POINT('Ctrl Pts',(-1.21754466145652,-2.68332862013697,
2.36002973506685));
#37918=CARTESIAN_POINT('Ctrl Pts',(-0.338595868525027,-3.08214636203174,
2.41247484029056));
#37919=CARTESIAN_POINT('Ctrl Pts',(0.755276899594388,-3.00729640794073,
2.46491994551426));
#37920=CARTESIAN_POINT('Ctrl Pts',(1.57170784623814,-2.49246924635079,2.51736505073797));
#37921=CARTESIAN_POINT('Ctrl Pts',(2.3881387928819,-1.97764208476085,2.56981015596168));
#37922=CARTESIAN_POINT('Ctrl Pts',(2.92712791805,-1.02283771567197,2.62225526118539));
#37923=CARTESIAN_POINT('Ctrl Pts',(2.94606932856971,-0.0578258660348382,
2.6747003664091));
#37924=CARTESIAN_POINT('Ctrl Pts',(2.96501073908941,0.907185983602299,2.72714547163281));
#37925=CARTESIAN_POINT('Ctrl Pts',(2.46390443496074,1.88240531378769,2.77959057685651));
#37926=CARTESIAN_POINT('Ctrl Pts',(1.66830473495772,2.42887370127543,2.83203568208022));
#37927=CARTESIAN_POINT('Ctrl Pts',(0.872705034954712,2.97534208876317,2.88448078730393));
#37928=CARTESIAN_POINT('Ctrl Pts',(-0.217388060922636,3.09305953355326,
2.93692589252764));
#37929=CARTESIAN_POINT('Ctrl Pts',(-1.11130990317228,2.72903986659667,2.98937099775135));
#37930=CARTESIAN_POINT('Ctrl Pts',(-2.00523174542191,2.36502019964009,3.04181610297505));
#37931=CARTESIAN_POINT('Ctrl Pts',(-2.70298233404385,1.51926342093683,3.09426120819876));
#37932=CARTESIAN_POINT('Ctrl Pts',(-2.89049530439613,0.572455370821353,
3.14670631342247));
#37933=CARTESIAN_POINT('Ctrl Pts',(-2.92758137029262,0.385196933861252,
3.15707883658511));
#37934=CARTESIAN_POINT('Ctrl Pts',(-2.94470877622731,0.1939857347123,3.16745135974775));
#37935=CARTESIAN_POINT('Ctrl Pts',(-2.94300132914192,0.00247067809074119,
3.17782388291039));
#37936=CARTESIAN_POINT('Origin',(0.,0.,0.));
#37937=CARTESIAN_POINT('',(-2.93815144027097,-0.00144838940242836,4.32217611708959));
#37938=CARTESIAN_POINT('',(-2.93758805006728,-0.000810565913221897,4.1778238829104));
#37939=CARTESIAN_POINT('',(-2.942,-3.60291088309151E-16,0.));
#37940=CARTESIAN_POINT('Ctrl Pts',(-2.93815144027097,-0.00144838940242836,
4.32217611708959));
#37941=CARTESIAN_POINT('Ctrl Pts',(-2.93549507201127,0.581944663119171,
4.29071171168856));
#37942=CARTESIAN_POINT('Ctrl Pts',(-2.76704590305946,1.16675179323199,4.25924730628754));
#37943=CARTESIAN_POINT('Ctrl Pts',(-2.44338137442995,1.64693751569171,4.22778290088651));
#37944=CARTESIAN_POINT('Ctrl Pts',(-1.90456974207211,2.44631350554451,4.175403396382));
#37945=CARTESIAN_POINT('Ctrl Pts',(-0.93560961338887,2.95575207374732,4.1230238918775));
#37946=CARTESIAN_POINT('Ctrl Pts',(0.0283581627927666,2.94647442485208,
4.07064438737299));
#37947=CARTESIAN_POINT('Ctrl Pts',(0.992325938974403,2.93719677595684,4.01826488286848));
#37948=CARTESIAN_POINT('Ctrl Pts',(1.95130136265442,2.40920290996356,3.96588537836398));
#37949=CARTESIAN_POINT('Ctrl Pts',(2.4746275187937,1.59960444002515,3.91350587385948));
#37950=CARTESIAN_POINT('Ctrl Pts',(2.99795367493297,0.790005970086747,3.86112636935497));
#37951=CARTESIAN_POINT('Ctrl Pts',(3.0856305635315,-0.301197103796779,3.80874686485047));
#37952=CARTESIAN_POINT('Ctrl Pts',(2.69828422619929,-1.18396704178881,3.75636736034596));
#37953=CARTESIAN_POINT('Ctrl Pts',(2.31093788886708,-2.06673697978085,3.70398785584146));
#37954=CARTESIAN_POINT('Ctrl Pts',(1.44856832560414,-2.7410737818814,3.65160835133695));
#37955=CARTESIAN_POINT('Ctrl Pts',(0.498448668458934,-2.90414611332682,
3.59922884683245));
#37956=CARTESIAN_POINT('Ctrl Pts',(-0.451670988686273,-3.06721844477224,
3.54684934232795));
#37957=CARTESIAN_POINT('Ctrl Pts',(-1.48954073971375,-2.71902630556253,
3.49446983782344));
#37958=CARTESIAN_POINT('Ctrl Pts',(-2.1490737861909,-2.01593590702758,3.44209033331894));
#37959=CARTESIAN_POINT('Ctrl Pts',(-2.65237107835254,-1.47939949597489,
3.40211892790916));
#37960=CARTESIAN_POINT('Ctrl Pts',(-2.93534805643284,-0.736191897535303,
3.36214752249938));
#37961=CARTESIAN_POINT('Ctrl Pts',(-2.94188729812012,0.00254759896953657,
3.32217611708959));
#37962=CARTESIAN_POINT('Ctrl Pts',(-2.94300132914192,0.00247067809074119,
3.17782388291039));
#37963=CARTESIAN_POINT('Ctrl Pts',(-2.93607565575577,-0.774344452547842,
3.21989646497146));
#37964=CARTESIAN_POINT('Ctrl Pts',(-2.61927127105561,-1.55615877069983,
3.26196904703253));
#37965=CARTESIAN_POINT('Ctrl Pts',(-2.06758380697847,-2.0994678941542,3.30404162909359));
#37966=CARTESIAN_POINT('Ctrl Pts',(-1.37988398712591,-2.77672378748653,
3.3564867343173));
#37967=CARTESIAN_POINT('Ctrl Pts',(-0.327208995338195,-3.08337625262348,
3.40893183954101));
#37968=CARTESIAN_POINT('Ctrl Pts',(0.616618861412321,-2.88139713307019,
3.46137694476472));
#37969=CARTESIAN_POINT('Ctrl Pts',(1.56044671816283,-2.67941801351691,3.51382204998842));
#37970=CARTESIAN_POINT('Ctrl Pts',(2.39542743987614,-1.9688073092734,3.56626715521213));
#37971=CARTESIAN_POINT('Ctrl Pts',(2.74572565546219,-1.06941987852551,3.61871226043584));
#37972=CARTESIAN_POINT('Ctrl Pts',(3.09602387104824,-0.170032447777603,
3.67115736565955));
#37973=CARTESIAN_POINT('Ctrl Pts',(2.96163958050702,0.918131709474696,3.72360247088326));
#37974=CARTESIAN_POINT('Ctrl Pts',(2.40306085127007,1.70527616384954,3.77604757610696));
#37975=CARTESIAN_POINT('Ctrl Pts',(1.84448212203313,2.49242061822439,3.82849268133067));
#37976=CARTESIAN_POINT('Ctrl Pts',(0.86170895410048,2.97854536972178,3.88093778655438));
#37977=CARTESIAN_POINT('Ctrl Pts',(-0.10290003671811,2.94483952623603,3.93338289177809));
#37978=CARTESIAN_POINT('Ctrl Pts',(-1.06750902753671,2.91113368275028,3.98582799700179));
#37979=CARTESIAN_POINT('Ctrl Pts',(-2.01395384124124,2.35759724428137,4.0382731022255));
#37980=CARTESIAN_POINT('Ctrl Pts',(-2.51622771244025,1.53338395412712,4.09071820744921));
#37981=CARTESIAN_POINT('Ctrl Pts',(-2.79430199366995,1.07707409733029,4.11975343260294));
#37982=CARTESIAN_POINT('Ctrl Pts',(-2.9362347477918,0.537799876108109,4.14878865775667));
#37983=CARTESIAN_POINT('Ctrl Pts',(-2.93758805006728,-0.000810565913221897,
4.1778238829104));
#37984=CARTESIAN_POINT('Origin',(0.,0.,0.));
#37985=CARTESIAN_POINT('',(-2.94644869531747,-0.000604754645607275,5.3221761170896));
#37986=CARTESIAN_POINT('',(-2.945679792052,-0.00146169071580815,5.1778238829104));
#37987=CARTESIAN_POINT('',(-2.942,-3.60291088309151E-16,0.));
#37988=CARTESIAN_POINT('Ctrl Pts',(-2.94644869531747,-0.000604754645607275,
5.3221761170896));
#37989=CARTESIAN_POINT('Ctrl Pts',(-2.94379550054715,0.929335583914262,
5.27165540538226));
#37990=CARTESIAN_POINT('Ctrl Pts',(-2.46604729438678,1.86162808593007,5.22113469367492));
#37991=CARTESIAN_POINT('Ctrl Pts',(-1.70849336410036,2.40074283220066,5.17061398196758));
#37992=CARTESIAN_POINT('Ctrl Pts',(-0.923066988207087,2.95969305927406,
5.11823447746308));
#37993=CARTESIAN_POINT('Ctrl Pts',(0.163133494924937,3.09600115191732,5.06585497295858));
#37994=CARTESIAN_POINT('Ctrl Pts',(1.06231690977038,2.74845383893534,5.01347546845407));
#37995=CARTESIAN_POINT('Ctrl Pts',(1.96150032461582,2.40090652595338,4.96109596394957));
#37996=CARTESIAN_POINT('Ctrl Pts',(2.67366667117468,1.56950380734618,4.90871645944506));
#37997=CARTESIAN_POINT('Ctrl Pts',(2.87899611438783,0.627612216959094,4.85633695494056));
#37998=CARTESIAN_POINT('Ctrl Pts',(3.08432555760098,-0.314279373428012,
4.80395745043605));
#37999=CARTESIAN_POINT('Ctrl Pts',(2.7828180974684,-1.36665983559502,4.75157794593155));
#38000=CARTESIAN_POINT('Ctrl Pts',(2.10987477706647,-2.05692589721429,4.69919844142705));
#38001=CARTESIAN_POINT('Ctrl Pts',(1.43693145666455,-2.74719195883355,4.64681893692254));
#38002=CARTESIAN_POINT('Ctrl Pts',(0.392552275993288,-3.07534361990509,
4.59443943241804));
#38003=CARTESIAN_POINT('Ctrl Pts',(-0.554252710038128,-2.89401445313919,
4.54205992791353));
#38004=CARTESIAN_POINT('Ctrl Pts',(-1.50105769606954,-2.71268528637328,
4.48968042340903));
#38005=CARTESIAN_POINT('Ctrl Pts',(-2.35028848746111,-2.02187529176995,
4.43730091890452));
#38006=CARTESIAN_POINT('Ctrl Pts',(-2.72057231514067,-1.13181358871689,
4.38492141440002));
#38007=CARTESIAN_POINT('Ctrl Pts',(-2.86842638565151,-0.776412580180032,
4.36400631529654));
#38008=CARTESIAN_POINT('Ctrl Pts',(-2.93991718809614,-0.389242894153138,
4.34309121619307));
#38009=CARTESIAN_POINT('Ctrl Pts',(-2.93815144027097,-0.00144838940242836,
4.32217611708959));
#38010=CARTESIAN_POINT('Ctrl Pts',(-2.93758805006728,-0.000810565913221897,
4.1778238829104));
#38011=CARTESIAN_POINT('Ctrl Pts',(-2.93867916073716,-0.435069497448956,
4.20123376298038));
#38012=CARTESIAN_POINT('Ctrl Pts',(-2.84838634229403,-0.86889693810433,
4.22464364305035));
#38013=CARTESIAN_POINT('Ctrl Pts',(-2.66438363654231,-1.25846258937073,
4.24805352312033));
#38014=CARTESIAN_POINT('Ctrl Pts',(-2.25216276075188,-2.13120570087471,
4.30049862834404));
#38015=CARTESIAN_POINT('Ctrl Pts',(-1.36961808047753,-2.78180178204309,
4.35294373356775));
#38016=CARTESIAN_POINT('Ctrl Pts',(-0.413994103635433,-2.91740931891088,
4.40538883879146));
#38017=CARTESIAN_POINT('Ctrl Pts',(0.541629873206673,-3.05301685577867,
4.45783394401517));
#38018=CARTESIAN_POINT('Ctrl Pts',(1.57033314661653,-2.67363584834587,4.51027904923887));
#38019=CARTESIAN_POINT('Ctrl Pts',(2.20908337968645,-1.9500304800975,4.56272415446258));
#38020=CARTESIAN_POINT('Ctrl Pts',(2.84783361275636,-1.22642511184914,4.61516925968629));
#38021=CARTESIAN_POINT('Ctrl Pts',(3.09663080548633,-0.158595382785209,
4.66761436491));
#38022=CARTESIAN_POINT('Ctrl Pts',(2.84348819889812,0.772815058373636,4.7200594701337));
#38023=CARTESIAN_POINT('Ctrl Pts',(2.5903455923099,1.70422549953248,4.77250457535741));
#38024=CARTESIAN_POINT('Ctrl Pts',(1.83526318640351,2.49921665278624,4.82494968058112));
#38025=CARTESIAN_POINT('Ctrl Pts',(0.918113109485756,2.79995295852677,4.87739478580482));
#38026=CARTESIAN_POINT('Ctrl Pts',(0.000963032567994487,3.1006892642673,
4.92983989102853));
#38027=CARTESIAN_POINT('Ctrl Pts',(-1.07825471536113,2.90717072249458,4.98228499625224));
#38028=CARTESIAN_POINT('Ctrl Pts',(-1.83377059439506,2.30650247319915,5.03473010147595));
#38029=CARTESIAN_POINT('Ctrl Pts',(-2.5208993779335,1.76020496324304,5.08242802862077));
#38030=CARTESIAN_POINT('Ctrl Pts',(-2.94027519175655,0.877129838501974,
5.13012595576559));
#38031=CARTESIAN_POINT('Ctrl Pts',(-2.945679792052,-0.00146169071580815,
5.1778238829104));
#38032=CARTESIAN_POINT('Origin',(0.,0.,0.));
#38033=CARTESIAN_POINT('',(-2.93949980478958,0.00219056232359141,6.3221761170896));
#38034=CARTESIAN_POINT('',(-2.94109090649655,0.00253660757586993,6.1778238829104));
#38035=CARTESIAN_POINT('',(-2.942,-3.60291088309151E-16,0.));
#38036=CARTESIAN_POINT('Ctrl Pts',(-2.93949980478958,0.00219056232359141,
6.3221761170896));
#38037=CARTESIAN_POINT('Ctrl Pts',(-2.94176361798241,0.320687415620876,
6.30497860358046));
#38038=CARTESIAN_POINT('Ctrl Pts',(-2.89395610782771,0.638523376129415,
6.28778109007132));
#38039=CARTESIAN_POINT('Ctrl Pts',(-2.79314214575126,0.938548174128603,
6.27058357656218));
#38040=CARTESIAN_POINT('Ctrl Pts',(-2.48608697885785,1.85235180335153,6.21820407205768));
#38041=CARTESIAN_POINT('Ctrl Pts',(-1.68730919078036,2.60092740470414,6.16582456755317));
#38042=CARTESIAN_POINT('Ctrl Pts',(-0.75552410366601,2.84810446618733,6.11344506304867));
#38043=CARTESIAN_POINT('Ctrl Pts',(0.176260983448343,3.09528152767051,6.06106555854416));
#38044=CARTESIAN_POINT('Ctrl Pts',(1.24105336959955,2.84106004928427,6.00868605403966));
#38045=CARTESIAN_POINT('Ctrl Pts',(1.96067583262663,2.19960587399116,5.95630654953515));
#38046=CARTESIAN_POINT('Ctrl Pts',(2.68029829565369,1.55815169869806,5.90392704503064));
#38047=CARTESIAN_POINT('Ctrl Pts',(3.05475083555665,0.52946482649812,5.85154754052614));
#38048=CARTESIAN_POINT('Ctrl Pts',(2.91587421520356,-0.424491793382225,
5.79916803602164));
#38049=CARTESIAN_POINT('Ctrl Pts',(2.77699759485047,-1.37844841326258,5.74678853151713));
#38050=CARTESIAN_POINT('Ctrl Pts',(2.12479181424134,-2.25767478082334,5.69440902701263));
#38051=CARTESIAN_POINT('Ctrl Pts',(1.25214960298458,-2.66732770639159,5.64202952250812));
#38052=CARTESIAN_POINT('Ctrl Pts',(0.379507391727844,-3.07698063195983,
5.58965001800362));
#38053=CARTESIAN_POINT('Ctrl Pts',(-0.713571250176501,-3.01706011553558,
5.53727051349912));
#38054=CARTESIAN_POINT('Ctrl Pts',(-1.53620630199898,-2.5144752771182,5.48489100899462));
#38055=CARTESIAN_POINT('Ctrl Pts',(-2.35884135382146,-2.01189043870081,
5.43251150449011));
#38056=CARTESIAN_POINT('Ctrl Pts',(-2.91103281556208,-1.0666412782903,5.3801319999856));
#38057=CARTESIAN_POINT('Ctrl Pts',(-2.94480241210512,-0.103220517333276,
5.3277524954811));
#38058=CARTESIAN_POINT('Ctrl Pts',(-2.94600079462919,-0.069031580495304,
5.32589370268393));
#38059=CARTESIAN_POINT('Ctrl Pts',(-2.94654631348559,-0.0348197596345374,
5.32403490988676));
#38060=CARTESIAN_POINT('Ctrl Pts',(-2.94644869531747,-0.000604754645607275,
5.3221761170896));
#38061=CARTESIAN_POINT('Ctrl Pts',(-2.945679792052,-0.00146169071580815,
5.1778238829104));
#38062=CARTESIAN_POINT('Ctrl Pts',(-2.94621768964176,-0.0889042840834332,
5.18257106098929));
#38063=CARTESIAN_POINT('Ctrl Pts',(-2.94265503660913,-0.176302465642187,
5.18731823906819));
#38064=CARTESIAN_POINT('Ctrl Pts',(-2.93484768462379,-0.263319805187537,
5.19206541714708));
#38065=CARTESIAN_POINT('Ctrl Pts',(-2.84859488567985,-1.22465587746066,
5.24451052237078));
#38066=CARTESIAN_POINT('Ctrl Pts',(-2.24427527765324,-2.13951006518879,
5.29695562759449));
#38067=CARTESIAN_POINT('Ctrl Pts',(-1.39390074925371,-2.59609494298297,
5.34940073281819));
#38068=CARTESIAN_POINT('Ctrl Pts',(-0.543526220854162,-3.05267982077716,
5.4018458380419));
#38069=CARTESIAN_POINT('Ctrl Pts',(0.552903227918311,-3.05099538863739,
5.45429094326562));
#38070=CARTESIAN_POINT('Ctrl Pts',(1.40187085321134,-2.59179983074767,5.50673604848932));
#38071=CARTESIAN_POINT('Ctrl Pts',(2.25083847850436,-2.13260427285796,5.55918115371303));
#38072=CARTESIAN_POINT('Ctrl Pts',(2.85234428031795,-1.21589758921833,5.61162625893673));
#38073=CARTESIAN_POINT('Ctrl Pts',(2.93564289965894,-0.254301037021637,
5.66407136416044));
#38074=CARTESIAN_POINT('Ctrl Pts',(3.01894151899992,0.707295515175046,5.71651646938415));
#38075=CARTESIAN_POINT('Ctrl Pts',(2.5840329558683,1.71378193592877,5.76896157460786));
#38076=CARTESIAN_POINT('Ctrl Pts',(1.82667504784324,2.31212597436553,5.82140667983157));
#38077=CARTESIAN_POINT('Ctrl Pts',(1.06931713981816,2.9104700128023,5.87385178505528));
#38078=CARTESIAN_POINT('Ctrl Pts',(-0.010490113100349,3.1006716689221,5.92629689027898));
#38079=CARTESIAN_POINT('Ctrl Pts',(-0.92671182736886,2.79711877487579,5.97874199550269));
#38080=CARTESIAN_POINT('Ctrl Pts',(-1.84293354163737,2.49356588082949,6.0311871007264));
#38081=CARTESIAN_POINT('Ctrl Pts',(-2.59556971725588,1.69625843661705,6.08363220595011));
#38082=CARTESIAN_POINT('Ctrl Pts',(-2.84584930505901,0.764074593638618,
6.13607731117382));
#38083=CARTESIAN_POINT('Ctrl Pts',(-2.91225724864025,0.516733559576513,
6.14999283508601));
#38084=CARTESIAN_POINT('Ctrl Pts',(-2.94329794130529,0.259896865352817,
6.16390835899821));
#38085=CARTESIAN_POINT('Ctrl Pts',(-2.94109090649655,0.00253660757586993,
6.1778238829104));
#38086=CARTESIAN_POINT('Origin',(0.,0.,0.));
#38087=CARTESIAN_POINT('',(-2.93998607517527,-0.0023358300504342,7.3221761170896));
#38088=CARTESIAN_POINT('',(-2.93846014819028,-0.00170708260597003,7.1778238829104));
#38089=CARTESIAN_POINT('',(-2.942,-3.60291088309151E-16,0.));
#38090=CARTESIAN_POINT('Ctrl Pts',(-2.93998607517527,-0.0023358300504342,
7.3221761170896));
#38091=CARTESIAN_POINT('Ctrl Pts',(-2.93483565594967,0.668801419715884,
7.28592229727415));
#38092=CARTESIAN_POINT('Ctrl Pts',(-2.70624449366069,1.34311250814063,7.2496684774587));
#38093=CARTESIAN_POINT('Ctrl Pts',(-2.28495024526271,1.86051554631288,7.21341465764326));
#38094=CARTESIAN_POINT('Ctrl Pts',(-1.67626448210673,2.60805925085354,7.16103515313876));
#38095=CARTESIAN_POINT('Ctrl Pts',(-0.665321452888303,3.02806588999372,
7.10865564863425));
#38096=CARTESIAN_POINT('Ctrl Pts',(0.293884302746592,2.93191878092119,7.05627614412975));
#38097=CARTESIAN_POINT('Ctrl Pts',(1.25309005838148,2.83577167184866,7.00389663962524));
#38098=CARTESIAN_POINT('Ctrl Pts',(2.16055854043283,2.22347081456344,6.95151713512074));
#38099=CARTESIAN_POINT('Ctrl Pts',(2.60876358347624,1.3699884259484,6.89913763061623));
#38100=CARTESIAN_POINT('Ctrl Pts',(3.05696862651966,0.516506037333356,6.84675812611173));
#38101=CARTESIAN_POINT('Ctrl Pts',(3.04591023055511,-0.578157882611513,
6.79437862160723));
#38102=CARTESIAN_POINT('Ctrl Pts',(2.58055450279311,-1.42241139605186,6.74199911710272));
#38103=CARTESIAN_POINT('Ctrl Pts',(2.11519877503111,-2.26666490949219,6.68961961259822));
#38104=CARTESIAN_POINT('Ctrl Pts',(1.19554571547167,-2.86050801642801,6.63724010809371));
#38105=CARTESIAN_POINT('Ctrl Pts',(0.234593342362696,-2.93725751088208,
6.5848606035892));
#38106=CARTESIAN_POINT('Ctrl Pts',(-0.726359030746288,-3.01400700533615,
6.5324810990847));
#38107=CARTESIAN_POINT('Ctrl Pts',(-1.72861071740481,-2.57366288730847,
6.4801015945802));
#38108=CARTESIAN_POINT('Ctrl Pts',(-2.32207028787941,-1.813974999748,6.4277220900757));
#38109=CARTESIAN_POINT('Ctrl Pts',(-2.72068210106971,-1.30371182195979,
6.39254009908033));
#38110=CARTESIAN_POINT('Ctrl Pts',(-2.93486858555413,-0.649377666932483,
6.35735810808496));
#38111=CARTESIAN_POINT('Ctrl Pts',(-2.93949980478958,0.00219056232359141,
6.3221761170896));
#38112=CARTESIAN_POINT('Ctrl Pts',(-2.94109090649655,0.00253660757586993,
6.1778238829104));
#38113=CARTESIAN_POINT('Ctrl Pts',(-2.9349800243151,-0.710047628629508,
6.21635346422191));
#38114=CARTESIAN_POINT('Ctrl Pts',(-2.67397994955092,-1.42664569379386,
6.25488304553342));
#38115=CARTESIAN_POINT('Ctrl Pts',(-2.20308134670334,-1.95680883878727,
6.29341262684494));
#38116=CARTESIAN_POINT('Ctrl Pts',(-1.5621108005568,-2.67844818649031,6.34585773206864));
#38117=CARTESIAN_POINT('Ctrl Pts',(-0.532246708275948,-3.05466664015197,
6.39830283729235));
#38118=CARTESIAN_POINT('Ctrl Pts',(0.42295609402977,-2.91612352177857,6.45074794251606));
#38119=CARTESIAN_POINT('Ctrl Pts',(1.3781588963355,-2.77758040340517,6.50319304773977));
#38120=CARTESIAN_POINT('Ctrl Pts',(2.25870040866608,-2.12427571299673,6.55563815296348));
#38121=CARTESIAN_POINT('Ctrl Pts',(2.66823777423309,-1.25027014357196,6.60808325818718));
#38122=CARTESIAN_POINT('Ctrl Pts',(3.07777513980009,-0.376264574147203,
6.66052836341089));
#38123=CARTESIAN_POINT('Ctrl Pts',(3.01630835860352,0.718441874293864,6.7129734686346));
#38124=CARTESIAN_POINT('Ctrl Pts',(2.51150440524776,1.54110800210975,6.76541857385831));
#38125=CARTESIAN_POINT('Ctrl Pts',(2.006700451892,2.36377412992563,6.81786367908202));
#38126=CARTESIAN_POINT('Ctrl Pts',(1.05855932637705,2.91439993711633,6.87030878430572));
#38127=CARTESIAN_POINT('Ctrl Pts',(0.0938513252260113,2.94514179293546,
6.92275388952943));
#38128=CARTESIAN_POINT('Ctrl Pts',(-0.870856675925038,2.9758836487546,6.97519899475314));
#38129=CARTESIAN_POINT('Ctrl Pts',(-1.85213155271217,2.48674155320215,7.02764409997685));
#38130=CARTESIAN_POINT('Ctrl Pts',(-2.40828908863565,1.69788454181399,7.08008920520056));
#38131=CARTESIAN_POINT('Ctrl Pts',(-2.75376700818296,1.2078566962645,7.11266743110384));
#38132=CARTESIAN_POINT('Ctrl Pts',(-2.93520341737875,0.60217681128353,7.14524565700712));
#38133=CARTESIAN_POINT('Ctrl Pts',(-2.93846014819028,-0.00170708260597003,
7.1778238829104));
#38134=CARTESIAN_POINT('Origin',(0.,0.,0.));
#38135=CARTESIAN_POINT('',(-2.94622250669394,0.000937675328142526,8.3221761170896));
#38136=CARTESIAN_POINT('',(-2.94656696235233,-0.000396508504380587,8.1778238829104));
#38137=CARTESIAN_POINT('',(-2.942,-3.60291088309151E-16,0.));
#38138=CARTESIAN_POINT('Ctrl Pts',(-2.94622250669394,0.000937675328142526,
8.3221761170896));
#38139=CARTESIAN_POINT('Ctrl Pts',(-2.94645073222768,0.0548930361868928,
8.31924549547236));
#38140=CARTESIAN_POINT('Ctrl Pts',(-2.94509413407217,0.108836699779164,
8.31631487385511));
#38141=CARTESIAN_POINT('Ctrl Pts',(-2.94211616003438,0.162690705921765,
8.31338425223786));
#38142=CARTESIAN_POINT('Ctrl Pts',(-2.88889031756852,1.12523262560549,8.26100474773336));
#38143=CARTESIAN_POINT('Ctrl Pts',(-2.31771549444688,2.05913344782865,8.20862524322884));
#38144=CARTESIAN_POINT('Ctrl Pts',(-1.48509504480843,2.54499674522788,8.15624573872434));
#38145=CARTESIAN_POINT('Ctrl Pts',(-0.652474595169965,3.03086004262711,
8.10386623421983));
#38146=CARTESIAN_POINT('Ctrl Pts',(0.44159148098532,3.06868581520241,8.05148672971533));
#38147=CARTESIAN_POINT('Ctrl Pts',(1.30577973958019,2.64148726651903,7.99910722521083));
#38148=CARTESIAN_POINT('Ctrl Pts',(2.16996799817506,2.21428871783565,7.94672772070633));
#38149=CARTESIAN_POINT('Ctrl Pts',(2.8042784392095,1.3220658478936,7.89434821620182));
#38150=CARTESIAN_POINT('Ctrl Pts',(2.92385476924452,0.36549831322338,7.84196871169732));
#38151=CARTESIAN_POINT('Ctrl Pts',(3.04343109927954,-0.591069221446826,
7.78958920719281));
#38152=CARTESIAN_POINT('Ctrl Pts',(2.64827331831513,-1.61198142084519,7.73720970268831));
#38153=CARTESIAN_POINT('Ctrl Pts',(1.9158389819387,-2.23876678477201,7.68483019818381));
#38154=CARTESIAN_POINT('Ctrl Pts',(1.18340464556226,-2.86555214869884,7.6324506936793));
#38155=CARTESIAN_POINT('Ctrl Pts',(0.113693753773775,-3.09821067715411,
7.58007118917479));
#38156=CARTESIAN_POINT('Ctrl Pts',(-0.812907669552306,-2.83226002346519,
7.52769168467029));
#38157=CARTESIAN_POINT('Ctrl Pts',(-1.73950909287838,-2.56630936977627,
7.47531218016578));
#38158=CARTESIAN_POINT('Ctrl Pts',(-2.52300104774206,-1.80174953394315,
7.42293267566128));
#38159=CARTESIAN_POINT('Ctrl Pts',(-2.81153277662714,-0.881929231056029,
7.37055317115678));
#38160=CARTESIAN_POINT('Ctrl Pts',(-2.90036087316611,-0.598751062127826,
7.35442748646772));
#38161=CARTESIAN_POINT('Ctrl Pts',(-2.94227697960606,-0.300857412821767,
7.33830180177866));
#38162=CARTESIAN_POINT('Ctrl Pts',(-2.93998607517527,-0.0023358300504342,
7.3221761170896));
#38163=CARTESIAN_POINT('Ctrl Pts',(-2.93846014819028,-0.00170708260597003,
7.1778238829104));
#38164=CARTESIAN_POINT('Ctrl Pts',(-2.94044617033292,-0.369968033311824,
7.19769076223082));
#38165=CARTESIAN_POINT('Ctrl Pts',(-2.87617048586605,-0.737561088352721,
7.21755764155125));
#38166=CARTESIAN_POINT('Ctrl Pts',(-2.7424268268773,-1.07785126568817,7.23742452087168));
#38167=CARTESIAN_POINT('Ctrl Pts',(-2.38936683413567,-1.97615813457835,
7.28986962609539));
#38168=CARTESIAN_POINT('Ctrl Pts',(-1.55220665359259,-2.68419994513487,
7.34231473131909));
#38169=CARTESIAN_POINT('Ctrl Pts',(-0.60776265660645,-2.88327813520494,
7.3947598365428));
#38170=CARTESIAN_POINT('Ctrl Pts',(0.336681340379679,-3.082356325275,7.44720494176651));
#38171=CARTESIAN_POINT('Ctrl Pts',(1.38840915380886,-2.77247089485864,7.49965004699022));
#38172=CARTESIAN_POINT('Ctrl Pts',(2.07402481044015,-2.09310519028348,7.55209515221392));
#38173=CARTESIAN_POINT('Ctrl Pts',(2.75964046707144,-1.41373948570832,7.60454025743763));
#38174=CARTESIAN_POINT('Ctrl Pts',(3.07914396690482,-0.364893506974353,
7.65698536266134));
#38175=CARTESIAN_POINT('Ctrl Pts',(2.8887227491853,0.5813339228528,7.70943046788505));
#38176=CARTESIAN_POINT('Ctrl Pts',(2.69830153146578,1.52756135267996,7.76187557310876));
#38177=CARTESIAN_POINT('Ctrl Pts',(1.99795559619334,2.37117023360031,7.81432067833246));
#38178=CARTESIAN_POINT('Ctrl Pts',(1.10291949457769,2.73244155291697,7.86676578355617));
#38179=CARTESIAN_POINT('Ctrl Pts',(0.207883392962048,3.09371287223363,7.91921088877988));
#38180=CARTESIAN_POINT('Ctrl Pts',(-0.881842874996807,2.97264662994661,
7.97165599400359));
#38181=CARTESIAN_POINT('Ctrl Pts',(-1.67575975122609,2.42373627051487,8.0241010992273));
#38182=CARTESIAN_POINT('Ctrl Pts',(-2.45144772506959,1.88742928765845,8.07534202712166));
#38183=CARTESIAN_POINT('Ctrl Pts',(-2.94475435076587,0.942699847726619,
8.12658295501603));
#38184=CARTESIAN_POINT('Ctrl Pts',(-2.94656696235233,-0.000396508504380587,
8.1778238829104));
#38185=CARTESIAN_POINT('Origin',(0.,0.,0.));
#38186=CARTESIAN_POINT('',(-2.93787859032851,0.00118007037484616,9.3221761170896));
#38187=CARTESIAN_POINT('',(-2.93938212312892,0.00216771032458683,9.1778238829104));
#38188=CARTESIAN_POINT('',(-2.942,-3.60291088309151E-16,0.));
#38189=CARTESIAN_POINT('Ctrl Pts',(-2.93787859032851,0.00118007037484616,
9.3221761170896));
#38190=CARTESIAN_POINT('Ctrl Pts',(-2.93938225399168,0.408942454113454,
9.30018918916604));
#38191=CARTESIAN_POINT('Ctrl Pts',(-2.86009946358647,0.816145924853212,
9.27820226124249));
#38192=CARTESIAN_POINT('Ctrl Pts',(-2.69715242952518,1.18654365111784,9.25621533331894));
#38193=CARTESIAN_POINT('Ctrl Pts',(-2.30896336853928,2.06894293121702,9.20383582881443));
#38194=CARTESIAN_POINT('Ctrl Pts',(-1.44594933104186,2.74245624053358,9.15145632430993));
#38195=CARTESIAN_POINT('Ctrl Pts',(-0.495674163844965,2.9046210644708,9.09907681980542));
#38196=CARTESIAN_POINT('Ctrl Pts',(0.454601003351916,3.06678588840801,9.04669731530092));
#38197=CARTESIAN_POINT('Ctrl Pts',(1.49213730024827,2.7176022269659,8.99431781079641));
#38198=CARTESIAN_POINT('Ctrl Pts',(2.15099835280526,2.01388208359571,8.94193830629191));
#38199=CARTESIAN_POINT('Ctrl Pts',(2.80985940536224,1.31016194022553,8.88955880178741));
#38200=CARTESIAN_POINT('Ctrl Pts',(3.09004521357986,0.251905314927287,8.8371792972829));
#38201=CARTESIAN_POINT('Ctrl Pts',(2.86572951288042,-0.685645923387644,
8.7847997927784));
#38202=CARTESIAN_POINT('Ctrl Pts',(2.64141381218099,-1.62319716170258,8.73242028827389));
#38203=CARTESIAN_POINT('Ctrl Pts',(1.91259660256449,-2.44004301303419,8.68004078376939));
#38204=CARTESIAN_POINT('Ctrl Pts',(1.00657547791151,-2.76935400264746,8.62766127926488));
#38205=CARTESIAN_POINT('Ctrl Pts',(0.100554353258536,-3.09866499226073,
8.57528177476038));
#38206=CARTESIAN_POINT('Ctrl Pts',(-0.982670686430926,-2.94044112015566,
8.52290227025587));
#38207=CARTESIAN_POINT('Ctrl Pts',(-1.75664477537062,-2.36573767553097,
8.47052276575137));
#38208=CARTESIAN_POINT('Ctrl Pts',(-2.48731518632227,-1.82318876070292,
8.42107388286411));
#38209=CARTESIAN_POINT('Ctrl Pts',(-2.94237161798714,-0.909460413780999,
8.37162499997686));
#38210=CARTESIAN_POINT('Ctrl Pts',(-2.94622250669394,0.000937675328142526,
8.3221761170896));
#38211=CARTESIAN_POINT('Ctrl Pts',(-2.94656696235233,-0.000396508504380587,
8.1778238829104));
#38212=CARTESIAN_POINT('Ctrl Pts',(-2.94660955927376,-0.0225595585939061,
8.17902806023974));
#38213=CARTESIAN_POINT('Ctrl Pts',(-2.94638072162746,-0.0447217067897041,
8.18023223756908));
#38214=CARTESIAN_POINT('Ctrl Pts',(-2.94587773547044,-0.0668776312364038,
8.18143641489842));
#38215=CARTESIAN_POINT('Ctrl Pts',(-2.92397135898579,-1.03182669697942,
8.23388152012213));
#38216=CARTESIAN_POINT('Ctrl Pts',(-2.3820511215168,-1.98497035188899,8.28632662534583));
#38217=CARTESIAN_POINT('Ctrl Pts',(-1.5640421648278,-2.49728659914907,8.33877173056954));
#38218=CARTESIAN_POINT('Ctrl Pts',(-0.746033208138801,-3.00960284640916,
8.39121683579325));
#38219=CARTESIAN_POINT('Ctrl Pts',(0.348064467770205,-3.08109168601973,
8.44366194101695));
#38220=CARTESIAN_POINT('Ctrl Pts',(1.22578367546087,-2.6795750856597,8.49610704624066));
#38221=CARTESIAN_POINT('Ctrl Pts',(2.10350288315153,-2.27805848529968,8.54855215146437));
#38222=CARTESIAN_POINT('Ctrl Pts',(2.76484362262384,-1.40353644496905,8.60099725668809));
#38223=CARTESIAN_POINT('Ctrl Pts',(2.91212808132915,-0.44964238612263,8.65344236191179));
#38224=CARTESIAN_POINT('Ctrl Pts',(3.05941254003446,0.504251672723784,8.7058874671355));
#38225=CARTESIAN_POINT('Ctrl Pts',(2.69264071797276,1.537517750086,8.75833257235921));
#38226=CARTESIAN_POINT('Ctrl Pts',(1.97690123029279,2.18506974304829,8.81077767758291));
#38227=CARTESIAN_POINT('Ctrl Pts',(1.26116174261282,2.83262173601059,8.86322278280662));
#38228=CARTESIAN_POINT('Ctrl Pts',(0.196454589314577,3.09445964457298,8.91566788803033));
#38229=CARTESIAN_POINT('Ctrl Pts',(-0.737982063629216,2.8527269003752,8.96811299325404));
#38230=CARTESIAN_POINT('Ctrl Pts',(-1.672418716573,2.61099415617743,9.02055809847774));
#38231=CARTESIAN_POINT('Ctrl Pts',(-2.47658486916233,1.86569075921951,9.07300320370145));
#38232=CARTESIAN_POINT('Ctrl Pts',(-2.78851523225651,0.952287217651892,
9.12544830892515));
#38233=CARTESIAN_POINT('Ctrl Pts',(-2.89235416848512,0.648223031136026,
9.1429068335869));
#38234=CARTESIAN_POINT('Ctrl Pts',(-2.94164516567622,0.325530543639097,
9.16036535824865));
#38235=CARTESIAN_POINT('Ctrl Pts',(-2.93938212312892,0.00216771032458683,
9.1778238829104));
#38236=CARTESIAN_POINT('Origin',(0.,0.,0.));
#38237=CARTESIAN_POINT('',(-2.94242444587263,-0.00248500551853048,10.3221761170896));
#38238=CARTESIAN_POINT('',(-2.93989309841074,-0.00232834448912937,10.1778238829104));
#38239=CARTESIAN_POINT('',(-2.942,-3.60291088309151E-16,0.));
#38240=CARTESIAN_POINT('Ctrl Pts',(-2.94242444587263,-0.00248500551853048,
10.3221761170896));
#38241=CARTESIAN_POINT('Ctrl Pts',(-2.93565996783783,0.755676872330999,
10.2811328828597));
#38242=CARTESIAN_POINT('Ctrl Pts',(-2.63573211439715,1.5185652175411,10.2400896486299));
#38243=CARTESIAN_POINT('Ctrl Pts',(-2.10792737213773,2.05892622612073,10.1990464144));
#38244=CARTESIAN_POINT('Ctrl Pts',(-1.43434130141424,2.74853664338077,10.1466669098955));
#38245=CARTESIAN_POINT('Ctrl Pts',(-0.389613404070186,3.07571802003838,
10.094287405391));
#38246=CARTESIAN_POINT('Ctrl Pts',(0.557026464387836,2.89349108573471,10.0419079008865));
#38247=CARTESIAN_POINT('Ctrl Pts',(1.50366633284582,2.71126415143105,9.98952839638201));
#38248=CARTESIAN_POINT('Ctrl Pts',(2.35221817241779,2.01962890616612,9.9371488918775));
#38249=CARTESIAN_POINT('Ctrl Pts',(2.72164717416933,1.12921048240304,9.884769387373));
#38250=CARTESIAN_POINT('Ctrl Pts',(3.09107617592089,0.238792058639911,9.83238988286849));
#38251=CARTESIAN_POINT('Ctrl Pts',(2.981382339852,-0.85040954362138,9.78001037836398));
#38252=CARTESIAN_POINT('Ctrl Pts',(2.44180970997212,-1.64926869616342,9.72763087385948));
#38253=CARTESIAN_POINT('Ctrl Pts',(1.90223708009224,-2.44812784870545,9.67525136935497));
#38254=CARTESIAN_POINT('Ctrl Pts',(0.93278565640137,-2.95664455152821,9.62287186485046));
#38255=CARTESIAN_POINT('Ctrl Pts',(-0.031174037472469,-2.94644704900523,
9.57049236034596));
#38256=CARTESIAN_POINT('Ctrl Pts',(-0.995133731346301,-2.93624954648225,
9.51811285584146));
#38257=CARTESIAN_POINT('Ctrl Pts',(-1.9536016954031,-2.40733783861356,9.46573335133695));
#38258=CARTESIAN_POINT('Ctrl Pts',(-2.4761536351943,-1.5972393592383,9.41335384683245));
#38259=CARTESIAN_POINT('Ctrl Pts',(-2.77935810415337,-1.1271894741653,9.3829612702515));
#38260=CARTESIAN_POINT('Ctrl Pts',(-2.93580007289335,-0.56247072784923,
9.35256869367055));
#38261=CARTESIAN_POINT('Ctrl Pts',(-2.93787859032851,0.00118007037484616,
9.3221761170896));
#38262=CARTESIAN_POINT('Ctrl Pts',(-2.93938212312892,0.00216771032458683,
9.1778238829104));
#38263=CARTESIAN_POINT('Ctrl Pts',(-2.93484702512206,-0.645845798130107,
9.21281046347236));
#38264=CARTESIAN_POINT('Ctrl Pts',(-2.72327366311651,-1.29655137950586,
9.24779704403432));
#38265=CARTESIAN_POINT('Ctrl Pts',(-2.32875660055073,-1.80542543875765,
9.28278362459629));
#38266=CARTESIAN_POINT('Ctrl Pts',(-1.73737303215174,-2.56823086742229,
9.33522872981999));
#38267=CARTESIAN_POINT('Ctrl Pts',(-0.73491132175476,-3.01233803857425,
9.3876738350437));
#38268=CARTESIAN_POINT('Ctrl Pts',(0.227407657021308,-2.93784857599215,
9.44011894026741));
#38269=CARTESIAN_POINT('Ctrl Pts',(1.1897266357974,-2.86335911341005,9.49256404549111));
#38270=CARTESIAN_POINT('Ctrl Pts',(2.11190288295256,-2.27027301709385,9.54500915071482));
#38271=CARTESIAN_POINT('Ctrl Pts',(2.57885359588429,-1.42554607687093,9.59745425593853));
#38272=CARTESIAN_POINT('Ctrl Pts',(3.045804308816,-0.580819136648041,9.64989936116224));
#38273=CARTESIAN_POINT('Ctrl Pts',(3.05752948752431,0.515548647481566,9.70234446638595));
#38274=CARTESIAN_POINT('Ctrl Pts',(2.60875076544854,1.37006875926759,9.75478957160966));
#38275=CARTESIAN_POINT('Ctrl Pts',(2.15997204337277,2.22458887105361,9.80723467683336));
#38276=CARTESIAN_POINT('Ctrl Pts',(1.25068942051291,2.83726131049606,9.85967978205706));
#38277=CARTESIAN_POINT('Ctrl Pts',(0.290183858659324,2.93231357229399,9.91212488728077));
#38278=CARTESIAN_POINT('Ctrl Pts',(-0.67032170319427,3.02736583409193,9.96456999250448));
#38279=CARTESIAN_POINT('Ctrl Pts',(-1.68205020404159,2.60479791824536,10.0170150977282));
#38280=CARTESIAN_POINT('Ctrl Pts',(-2.28961248249041,1.85481470515708,10.0694602029519));
#38281=CARTESIAN_POINT('Ctrl Pts',(-2.708067067946,1.33826862311137,10.1055814296047));
#38282=CARTESIAN_POINT('Ctrl Pts',(-2.93479827488144,0.666407318052135,
10.1417026562576));
#38283=CARTESIAN_POINT('Ctrl Pts',(-2.93989309841074,-0.00232834448912937,
10.1778238829104));
#38284=CARTESIAN_POINT('Origin',(0.,0.,-1.84858989190501));
#38285=CARTESIAN_POINT('',(-2.3720921752204,-0.00200333509135781,10.651410108095));
#38286=CARTESIAN_POINT('',(-2.37533330856671,0.000645282184899808,10.848589891905));
#38287=CARTESIAN_POINT('',(-2.37175,-1.78696459712734E-13,-1.84858989190501));
#38288=CARTESIAN_POINT('',(-2.34668236863852,0.343918483395543,11.62825));
#38289=CARTESIAN_POINT('Ctrl Pts',(-2.3720921752204,-0.00200333509135741,
10.651410108095));
#38290=CARTESIAN_POINT('Ctrl Pts',(-2.37359839777753,-0.170820576644891,
10.6627463783696));
#38291=CARTESIAN_POINT('Ctrl Pts',(-2.28072670946568,-1.11802807678178,
10.7264621531488));
#38292=CARTESIAN_POINT('Ctrl Pts',(-1.0098707589218,-2.60498459805753,10.8425574324324));
#38293=CARTESIAN_POINT('Ctrl Pts',(1.61803174729613,-2.2773674076414,10.999695945946));
#38294=CARTESIAN_POINT('Ctrl Pts',(2.79127527466209,0.0946110570183949,
11.1568344594594));
#38295=CARTESIAN_POINT('Ctrl Pts',(1.46022534703361,2.38369320998594,11.313972972973));
#38296=CARTESIAN_POINT('Ctrl Pts',(-1.1878082887304,2.52773050943662,11.4711114864865));
#38297=CARTESIAN_POINT('Ctrl Pts',(-2.23349531079268,1.11623543008163,11.5758704954955));
#38298=CARTESIAN_POINT('Ctrl Pts',(-2.34668236863853,0.343918483395475,
11.62825));
#38299=CARTESIAN_POINT('',(-0.439445221994028,2.33068358199191,11.62825));
#38300=CARTESIAN_POINT('Origin',(0.,0.,11.62825));
#38301=CARTESIAN_POINT('Ctrl Pts',(-2.37533330856671,0.000645282184899929,
10.848589891905));
#38302=CARTESIAN_POINT('Ctrl Pts',(-2.37266626526946,-0.74297942345447,
10.8986961737085));
#38303=CARTESIAN_POINT('Ctrl Pts',(-1.5987407489101,-2.26979394046941,11.0012475607357));
#38304=CARTESIAN_POINT('Ctrl Pts',(0.989622905930635,-2.61290295808564,
11.1562440529866));
#38305=CARTESIAN_POINT('Ctrl Pts',(2.72902843688469,-0.61088887604173,11.3135793686578));
#38306=CARTESIAN_POINT('Ctrl Pts',(2.00599839187704,1.9449087769569,11.4709146843289));
#38307=CARTESIAN_POINT('Ctrl Pts',(0.328567026486064,2.47549058867235,11.5758048947763));
#38308=CARTESIAN_POINT('Ctrl Pts',(-0.439445221994061,2.3306835819919,11.62825));
#38309=CARTESIAN_POINT('Origin',(0.,0.,-1.84858989190501));
#38310=CARTESIAN_POINT('',(-2.36842744616303,0.000951336475574988,9.65141010809499));
#38311=CARTESIAN_POINT('',(-2.37005148067835,-0.00187703978340947,9.84858989190503));
#38312=CARTESIAN_POINT('',(-2.37175,-1.78696459712734E-13,-1.84858989190501));
#38313=CARTESIAN_POINT('Ctrl Pts',(-2.36842744616303,0.000951336475575049,
9.65141010809499));
#38314=CARTESIAN_POINT('Ctrl Pts',(-2.36675180927421,-0.453446617531184,
9.68180268467594));
#38315=CARTESIAN_POINT('Ctrl Pts',(-2.02327622703562,-1.69331275929724,
9.76457476576139));
#38316=CARTESIAN_POINT('Ctrl Pts',(-0.0295588149451427,-2.79350652787453,
9.89972635135136));
#38317=CARTESIAN_POINT('Ctrl Pts',(2.31506703223917,-1.56365490661018,10.0568648648649));
#38318=CARTESIAN_POINT('Ctrl Pts',(2.58036243233743,1.07058768363104,10.2140033783784));
#38319=CARTESIAN_POINT('Ctrl Pts',(0.528133174514654,2.74331293137788,10.3711418918919));
#38320=CARTESIAN_POINT('Ctrl Pts',(-1.81626974066498,2.00910742659655,10.5169441351307));
#38321=CARTESIAN_POINT('Ctrl Pts',(-2.36663886088356,0.609203474490441,
10.6103668738651));
#38322=CARTESIAN_POINT('Ctrl Pts',(-2.3720921752204,-0.00200333509135741,
10.651410108095));
#38323=CARTESIAN_POINT('Ctrl Pts',(-2.37005148067835,-0.0018770397834093,
9.84858989190503));
#38324=CARTESIAN_POINT('Ctrl Pts',(-2.37190764427919,-0.245513112411714,
9.8649137704759));
#38325=CARTESIAN_POINT('Ctrl Pts',(-2.22599738542921,-1.26973141402768,
9.93368275427047));
#38326=CARTESIAN_POINT('Ctrl Pts',(-0.757654725048104,-2.69016151139635,
10.0548968432888));
#38327=CARTESIAN_POINT('Ctrl Pts',(1.83027666927001,-2.11210170665972,10.2122321589599));
#38328=CARTESIAN_POINT('Ctrl Pts',(2.77060484795253,0.367287133540841,10.369567474631));
#38329=CARTESIAN_POINT('Ctrl Pts',(1.21665350181368,2.51610800548609,10.5269027903021));
#38330=CARTESIAN_POINT('Ctrl Pts',(-1.43234772356642,2.39972494583597,10.6842381059733));
#38331=CARTESIAN_POINT('Ctrl Pts',(-2.35921176770024,0.848280000432971,
10.7914671398409));
#38332=CARTESIAN_POINT('Ctrl Pts',(-2.37545779881228,0.0353556381482985,
10.8462510684848));
#38333=CARTESIAN_POINT('Ctrl Pts',(-2.37533330856671,0.000645282184899929,
10.848589891905));
#38334=CARTESIAN_POINT('Origin',(0.,0.,-1.84858989190501));
#38335=CARTESIAN_POINT('',(-2.37515405515002,0.000755925037124906,8.65141010809499));
#38336=CARTESIAN_POINT('',(-2.36963954810708,0.00174754145538428,8.84858989190503));
#38337=CARTESIAN_POINT('',(-2.37175,-1.78696459712734E-13,-1.84858989190501));
#38338=CARTESIAN_POINT('Ctrl Pts',(-2.37515405515002,0.00075592503712492,
8.65141010809499));
#38339=CARTESIAN_POINT('Ctrl Pts',(-2.37204958700235,-0.733179040239741,
8.70085899098224));
#38340=CARTESIAN_POINT('Ctrl Pts',(-1.61660279875904,-2.25007474146859,
8.80268737837401));
#38341=CARTESIAN_POINT('Ctrl Pts',(0.954326572136137,-2.62560372673677,
8.95689527027026));
#38342=CARTESIAN_POINT('Ctrl Pts',(2.71697669134881,-0.650055649344734,
9.11403378378378));
#38343=CARTESIAN_POINT('Ctrl Pts',(2.03934512373477,1.90934627218937,9.2711722972973));
#38344=CARTESIAN_POINT('Ctrl Pts',(-0.469944521571767,2.75384968723896,
9.42831081081079));
#38345=CARTESIAN_POINT('Ctrl Pts',(-2.15345863304216,1.44000181080629,9.55505674774338));
#38346=CARTESIAN_POINT('Ctrl Pts',(-2.36963965360463,0.329676840769313,
9.62942318017144));
#38347=CARTESIAN_POINT('Ctrl Pts',(-2.36842744616303,0.000951336475575049,
9.65141010809499));
#38348=CARTESIAN_POINT('Ctrl Pts',(-2.36963954810708,0.00174754145538407,
8.84858989190503));
#38349=CARTESIAN_POINT('Ctrl Pts',(-2.36598349144566,-0.520661037292834,
8.88357647246699));
#38350=CARTESIAN_POINT('Ctrl Pts',(-1.9397431197991,-1.83158688452099,8.97100815825266));
#38351=CARTESIAN_POINT('Ctrl Pts',(0.215690902196592,-2.78647992051942,
9.11088494926201));
#38352=CARTESIAN_POINT('Ctrl Pts',(2.4459813653409,-1.35209655994371,9.26822026493315));
#38353=CARTESIAN_POINT('Ctrl Pts',(2.47433880171217,1.29947749716991,9.42555558060427));
#38354=CARTESIAN_POINT('Ctrl Pts',(0.275231669725872,2.78123058171878,9.58289089627539));
#38355=CARTESIAN_POINT('Ctrl Pts',(-1.91777323438188,1.86527979947427,9.72390233337565));
#38356=CARTESIAN_POINT('Ctrl Pts',(-2.36594419049973,0.537237102851684,
9.81246866525219));
#38357=CARTESIAN_POINT('Ctrl Pts',(-2.37005148067835,-0.0018770397834093,
9.84858989190503));
#38358=CARTESIAN_POINT('Origin',(0.,0.,-1.84858989190501));
#38359=CARTESIAN_POINT('',(-2.37012643568897,-0.00188307441280249,7.65141010809499));
#38360=CARTESIAN_POINT('',(-2.37543174471759,-0.000319652972777529,7.84858989190503));
#38361=CARTESIAN_POINT('',(-2.37175,-1.78696459712734E-13,-1.84858989190501));
#38362=CARTESIAN_POINT('Ctrl Pts',(-2.37012643568897,-0.00188307441280247,
7.65141010809499));
#38363=CARTESIAN_POINT('Ctrl Pts',(-2.37197329244753,-0.242542001652036,
7.66753579278404));
#38364=CARTESIAN_POINT('Ctrl Pts',(-2.22842022339473,-1.26275955622086,
7.7360409819776));
#38365=CARTESIAN_POINT('Ctrl Pts',(-0.770711640749916,-2.68524440462409,
7.85692567567567));
#38366=CARTESIAN_POINT('Ctrl Pts',(1.81639251383808,-2.12255793467458,8.01406418918919));
#38367=CARTESIAN_POINT('Ctrl Pts',(2.77208469636934,0.346526200869026,8.1712027027027));
#38368=CARTESIAN_POINT('Ctrl Pts',(1.23799993580832,2.50437418705365,8.32834121621622));
#38369=CARTESIAN_POINT('Ctrl Pts',(-1.40800742257503,2.4128922603655,8.48547972972973));
#38370=CARTESIAN_POINT('Ctrl Pts',(-2.35469744140074,0.865004378788607,
8.59316936035599));
#38371=CARTESIAN_POINT('Ctrl Pts',(-2.37533804356255,0.0442530790537146,
8.64847948647774));
#38372=CARTESIAN_POINT('Ctrl Pts',(-2.37515405515002,0.00075592503712492,
8.65141010809499));
#38373=CARTESIAN_POINT('Ctrl Pts',(-2.37543174471759,-0.000319652972777509,
7.84858989190503));
#38374=CARTESIAN_POINT('Ctrl Pts',(-2.37546608504675,-0.0181868229420618,
7.84979406923436));
#38375=CARTESIAN_POINT('Ctrl Pts',(-2.36724692977477,-0.814184073087101,
7.9034433517874));
#38376=CARTESIAN_POINT('Ctrl Pts',(-1.48345697628832,-2.36861723168749,
8.00953773956416));
#38377=CARTESIAN_POINT('Ctrl Pts',(1.16262680634646,-2.54151354917186,8.16687305523529));
#38378=CARTESIAN_POINT('Ctrl Pts',(2.76208455499713,-0.426475157784177,
8.3242083709064));
#38379=CARTESIAN_POINT('Ctrl Pts',(1.8750440359881,2.07248692819523,8.48154368657753));
#38380=CARTESIAN_POINT('Ctrl Pts',(-0.699958537943023,2.7057439570526,8.63887900224866));
#38381=CARTESIAN_POINT('Ctrl Pts',(-2.21235813584821,1.30404785948979,8.76122773735781));
#38382=CARTESIAN_POINT('Ctrl Pts',(-2.37146394347132,0.262432721575661,
8.83113136724327));
#38383=CARTESIAN_POINT('Ctrl Pts',(-2.36963954810708,0.00174754145538407,
8.84858989190503));
#38384=CARTESIAN_POINT('Origin',(0.,0.,-1.84858989190501));
#38385=CARTESIAN_POINT('',(-2.36973441944585,0.0017659640348839,6.65141010809499));
#38386=CARTESIAN_POINT('',(-2.36889628024144,-0.00137619754296547,6.84858989190503));
#38387=CARTESIAN_POINT('',(-2.37175,-1.78696459712734E-13,-1.84858989190501));
#38388=CARTESIAN_POINT('Ctrl Pts',(-2.36973441944585,0.00176596403488379,
6.65141010809499));
#38389=CARTESIAN_POINT('Ctrl Pts',(-2.36600087280351,-0.523508321396127,
6.68659209909035));
#38390=CARTESIAN_POINT('Ctrl Pts',(-1.93625564677593,-1.83636884117464,
6.77415359459022));
#38391=CARTESIAN_POINT('Ctrl Pts',(0.222416181733502,-2.78479173243988,
6.91409459459459));
#38392=CARTESIAN_POINT('Ctrl Pts',(2.4466042959518,-1.34857753576241,7.0712331081081));
#38393=CARTESIAN_POINT('Ctrl Pts',(2.47334911304448,1.29887571249989,7.22837162162162));
#38394=CARTESIAN_POINT('Ctrl Pts',(0.278629494786153,2.77973012269657,7.38551013513513));
#38395=CARTESIAN_POINT('Ctrl Pts',(-1.91543890246215,1.86818192765693,7.52652296395959));
#38396=CARTESIAN_POINT('Ctrl Pts',(-2.36597432596829,0.539167154048567,
7.61515628827954));
#38397=CARTESIAN_POINT('Ctrl Pts',(-2.37012643568897,-0.00188307441280247,
7.65141010809499));
#38398=CARTESIAN_POINT('Ctrl Pts',(-2.36889628024144,-0.0013761975429653,
6.84858989190503));
#38399=CARTESIAN_POINT('Ctrl Pts',(-2.37049735026751,-0.298256860301772,
6.86845677122545));
#38400=CARTESIAN_POINT('Ctrl Pts',(-2.18189218700624,-1.37689100842058,
6.94076875576958));
#38401=CARTESIAN_POINT('Ctrl Pts',(-0.57644849505612,-2.73472106868152,
7.06552584553741));
#38402=CARTESIAN_POINT('Ctrl Pts',(1.96716344393165,-1.98526073259378,7.22286116120855));
#38403=CARTESIAN_POINT('Ctrl Pts',(2.73988515609665,0.551381466653972,7.38019647687966));
#38404=CARTESIAN_POINT('Ctrl Pts',(1.04609303646807,2.5916561403346,7.53753179255079));
#38405=CARTESIAN_POINT('Ctrl Pts',(-1.56924738212969,2.3010974504224,7.69366293089257));
#38406=CARTESIAN_POINT('Ctrl Pts',(-2.3739704729535,0.759975650525201,7.79734896401065));
#38407=CARTESIAN_POINT('Ctrl Pts',(-2.37543174471759,-0.000319652972777509,
7.84858989190503));
#38408=CARTESIAN_POINT('Origin',(0.,0.,-1.84858989190501));
#38409=CARTESIAN_POINT('',(-2.37533640146812,-0.000487534612837604,5.65141010809499));
#38410=CARTESIAN_POINT('',(-2.3710171167516,0.00204493508413422,5.84858989190502));
#38411=CARTESIAN_POINT('',(-2.37175,-1.78696459712734E-13,-1.84858989190501));
#38412=CARTESIAN_POINT('Ctrl Pts',(-2.37533640146812,-0.000487534612837498,
5.65141010809499));
#38413=CARTESIAN_POINT('Ctrl Pts',(-2.3754150982357,-0.0280706202968775,
5.65326890089215));
#38414=CARTESIAN_POINT('Ctrl Pts',(-2.36258260410634,-0.832851216236821,
5.70750719819383));
#38415=CARTESIAN_POINT('Ctrl Pts',(-1.45646562934828,-2.38395507960311,
5.81412499999999));
#38416=CARTESIAN_POINT('Ctrl Pts',(1.18715361157964,-2.5288733170224,5.97126351351352));
#38417=CARTESIAN_POINT('Ctrl Pts',(2.76451839080433,-0.402457473451116,
6.12840202702702));
#38418=CARTESIAN_POINT('Ctrl Pts',(1.8589019956498,2.08542976904401,6.28554054054054));
#38419=CARTESIAN_POINT('Ctrl Pts',(-0.716306714602523,2.70026640197657,
6.44267905405405));
#38420=CARTESIAN_POINT('Ctrl Pts',(-2.21563200675447,1.29517183256302,6.5646355765722));
#38421=CARTESIAN_POINT('Ctrl Pts',(-2.37155943608083,0.258528340584143,
6.63421259458585));
#38422=CARTESIAN_POINT('Ctrl Pts',(-2.36973441944585,0.00176596403488379,
6.65141010809499));
#38423=CARTESIAN_POINT('Ctrl Pts',(-2.3710171167516,0.00204493508413416,
5.84858989190502));
#38424=CARTESIAN_POINT('Ctrl Pts',(-2.36609071130836,-0.572418580286349,
5.88711947321653));
#38425=CARTESIAN_POINT('Ctrl Pts',(-1.86927748327345,-1.93646185988882,
5.97809415975175));
#38426=CARTESIAN_POINT('Ctrl Pts',(0.401163844498212,-2.76587414046649,
6.12151395151068));
#38427=CARTESIAN_POINT('Ctrl Pts',(2.53076037597685,-1.18585163930103,6.2788492671818));
#38428=CARTESIAN_POINT('Ctrl Pts',(2.38210248511723,1.46170446446183,6.43618458285292));
#38429=CARTESIAN_POINT('Ctrl Pts',(0.0890157606711408,2.793397283841,6.59351989852405));
#38430=CARTESIAN_POINT('Ctrl Pts',(-1.98453634187054,1.75978107224967,6.73098833487474));
#38431=CARTESIAN_POINT('Ctrl Pts',(-2.36627080393209,0.485456441931073,
6.81601166600174));
#38432=CARTESIAN_POINT('Ctrl Pts',(-2.36889628024144,-0.0013761975429653,
6.84858989190503));
#38433=CARTESIAN_POINT('Origin',(0.,0.,-1.84858989190501));
#38434=CARTESIAN_POINT('',(-2.36864740940268,-0.0011676470311218,4.65141010809498));
#38435=CARTESIAN_POINT('',(-2.37471653528189,-0.00117837014130401,4.84858989190502));
#38436=CARTESIAN_POINT('',(-2.37175,-1.78696459712734E-13,-1.84858989190501));
#38437=CARTESIAN_POINT('Ctrl Pts',(-2.36864740940268,-0.00116764703112199,
4.65141010809498));
#38438=CARTESIAN_POINT('Ctrl Pts',(-2.37007090104248,-0.313795660845675,
4.67232520719846));
#38439=CARTESIAN_POINT('Ctrl Pts',(-2.16810014725707,-1.40760004764448,
4.74561981080643));
#38440=CARTESIAN_POINT('Ctrl Pts',(-0.525482821607704,-2.74379331497496,
4.87129391891892));
#38441=CARTESIAN_POINT('Ctrl Pts',(2.00035639160479,-1.95015595724574,5.02843243243243));
#38442=CARTESIAN_POINT('Ctrl Pts',(2.72955454106374,0.595034417816705,5.18557094594594));
#38443=CARTESIAN_POINT('Ctrl Pts',(1.0071746643292,2.60578839251754,5.34270945945947));
#38444=CARTESIAN_POINT('Ctrl Pts',(-1.58873507575841,2.28002578161798,5.49798918017579));
#38445=CARTESIAN_POINT('Ctrl Pts',(-2.37319747737008,0.7492017916888,5.60088939638765));
#38446=CARTESIAN_POINT('Ctrl Pts',(-2.37533640146812,-0.000487534612837498,
5.65141010809499));
#38447=CARTESIAN_POINT('Ctrl Pts',(-2.37471653528189,-0.00117837014130423,
4.84858989190502));
#38448=CARTESIAN_POINT('Ctrl Pts',(-2.37515017179056,-0.0716719020310164,
4.85333706998391));
#38449=CARTESIAN_POINT('Ctrl Pts',(-2.34054813360425,-0.920521113001663,
4.91052935328651));
#38450=CARTESIAN_POINT('Ctrl Pts',(-1.32208186928512,-2.46233460804071,
5.02016674181281));
#38451=CARTESIAN_POINT('Ctrl Pts',(1.32964132424929,-2.45826079574207,5.17750205748394));
#38452=CARTESIAN_POINT('Ctrl Pts',(2.78438780839412,-0.241198514719961,
5.33483737315506));
#38453=CARTESIAN_POINT('Ctrl Pts',(1.73255804842731,2.19299676239354,5.49217268882618));
#38454=CARTESIAN_POINT('Ctrl Pts',(-0.878964234485193,2.65300095467984,
5.64950800449731));
#38455=CARTESIAN_POINT('Ctrl Pts',(-2.25346115704322,1.19692341827648,5.76831373885692));
#38456=CARTESIAN_POINT('Ctrl Pts',(-2.37279636039799,0.20952086689332,5.83467436799283));
#38457=CARTESIAN_POINT('Ctrl Pts',(-2.3710171167516,0.00204493508413416,
5.84858989190502));
#38458=CARTESIAN_POINT('Origin',(0.,0.,-1.84858989190501));
#38459=CARTESIAN_POINT('',(-2.37165914320747,0.00205379600805495,3.65141010809498));
#38460=CARTESIAN_POINT('',(-2.36819322153198,-0.000653453332863235,3.84858989190502));
#38461=CARTESIAN_POINT('',(-2.37175,-1.78696459712734E-13,-1.84858989190501));
#38462=CARTESIAN_POINT('Ctrl Pts',(-2.37165914320747,0.0020537960080548,
3.65141010809498));
#38463=CARTESIAN_POINT('Ctrl Pts',(-2.36638740749304,-0.593495286532831,
3.69138151350476));
#38464=CARTESIAN_POINT('Ctrl Pts',(-1.83931642681201,-1.97778866762885,
3.78373242341905));
#38465=CARTESIAN_POINT('Ctrl Pts',(0.47257542983782,-2.75339906613161,3.92846283783783));
#38466=CARTESIAN_POINT('Ctrl Pts',(2.55822296043148,-1.12251023841371,4.08560135135135));
#38467=CARTESIAN_POINT('Ctrl Pts',(2.34617571991457,1.51657292659299,4.24273986486486));
#38468=CARTESIAN_POINT('Ctrl Pts',(0.0268861606557786,2.79353021925399,
4.39987837837838));
#38469=CARTESIAN_POINT('Ctrl Pts',(-2.00464048744226,1.72543877128143,4.53610179278842));
#38470=CARTESIAN_POINT('Ctrl Pts',(-2.36650592693501,0.469145905762286,
4.61994570269395));
#38471=CARTESIAN_POINT('Ctrl Pts',(-2.36864740940268,-0.00116764703112199,
4.65141010809498));
#38472=CARTESIAN_POINT('Ctrl Pts',(-2.36819322153198,-0.000653453332863235,
3.84858989190502));
#38473=CARTESIAN_POINT('Ctrl Pts',(-2.36907284142701,-0.350739660290616,
3.871999771975));
#38474=CARTESIAN_POINT('Ctrl Pts',(-2.13320735842129,-1.48399610964751,
3.94785475726868));
#38475=CARTESIAN_POINT('Ctrl Pts',(-0.392663608746353,-2.76709368867159,
4.07615484778607));
#38476=CARTESIAN_POINT('Ctrl Pts',(2.09526330020315,-1.8495577562663,4.23349016345719));
#38477=CARTESIAN_POINT('Ctrl Pts',(2.69698125586998,0.732996791565816,4.39082547912832));
#38478=CARTESIAN_POINT('Ctrl Pts',(0.870808554093777,2.65568911080063,4.54816079479944));
#38479=CARTESIAN_POINT('Ctrl Pts',(-1.66053522846232,2.20178445767042,4.70074893239168));
#38480=CARTESIAN_POINT('Ctrl Pts',(-2.37035951259304,0.707115123883991,
4.8008919647602));
#38481=CARTESIAN_POINT('Ctrl Pts',(-2.37471653528189,-0.00117837014130423,
4.84858989190502));
#38482=CARTESIAN_POINT('Origin',(0.,0.,-1.84858989190501));
#38483=CARTESIAN_POINT('',(-2.37406517885066,-0.00153607482357252,2.65141010809498));
#38484=CARTESIAN_POINT('',(-2.37255724078598,0.00199178475905649,2.84858989190502));
#38485=CARTESIAN_POINT('',(-2.37175,-1.78696459712734E-13,-1.84858989190501));
#38486=CARTESIAN_POINT('Ctrl Pts',(-2.37406517885066,-0.00153607482357281,
2.65141010809498));
#38487=CARTESIAN_POINT('Ctrl Pts',(-2.37481281249436,-0.100330398866114,
2.65805831530656));
#38488=CARTESIAN_POINT('Ctrl Pts',(-2.32469515905834,-0.976735840432517,
2.71708602702265));
#38489=CARTESIAN_POINT('Ctrl Pts',(-1.23560715428754,-2.50555554774625,
2.82849324324324));
#38490=CARTESIAN_POINT('Ctrl Pts',(1.41031161531747,-2.41154623133624,2.98563175675675));
#38491=CARTESIAN_POINT('Ctrl Pts',(2.78954424185296,-0.151581281506301,
3.14277027027027));
#38492=CARTESIAN_POINT('Ctrl Pts',(1.66331845351111,2.24452793077997,3.29990878378378));
#38493=CARTESIAN_POINT('Ctrl Pts',(-0.956834235921451,2.62469088021855,
3.45704729729729));
#38494=CARTESIAN_POINT('Ctrl Pts',(-2.26971028444252,1.15040938517441,3.57421440540103));
#38495=CARTESIAN_POINT('Ctrl Pts',(-2.37329561854466,0.186926755969883,
3.63900200900026));
#38496=CARTESIAN_POINT('Ctrl Pts',(-2.37165914320747,0.0020537960080548,
3.65141010809498));
#38497=CARTESIAN_POINT('Ctrl Pts',(-2.37255724078598,0.00199178475905658,
2.84858989190502));
#38498=CARTESIAN_POINT('Ctrl Pts',(-2.36697397570993,-0.624252704055323,
2.89066247396608));
#38499=CARTESIAN_POINT('Ctrl Pts',(-1.79321255273579,-2.04018921676783,
2.98518016125086));
#38500=CARTESIAN_POINT('Ctrl Pts',(0.584848394656438,-2.73293698550247,
3.13214295375933));
#38501=CARTESIAN_POINT('Ctrl Pts',(2.60425579784155,-1.01431944186932,3.28947826943046));
#38502=CARTESIAN_POINT('Ctrl Pts',(2.27924634057658,1.61741407950708,3.44681358510158));
#38503=CARTESIAN_POINT('Ctrl Pts',(-0.0975982492034651,2.79311059143494,
3.6041489007727));
#38504=CARTESIAN_POINT('Ctrl Pts',(-2.04600507844241,1.65356799864077,3.73807433637385));
#38505=CARTESIAN_POINT('Ctrl Pts',(-2.36710223082098,0.433557734928271,
3.81955466675129));
#38506=CARTESIAN_POINT('Ctrl Pts',(-2.36819322153198,-0.000653453332863235,
3.84858989190502));
#38507=CARTESIAN_POINT('Origin',(0.,0.,-1.84858989190501));
#38508=CARTESIAN_POINT('',(-2.36804188512505,-0.000112073902353324,1.65141010809498));
#38509=CARTESIAN_POINT('',(-2.37344137975612,-0.00178937704920473,1.84858989190502));
#38510=CARTESIAN_POINT('',(-2.37175,-1.78696459712734E-13,-1.84858989190501));
#38511=CARTESIAN_POINT('Ctrl Pts',(-2.36804188512505,-0.000112073902353224,
1.65141010809498));
#38512=CARTESIAN_POINT('Ctrl Pts',(-2.36821023678956,-0.384577180330964,
1.67711462161287));
#38513=CARTESIAN_POINT('Ctrl Pts',(-2.09930421630608,-1.55226751145704,
1.75519863963526));
#38514=CARTESIAN_POINT('Ctrl Pts',(-0.275973625536248,-2.77999224892802,
1.88566216216216));
#38515=CARTESIAN_POINT('Ctrl Pts',(2.16802781286073,-1.76187209738162,2.04280067567567));
#38516=CARTESIAN_POINT('Ctrl Pts',(2.66479327803676,0.838697048159531,2.19993918918919));
#38517=CARTESIAN_POINT('Ctrl Pts',(0.76814623510466,2.68597898024514,2.3570777027027));
#38518=CARTESIAN_POINT('Ctrl Pts',(-1.70898688612053,2.14473275169325,2.50756800900463));
#38519=CARTESIAN_POINT('Ctrl Pts',(-2.36892240045369,0.678044518839718,
2.60567881080206));
#38520=CARTESIAN_POINT('Ctrl Pts',(-2.37406517885066,-0.00153607482357281,
2.65141010809498));
#38521=CARTESIAN_POINT('Ctrl Pts',(-2.37344137975612,-0.00178937704920463,
1.84858989190502));
#38522=CARTESIAN_POINT('Ctrl Pts',(-2.37447812169567,-0.12506848067989,
1.85688007073346));
#38523=CARTESIAN_POINT('Ctrl Pts',(-2.31006431944847,-1.02714724785255,
1.91761535478561));
#38524=CARTESIAN_POINT('Ctrl Pts',(-1.15481219883121,-2.54507342378116,
2.03079574406147));
#38525=CARTESIAN_POINT('Ctrl Pts',(1.49072764255621,-2.36404822464922,2.18813105973259));
#38526=CARTESIAN_POINT('Ctrl Pts',(2.79427705549031,-0.0548463935276453,
2.34546637540372));
#38527=CARTESIAN_POINT('Ctrl Pts',(1.5823475414007,2.30372918060613,2.50280169107483));
#38528=CARTESIAN_POINT('Ctrl Pts',(-1.05405113312049,2.58842974112365,2.66013700674597));
#38529=CARTESIAN_POINT('Ctrl Pts',(-2.29031280961247,1.08993341565411,2.77539974035602));
#38530=CARTESIAN_POINT('Ctrl Pts',(-2.37393373216083,0.15638533864836,2.83821736874238));
#38531=CARTESIAN_POINT('Ctrl Pts',(-2.37255724078598,0.00199178475905658,
2.84858989190502));
#38532=CARTESIAN_POINT('Origin',(0.,0.,-1.84858989190501));
#38533=CARTESIAN_POINT('',(-2.37366757034868,0.00184471646948807,0.651410108094983));
#38534=CARTESIAN_POINT('',(-2.36802324146013,0.000186122305323028,0.848589891905023));
#38535=CARTESIAN_POINT('',(-2.37175,-1.78696459712734E-13,-1.84858989190501));
#38536=CARTESIAN_POINT('Ctrl Pts',(-2.37366757034868,0.001844716469488,
0.651410108094984));
#38537=CARTESIAN_POINT('Ctrl Pts',(-2.36827887140227,-0.663567421798888,
0.696170927919177));
#38538=CARTESIAN_POINT('Ctrl Pts',(-1.73206830317985,-2.11713322740477,
0.793311252247876));
#38539=CARTESIAN_POINT('Ctrl Pts',(0.718910407331439,-2.69944634094777,
0.942831081081078));
#38540=CARTESIAN_POINT('Ctrl Pts',(2.64899289676255,-0.887370898887054,
1.09996959459459));
#38541=CARTESIAN_POINT('Ctrl Pts',(2.19990031581894,1.72195501972256,1.25710810810811));
#38542=CARTESIAN_POINT('Ctrl Pts',(-0.225079684819506,2.78455874530281,
1.41424662162162));
#38543=CARTESIAN_POINT('Ctrl Pts',(-2.08428517335687,1.58152664346482,1.54568062161725));
#38544=CARTESIAN_POINT('Ctrl Pts',(-2.36786717732013,0.39886856587965,1.62473511710837));
#38545=CARTESIAN_POINT('Ctrl Pts',(-2.36804188512505,-0.000112073902353224,
1.65141010809498));
#38546=CARTESIAN_POINT('Ctrl Pts',(-2.36802324146013,0.000186122305323062,
0.848589891905023));
#38547=CARTESIAN_POINT('Ctrl Pts',(-2.36776001721126,-0.402962357372647,
0.87554277272455));
#38548=CARTESIAN_POINT('Ctrl Pts',(-2.0797505690667,-1.59092671500009,0.954940758767785));
#38549=CARTESIAN_POINT('Ctrl Pts',(-0.207121339063888,-2.78711087979173,
1.08678385003473));
#38550=CARTESIAN_POINT('Ctrl Pts',(2.21401803077907,-1.70561830406782,1.24411916570585));
#38551=CARTESIAN_POINT('Ctrl Pts',(2.64205485235054,0.911349150745493,1.40145448137697));
#38552=CARTESIAN_POINT('Ctrl Pts',(0.691640660298454,2.70787919402874,1.5587897970481));
#38553=CARTESIAN_POINT('Ctrl Pts',(-1.74582592441822,2.10050088985172,1.70783493389078));
#38554=CARTESIAN_POINT('Ctrl Pts',(-2.36791951286044,0.654816452515466,
1.80443496550976));
#38555=CARTESIAN_POINT('Ctrl Pts',(-2.37344137975612,-0.00178937704920463,
1.84858989190502));
#38556=CARTESIAN_POINT('Origin',(0.,0.,11.5));
#38557=CARTESIAN_POINT('',(-2.86997293948595,0.000709208322249463,11.1339652973708));
#38558=CARTESIAN_POINT('Ctrl Pts',(-0.439445221994061,2.3306835819919,11.62825));
#38559=CARTESIAN_POINT('Ctrl Pts',(-0.359483020814685,2.34931149018937,
11.6247602761445));
#38560=CARTESIAN_POINT('Ctrl Pts',(-0.27871400731898,2.36341693162049,11.6212847858384));
#38561=CARTESIAN_POINT('Ctrl Pts',(-0.197463562604575,2.37318447045242,
11.6178187998135));
#38562=CARTESIAN_POINT('Ctrl Pts',(-0.114065564321399,2.38321017787593,
11.614261203328));
#38563=CARTESIAN_POINT('Ctrl Pts',(-0.0301595928545948,2.38866567182183,
11.6107136201843));
#38564=CARTESIAN_POINT('Ctrl Pts',(0.0539178478306465,2.38969830818771,
11.6071709361129));
#38565=CARTESIAN_POINT('Ctrl Pts',(0.0934462943689916,2.39018379527021,
11.6055053668855));
#38566=CARTESIAN_POINT('Ctrl Pts',(0.133012786809523,2.38969093626847,11.6038408805234));
#38567=CARTESIAN_POINT('Ctrl Pts',(0.172582728329755,2.38823118545469,11.6021769455617));
#38568=CARTESIAN_POINT('Ctrl Pts',(0.196983674678661,2.38733102488025,11.6011508741002));
#38569=CARTESIAN_POINT('Ctrl Pts',(0.221385934120707,2.38606314465001,11.6001250123152));
#38570=CARTESIAN_POINT('Ctrl Pts',(0.24578137026875,2.38442977721171,11.5990992355836));
#38571=CARTESIAN_POINT('Ctrl Pts',(0.261730484740349,2.38336192320454,11.5984286088969));
#38572=CARTESIAN_POINT('Ctrl Pts',(0.277677591321838,2.38213767553654,11.597757980196));
#38573=CARTESIAN_POINT('Ctrl Pts',(0.293603734342933,2.38075929535175,11.5970880163414));
#38574=CARTESIAN_POINT('Ctrl Pts',(0.379341030417818,2.37333888038685,11.5934813119885));
#38575=CARTESIAN_POINT('Ctrl Pts',(0.464583014225527,2.36144918428767,11.5898891320915));
#38576=CARTESIAN_POINT('Ctrl Pts',(0.548977057540434,2.34525221307984,11.5863062427765));
#38577=CARTESIAN_POINT('Ctrl Pts',(0.63410785152571,2.32891384410355,11.5826920752337));
#38578=CARTESIAN_POINT('Ctrl Pts',(0.718376786391574,2.30819252148602,11.5790873611926));
#38579=CARTESIAN_POINT('Ctrl Pts',(0.801421129360431,2.28320149524268,11.5754867285058));
#38580=CARTESIAN_POINT('Ctrl Pts',(0.851520069054253,2.26812492443856,11.5733145410529));
#38581=CARTESIAN_POINT('Ctrl Pts',(0.901173245121242,2.25149340059607,11.5711438389925));
#38582=CARTESIAN_POINT('Ctrl Pts',(0.950298631716725,2.23332291784394,11.5689734428101));
#38583=CARTESIAN_POINT('Ctrl Pts',(0.963508179039198,2.22843697457875,11.5683898351671));
#38584=CARTESIAN_POINT('Ctrl Pts',(0.976678902975083,2.22343988211883,11.5678062771152));
#38585=CARTESIAN_POINT('Ctrl Pts',(0.989796896482515,2.2183369213822,11.5672232951128));
#38586=CARTESIAN_POINT('Ctrl Pts',(1.0715488401239,2.18653503351653,11.5635901242489));
#38587=CARTESIAN_POINT('Ctrl Pts',(1.15137916677557,2.15057972741051,11.5599737688071));
#38588=CARTESIAN_POINT('Ctrl Pts',(1.22892868995964,2.11061806082819,11.5563689172299));
#38589=CARTESIAN_POINT('Ctrl Pts',(1.30609743699769,2.07085261014462,11.5527817658451));
#38590=CARTESIAN_POINT('Ctrl Pts',(1.38100867140758,2.02711976610499,11.5492060056319));
#38591=CARTESIAN_POINT('Ctrl Pts',(1.45329568150197,1.97951483102432,11.5456364028898));
#38592=CARTESIAN_POINT('Ctrl Pts',(1.51120974849783,1.94137526215855,11.5427765500327));
#38593=CARTESIAN_POINT('Ctrl Pts',(1.56743935204678,1.90074932215926,11.5399206494764));
#38594=CARTESIAN_POINT('Ctrl Pts',(1.621783737959,1.85766460010194,11.5370660098083));
#38595=CARTESIAN_POINT('Ctrl Pts',(1.64895593091511,1.83612223907328,11.5356386899743));
#38596=CARTESIAN_POINT('Ctrl Pts',(1.67565661487015,1.81396489287275,11.5342116853624));
#38597=CARTESIAN_POINT('Ctrl Pts',(1.70185926132131,1.79119431574093,11.532784659546));
#38598=CARTESIAN_POINT('Ctrl Pts',(1.71882166156475,1.77645368090452,11.5318608680083));
#38599=CARTESIAN_POINT('Ctrl Pts',(1.73557532962421,1.76145603809249,11.5309370675846));
#38600=CARTESIAN_POINT('Ctrl Pts',(1.75211281381839,1.74620161928424,11.5300131670071));
#38601=CARTESIAN_POINT('Ctrl Pts',(1.76112158754248,1.73789179381609,11.529509873329));
#38602=CARTESIAN_POINT('Ctrl Pts',(1.77006808708219,1.72950393138366,11.5290064421071));
#38603=CARTESIAN_POINT('Ctrl Pts',(1.77894146971999,1.72104732904951,11.5285034067769));
#38604=CARTESIAN_POINT('Ctrl Pts',(1.83933200754334,1.66349331791721,11.5250798449438));
#38605=CARTESIAN_POINT('Ctrl Pts',(1.8963984276916,1.60270624192685,11.5216713230637));
#38606=CARTESIAN_POINT('Ctrl Pts',(1.95011819953022,1.53907807970147,11.5182734051049));
#38607=CARTESIAN_POINT('Ctrl Pts',(2.00542449571231,1.47357076525995,11.5147751352761));
#38608=CARTESIAN_POINT('Ctrl Pts',(2.05718398574646,1.40505149787053,11.511288104956));
#38609=CARTESIAN_POINT('Ctrl Pts',(2.10533946111886,1.3339039115796,11.5078074733588));
#38610=CARTESIAN_POINT('Ctrl Pts',(2.15154257592138,1.26564085173229,11.5044679565119));
#38611=CARTESIAN_POINT('Ctrl Pts',(2.19442802485129,1.19495736996561,11.5011343300606));
#38612=CARTESIAN_POINT('Ctrl Pts',(2.23391281993103,1.12216394079048,11.4978023184486));
#38613=CARTESIAN_POINT('Ctrl Pts',(2.25118741777841,1.09031681552637,11.4963445633684));
#38614=CARTESIAN_POINT('Ctrl Pts',(2.26781067606573,1.05806553560368,11.4948871173785));
#38615=CARTESIAN_POINT('Ctrl Pts',(2.28377353610697,1.02543493097626,11.4934296224428));
#38616=CARTESIAN_POINT('Ctrl Pts',(2.29326703470383,1.00602872191068,11.4925628149854));
#38617=CARTESIAN_POINT('Ctrl Pts',(2.30252692730832,0.986488335264957,11.4916959902159));
#38618=CARTESIAN_POINT('Ctrl Pts',(2.31155107931692,0.966818908506685,11.4908290728209));
#38619=CARTESIAN_POINT('Ctrl Pts',(2.31863529945096,0.951377840034761,11.490148517611));
#38620=CARTESIAN_POINT('Ctrl Pts',(2.32557538886546,0.935854346809815,11.4894677807698));
#38621=CARTESIAN_POINT('Ctrl Pts',(2.33236053374086,0.920273937348818,11.4887878255595));
#38622=CARTESIAN_POINT('Ctrl Pts',(2.36796902716184,0.838507826532316,11.4852194152932));
#38623=CARTESIAN_POINT('Ctrl Pts',(2.39937221583678,0.755052917299449,11.4816670269197));
#38624=CARTESIAN_POINT('Ctrl Pts',(2.42650990964853,0.670313949715511,11.4781256336386));
#38625=CARTESIAN_POINT('Ctrl Pts',(2.45395171326163,0.584625382258507,11.4745445548773));
#38626=CARTESIAN_POINT('Ctrl Pts',(2.47703230477293,0.497622920338958,11.470974719015));
#38627=CARTESIAN_POINT('Ctrl Pts',(2.49564463758615,0.409696684762178,11.4674109283565));
#38628=CARTESIAN_POINT('Ctrl Pts',(2.51256694354607,0.329754279086013,11.464170735066));
#38629=CARTESIAN_POINT('Ctrl Pts',(2.52579526118549,0.24904737731457,11.460935538995));
#38630=CARTESIAN_POINT('Ctrl Pts',(2.53521313973642,0.167858755145902,11.4577014336506));
#38631=CARTESIAN_POINT('Ctrl Pts',(2.53942638325848,0.131537684050459,11.4562546032081));
#38632=CARTESIAN_POINT('Ctrl Pts',(2.54287653840534,0.0951201284473648,
11.4548079910601));
#38633=CARTESIAN_POINT('Ctrl Pts',(2.54555076253572,0.0586312673898904,
11.4533612474409));
#38634=CARTESIAN_POINT('Ctrl Pts',(2.54678080763582,0.0418477284777441,
11.4526957983935));
#38635=CARTESIAN_POINT('Ctrl Pts',(2.54784667039524,0.0250491043820508,
11.4520303215313));
#38636=CARTESIAN_POINT('Ctrl Pts',(2.54874698931854,0.00823785327091157,
11.4513647828174));
#38637=CARTESIAN_POINT('Ctrl Pts',(2.54950258918657,-0.00587112388394168,
11.4508062241208));
#38638=CARTESIAN_POINT('Ctrl Pts',(2.55014158604825,-0.0199907301096276,
11.4502475533557));
#38639=CARTESIAN_POINT('Ctrl Pts',(2.55066270854233,-0.0341027028361791,
11.4496894146469));
#38640=CARTESIAN_POINT('Ctrl Pts',(2.55400035119776,-0.124485909584641,
11.4461146935723));
#38641=CARTESIAN_POINT('Ctrl Pts',(2.55251590030915,-0.214700787372498,
11.4425560101414));
#38642=CARTESIAN_POINT('Ctrl Pts',(2.54610973516166,-0.304360270645855,
11.4390083150826));
#38643=CARTESIAN_POINT('Ctrl Pts',(2.53992350143221,-0.390941635131681,
11.4355824166973));
#38644=CARTESIAN_POINT('Ctrl Pts',(2.52914771427487,-0.477005973362024,
11.4321667651471));
#38645=CARTESIAN_POINT('Ctrl Pts',(2.51364702202946,-0.56221151242787,11.4287568135539));
#38646=CARTESIAN_POINT('Ctrl Pts',(2.4978416408886,-0.649091891634602,11.4252798343488));
#38647=CARTESIAN_POINT('Ctrl Pts',(2.47712400969773,-0.735080204165537,
11.4218087813851));
#38648=CARTESIAN_POINT('Ctrl Pts',(2.45176245019841,-0.819915179815436,
11.4183388343531));
#38649=CARTESIAN_POINT('Ctrl Pts',(2.43759878319083,-0.867292958210081,
11.4164009734618));
#38650=CARTESIAN_POINT('Ctrl Pts',(2.42198578511571,-0.914310849766526,
11.4144634574981));
#38651=CARTESIAN_POINT('Ctrl Pts',(2.40496360252248,-0.960921226687823,
11.4125254468584));
#38652=CARTESIAN_POINT('Ctrl Pts',(2.39839032938233,-0.978920254544038,
11.4117770661373));
#38653=CARTESIAN_POINT('Ctrl Pts',(2.39160484182306,-0.996863365779891,
11.4110284061025));
#38654=CARTESIAN_POINT('Ctrl Pts',(2.38462104532031,-1.01471861919519,11.4102806421704));
#38655=CARTESIAN_POINT('Ctrl Pts',(2.35196925304181,-1.09819843212604,11.4067845734384));
#38656=CARTESIAN_POINT('Ctrl Pts',(2.31495075727319,-1.17986515814379,11.4033036769767));
#38657=CARTESIAN_POINT('Ctrl Pts',(2.27389075093231,-1.25946542646749,11.3998332297369));
#38658=CARTESIAN_POINT('Ctrl Pts',(2.23207387867294,-1.34053297976178,11.3962988111666));
#38659=CARTESIAN_POINT('Ctrl Pts',(2.18606471254661,-1.41945796930655,11.3927752305933));
#38660=CARTESIAN_POINT('Ctrl Pts',(2.13615274225743,-1.49596025824322,11.3892574989426));
#38661=CARTESIAN_POINT('Ctrl Pts',(2.08602408315185,-1.57279467573233,11.385724495342));
#38662=CARTESIAN_POINT('Ctrl Pts',(2.03195810671375,-1.64718611516111,11.3821973915595));
#38663=CARTESIAN_POINT('Ctrl Pts',(1.97420160691916,-1.71882633760539,11.3786711332592));
#38664=CARTESIAN_POINT('Ctrl Pts',(1.95240508667088,-1.74586238661548,11.377340371168));
#38665=CARTESIAN_POINT('Ctrl Pts',(1.93008253152955,-1.77250629512415,11.3760097294909));
#38666=CARTESIAN_POINT('Ctrl Pts',(1.90724574604483,-1.79874022848494,11.3746789365696));
#38667=CARTESIAN_POINT('Ctrl Pts',(1.89585779635524,-1.81182222347379,11.3740153141501));
#38668=CARTESIAN_POINT('Ctrl Pts',(1.8843419621495,-1.82480225835256,11.3733516541209));
#38669=CARTESIAN_POINT('Ctrl Pts',(1.87269964124851,-1.83767804526001,11.3726879227956));
#38670=CARTESIAN_POINT('Ctrl Pts',(1.86326625859819,-1.8481108640987,11.3721501235353));
#38671=CARTESIAN_POINT('Ctrl Pts',(1.8537496389451,-1.8584753407347,11.3716122696922));
#38672=CARTESIAN_POINT('Ctrl Pts',(1.8441608279676,-1.86875948192732,11.3710749125616));
#38673=CARTESIAN_POINT('Ctrl Pts',(1.78056218360928,-1.93696996597738,11.3675108434478));
#38674=CARTESIAN_POINT('Ctrl Pts',(1.71368420494736,-2.00176842633816,11.3639624618779));
#38675=CARTESIAN_POINT('Ctrl Pts',(1.64382533951827,-2.06287172496906,11.3604247664903));
#38676=CARTESIAN_POINT('Ctrl Pts',(1.57423141411002,-2.12374328910052,11.3569004878264));
#38677=CARTESIAN_POINT('Ctrl Pts',(1.50167852811227,-2.18094842953722,11.3533868144436));
#38678=CARTESIAN_POINT('Ctrl Pts',(1.42641996197867,-2.2341772386581,11.3498788016679));
#38679=CARTESIAN_POINT('Ctrl Pts',(1.3516762241841,-2.28704192046701,11.3463947864845));
#38680=CARTESIAN_POINT('Ctrl Pts',(1.27426307539374,-2.33598522008376,11.342916354727));
#38681=CARTESIAN_POINT('Ctrl Pts',(1.19439676647842,-2.38066281826916,11.339438662505));
#38682=CARTESIAN_POINT('Ctrl Pts',(1.15339338620205,-2.40360030684365,11.3376532145659));
#38683=CARTESIAN_POINT('Ctrl Pts',(1.11174294293827,-2.42541271468527,11.3358679615534));
#38684=CARTESIAN_POINT('Ctrl Pts',(1.06947220915485,-2.44604826098259,11.334082247983));
#38685=CARTESIAN_POINT('Ctrl Pts',(1.05124776879456,-2.45494499044852,11.3333123623541));
#38686=CARTESIAN_POINT('Ctrl Pts',(1.0329023157667,-2.46362538871231,11.3325421557385));
#38687=CARTESIAN_POINT('Ctrl Pts',(1.01446903163988,-2.47207123914098,11.3317728670993));
#38688=CARTESIAN_POINT('Ctrl Pts',(0.992379075227472,-2.48219252119531,
11.3308509720972));
#38689=CARTESIAN_POINT('Ctrl Pts',(0.970156538466361,-2.49198036655811,
11.3299301186847));
#38690=CARTESIAN_POINT('Ctrl Pts',(0.94780620569595,-2.50142961190602,11.3290102203308));
#38691=CARTESIAN_POINT('Ctrl Pts',(0.865790439448149,-2.53610413356231,
11.3256346031023));
#38692=CARTESIAN_POINT('Ctrl Pts',(0.78205610317221,-2.56622272676918,11.3222718463403));
#38693=CARTESIAN_POINT('Ctrl Pts',(0.696974578785958,-2.59191739767486,
11.318917674299));
#38694=CARTESIAN_POINT('Ctrl Pts',(0.609579162327931,-2.61831086536073,
11.3154722816062));
#38695=CARTESIAN_POINT('Ctrl Pts',(0.520761565645775,-2.64003666842693,
11.3120359469267));
#38696=CARTESIAN_POINT('Ctrl Pts',(0.430899300361841,-2.65718927641842,
11.3086040360895));
#38697=CARTESIAN_POINT('Ctrl Pts',(0.343209845834361,-2.67392714557567,
11.3052551066101));
#38698=CARTESIAN_POINT('Ctrl Pts',(0.25452479015491,-2.6863100783274,11.3019103896282));
#38699=CARTESIAN_POINT('Ctrl Pts',(0.165183352753207,-2.69438132192965,
11.2985655790638));
#38700=CARTESIAN_POINT('Ctrl Pts',(0.137834848150192,-2.69685202812409,
11.2975416917191));
#38701=CARTESIAN_POINT('Ctrl Pts',(0.110424801620538,-2.69891839950379,
11.2965177956053));
#38702=CARTESIAN_POINT('Ctrl Pts',(0.08296290180991,-2.70058085938097,11.2954937672061));
#38703=CARTESIAN_POINT('Ctrl Pts',(0.0669684788561147,-2.70154911309258,
11.2948973502268));
#38704=CARTESIAN_POINT('Ctrl Pts',(0.0509564666454086,-2.70238034652659,
11.2943008883741));
#38705=CARTESIAN_POINT('Ctrl Pts',(0.0349287839010169,-2.70307458363613,
11.2937043572455));
#38706=CARTESIAN_POINT('Ctrl Pts',(0.0206834334719444,-2.70369161924033,
11.293174162388));
#38707=CARTESIAN_POINT('Ctrl Pts',(0.00643409067270473,-2.70420004997344,
11.2926442249703));
#38708=CARTESIAN_POINT('Ctrl Pts',(-0.00781400179505987,-2.70460019597085,
11.2921146711228));
#38709=CARTESIAN_POINT('Ctrl Pts',(-0.101952151334104,-2.70724398873305,
11.2886158715889));
#38710=CARTESIAN_POINT('Ctrl Pts',(-0.196088226677417,-2.7051673117304,
11.2851318105594));
#38711=CARTESIAN_POINT('Ctrl Pts',(-0.289825667638303,-2.6984813516168,
11.2816577549713));
#38712=CARTESIAN_POINT('Ctrl Pts',(-0.384631538117472,-2.69171918420471,
11.2781441017209));
#38713=CARTESIAN_POINT('Ctrl Pts',(-0.479030586990251,-2.68024208441543,
11.2746406832979));
#38714=CARTESIAN_POINT('Ctrl Pts',(-0.57262152425153,-2.66411259564997,
11.2711426029439));
#38715=CARTESIAN_POINT('Ctrl Pts',(-0.666559717691804,-2.64792326065578,
11.2676315434484));
#38716=CARTESIAN_POINT('Ctrl Pts',(-0.759684799865766,-2.62704692522732,
11.2641258617076));
#38717=CARTESIAN_POINT('Ctrl Pts',(-0.851585181919148,-2.6014943492988,
11.2606206062542));
#38718=CARTESIAN_POINT('Ctrl Pts',(-0.886047825189167,-2.59191213332561,
11.2593061354592));
#38719=CARTESIAN_POINT('Ctrl Pts',(-0.920338108563248,-2.58167179563189,
11.2579917246108));
#38720=CARTESIAN_POINT('Ctrl Pts',(-0.95443366677234,-2.57077201863537,
11.2566771125966));
#38721=CARTESIAN_POINT('Ctrl Pts',(-0.974280480974564,-2.5644273256531,
11.255911885049));
#38722=CARTESIAN_POINT('Ctrl Pts',(-0.99406130744013,-2.55785917358927,
11.2551465893396));
#38723=CARTESIAN_POINT('Ctrl Pts',(-1.01377165408274,-2.55106714297751,
11.2543811739687));
#38724=CARTESIAN_POINT('Ctrl Pts',(-1.02736841414217,-2.54638180627496,
11.2538531685848));
#38725=CARTESIAN_POINT('Ctrl Pts',(-1.04092225787931,-2.54159315279905,
11.253325470206));
#38726=CARTESIAN_POINT('Ctrl Pts',(-1.05443025528497,-2.53670205395909,
11.252798124302));
#38727=CARTESIAN_POINT('Ctrl Pts',(-1.14463510839177,-2.50403985843604,
11.2492765690056));
#38728=CARTESIAN_POINT('Ctrl Pts',(-1.23281912858369,-2.46680540724472,
11.2457698275395));
#38729=CARTESIAN_POINT('Ctrl Pts',(-1.31858159439492,-2.42506535814129,
11.242273074989));
#38730=CARTESIAN_POINT('Ctrl Pts',(-1.40311199337542,-2.38392494816353,
11.2388265569179));
#38731=CARTESIAN_POINT('Ctrl Pts',(-1.48529083212456,-2.33840727081253,
11.2353897428216));
#38732=CARTESIAN_POINT('Ctrl Pts',(-1.56472199239298,-2.28852750879454,
11.2319580127567));
#38733=CARTESIAN_POINT('Ctrl Pts',(-1.58551758994019,-2.27546866069046,
11.2310595633688));
#38734=CARTESIAN_POINT('Ctrl Pts',(-1.60612474663732,-2.26211056997792,
11.230161462454));
#38735=CARTESIAN_POINT('Ctrl Pts',(-1.62653609083598,-2.2484529714829,11.2292636271078));
#38736=CARTESIAN_POINT('Ctrl Pts',(-1.70441968299709,-2.19633965543995,
11.225837755629));
#38737=CARTESIAN_POINT('Ctrl Pts',(-1.77945485532057,-2.13986885585993,
11.222415750716));
#38738=CARTESIAN_POINT('Ctrl Pts',(-1.85149349468849,-2.07939019092048,
11.2189930066095));
#38739=CARTESIAN_POINT('Ctrl Pts',(-1.8748645479439,-2.05976946915896,11.2178825867641));
#38740=CARTESIAN_POINT('Ctrl Pts',(-1.89791995295043,-2.03972659946025,
11.2167720891179));
#38741=CARTESIAN_POINT('Ctrl Pts',(-1.92065386067013,-2.01927267290743,
11.2156613564032));
#38742=CARTESIAN_POINT('Ctrl Pts',(-1.9316413592642,-2.00938710936888,11.2151245294621));
#38743=CARTESIAN_POINT('Ctrl Pts',(-1.94255421950186,-1.99940498570623,
11.2145876221361));
#38744=CARTESIAN_POINT('Ctrl Pts',(-1.95338011991677,-1.98933864610605,
11.2140511999421));
#38745=CARTESIAN_POINT('Ctrl Pts',(-2.02242773931489,-1.92513550744723,
11.2106298978731));
#38746=CARTESIAN_POINT('Ctrl Pts',(-2.08805585991204,-1.85740773886018,
11.2072227031525));
#38747=CARTESIAN_POINT('Ctrl Pts',(-2.15015903930769,-1.7865606665237,11.2038251982962));
#38748=CARTESIAN_POINT('Ctrl Pts',(-2.21349481278046,-1.71430745552261,
11.2003602613952));
#38749=CARTESIAN_POINT('Ctrl Pts',(-2.27316487566809,-1.63880924004706,
11.1969054028151));
#38750=CARTESIAN_POINT('Ctrl Pts',(-2.32902567586957,-1.56045035084564,
11.1934559367882));
#38751=CARTESIAN_POINT('Ctrl Pts',(-2.38527990190259,-1.48153958249049,
11.1899821762823));
#38752=CARTESIAN_POINT('Ctrl Pts',(-2.43767154642151,-1.39972691196139,
11.1865138845562));
#38753=CARTESIAN_POINT('Ctrl Pts',(-2.48601414345046,-1.31537014370798,
11.1830462761383));
#38754=CARTESIAN_POINT('Ctrl Pts',(-2.51324863986033,-1.26784654664574,
11.1810927491288));
#38755=CARTESIAN_POINT('Ctrl Pts',(-2.53919729042327,-1.21951494628862,
11.1791394389872));
#38756=CARTESIAN_POINT('Ctrl Pts',(-2.56382026308967,-1.17043597842562,
11.1771854900701));
#38757=CARTESIAN_POINT('Ctrl Pts',(-2.57043915220293,-1.15724308533024,
11.1766602500274));
#38758=CARTESIAN_POINT('Ctrl Pts',(-2.57696321367054,-1.1439941193146,11.1761348825453));
#38759=CARTESIAN_POINT('Ctrl Pts',(-2.58338840616944,-1.13069688731366,
11.175609633533));
#38760=CARTESIAN_POINT('Ctrl Pts',(-2.62620034331217,-1.04209561027884,
11.172109827464));
#38761=CARTESIAN_POINT('Ctrl Pts',(-2.66450788394824,-0.951602474453648,
11.1686250464566));
#38762=CARTESIAN_POINT('Ctrl Pts',(-2.69817002472794,-0.859613847080416,
11.1651505728457));
#38763=CARTESIAN_POINT('Ctrl Pts',(-2.73183382450822,-0.767620686151626,
11.1616759279993));
#38764=CARTESIAN_POINT('Ctrl Pts',(-2.76085223666098,-0.67413102162785,
11.1582115915653));
#38765=CARTESIAN_POINT('Ctrl Pts',(-2.78504109696179,-0.579512179774996,
11.1547528451809));
#38766=CARTESIAN_POINT('Ctrl Pts',(-2.80867562760501,-0.487061692675289,
11.1513733619645));
#38767=CARTESIAN_POINT('Ctrl Pts',(-2.8276996967141,-0.393532337548253,
11.1479992155222));
#38768=CARTESIAN_POINT('Ctrl Pts',(-2.84189514122644,-0.299251761426908,
11.1446260045022));
#38769=CARTESIAN_POINT('Ctrl Pts',(-2.85324010443846,-0.223902964369238,
11.1419301428196));
#38770=CARTESIAN_POINT('Ctrl Pts',(-2.86150015598816,-0.148073915036915,
11.1392348786069));
#38771=CARTESIAN_POINT('Ctrl Pts',(-2.86653995619031,-0.0719300717664526,
11.1365379651471));
#38772=CARTESIAN_POINT('Ctrl Pts',(-2.86814414143213,-0.0476932320643782,
11.1356795285827));
#38773=CARTESIAN_POINT('Ctrl Pts',(-2.86941988081495,-0.0234547494955555,
11.1348219958471));
#38774=CARTESIAN_POINT('Ctrl Pts',(-2.87036479087719,0.000779773978368722,
11.1339652973708));
#38775=CARTESIAN_POINT('',(0.261199069988913,2.92594434598213,11.058));
#38776=CARTESIAN_POINT('Ctrl Pts',(0.261124777554784,2.92529416030266,11.058));
#38777=CARTESIAN_POINT('Ctrl Pts',(0.163252076286772,2.9214051496811,11.0703793245688));
#38778=CARTESIAN_POINT('Ctrl Pts',(0.0658388360676064,2.91286361031638,
11.0828028087884));
#38779=CARTESIAN_POINT('Ctrl Pts',(-0.0307369711720644,2.89968653111402,
11.0952900032599));
#38780=CARTESIAN_POINT('Ctrl Pts',(-0.12623809978967,2.88665608413482,11.1076382424244));
#38781=CARTESIAN_POINT('Ctrl Pts',(-0.220921197195477,2.86909236615812,
11.1200487818169));
#38782=CARTESIAN_POINT('Ctrl Pts',(-0.31439997383375,2.84696555496448,11.1325405266072));
#38783=CARTESIAN_POINT('Ctrl Pts',(-0.389995520831668,2.82907177783499,
11.1426425017756));
#38784=CARTESIAN_POINT('Ctrl Pts',(-0.464803253647579,2.80819289824412,
11.152797583885));
#38785=CARTESIAN_POINT('Ctrl Pts',(-0.538603048202427,2.78429272567688,
11.1630157713274));
#38786=CARTESIAN_POINT('Ctrl Pts',(-0.593952894118562,2.76636759625145,
11.1706794119091));
#38787=CARTESIAN_POINT('Ctrl Pts',(-0.648735503576454,2.7467426089957,11.1783785492407));
#38788=CARTESIAN_POINT('Ctrl Pts',(-0.702851172581185,2.72539620337798,
11.1861174013937));
#38789=CARTESIAN_POINT('Ctrl Pts',(-0.71873840261759,2.71912934457837,11.1883893667345));
#38790=CARTESIAN_POINT('Ctrl Pts',(-0.734568107078247,2.71271408483162,
11.190664755044));
#38791=CARTESIAN_POINT('Ctrl Pts',(-0.750337652372167,2.70614979460715,
11.1929436730527));
#38792=CARTESIAN_POINT('Ctrl Pts',(-0.763539656096334,2.70065427889159,
11.1948515456945));
#38793=CARTESIAN_POINT('Ctrl Pts',(-0.776691326847496,2.69505769580723,
11.1967607130315));
#38794=CARTESIAN_POINT('Ctrl Pts',(-0.789788993683481,2.68936106997679,
11.1986708957826));
#38795=CARTESIAN_POINT('Ctrl Pts',(-0.87317349082548,2.65309428397392,11.2108318119326));
#38796=CARTESIAN_POINT('Ctrl Pts',(-0.954403883416443,2.61276259333994,
11.2230385405707));
#38797=CARTESIAN_POINT('Ctrl Pts',(-1.03314628688233,2.56834468618871,11.2353100289649));
#38798=CARTESIAN_POINT('Ctrl Pts',(-1.07823214235908,2.54291214597843,11.2423363645588));
#38799=CARTESIAN_POINT('Ctrl Pts',(-1.12250179725942,2.51613922516579,11.2493839310575));
#38800=CARTESIAN_POINT('Ctrl Pts',(-1.16588734321926,2.48801620495338,11.2564562851141));
#38801=CARTESIAN_POINT('Ctrl Pts',(-1.2435976078222,2.43764349916415,11.2691239718505));
#38802=CARTESIAN_POINT('Ctrl Pts',(-1.31847408700313,2.38294042952196,11.2818711829841));
#38803=CARTESIAN_POINT('Ctrl Pts',(-1.39030087935118,2.32423346489716,11.2947183566611));
#38804=CARTESIAN_POINT('Ctrl Pts',(-1.46342993694969,2.26446210581046,11.3077984577361));
#38805=CARTESIAN_POINT('Ctrl Pts',(-1.53339828473794,2.20053932645019,11.3209821789827));
#38806=CARTESIAN_POINT('Ctrl Pts',(-1.59992558939365,2.1327921427514,11.3342910904939));
#38807=CARTESIAN_POINT('Ctrl Pts',(-1.61340208445737,2.11906853570881,11.3369870884937));
#38808=CARTESIAN_POINT('Ctrl Pts',(-1.62674073455187,2.10518403555254,11.3396889690338));
#38809=CARTESIAN_POINT('Ctrl Pts',(-1.63991787601809,2.09116421105248,11.3423925384684));
#38810=CARTESIAN_POINT('Ctrl Pts',(-1.70139884650346,2.02575150993609,11.3550066606613));
#38811=CARTESIAN_POINT('Ctrl Pts',(-1.75944768512028,1.95731714657644,11.3676731670409));
#38812=CARTESIAN_POINT('Ctrl Pts',(-1.8138993651727,1.88618389956551,11.3804137020214));
#38813=CARTESIAN_POINT('Ctrl Pts',(-1.86815753562372,1.81530344486993,11.393108959871));
#38814=CARTESIAN_POINT('Ctrl Pts',(-1.91884436205444,1.74174225535381,11.4058777210929));
#38815=CARTESIAN_POINT('Ctrl Pts',(-1.96574838356875,1.66580180077525,11.4187414001618));
#38816=CARTESIAN_POINT('Ctrl Pts',(-2.01186212788083,1.59114085290088,11.4313883414761));
#38817=CARTESIAN_POINT('Ctrl Pts',(-2.05431959945996,1.51417923664983,11.4441270290762));
#38818=CARTESIAN_POINT('Ctrl Pts',(-2.09287020326133,1.43520021222363,11.4569778131465));
#38819=CARTESIAN_POINT('Ctrl Pts',(-2.11361694660402,1.39269614256837,11.4638937079073));
#38820=CARTESIAN_POINT('Ctrl Pts',(-2.13323129045024,1.34960780406157,11.4708420687169));
#38821=CARTESIAN_POINT('Ctrl Pts',(-2.15166787184208,1.30598030868302,11.4778260675126));
#38822=CARTESIAN_POINT('Ctrl Pts',(-2.15713184571921,1.29305060712901,11.4798958865407));
#38823=CARTESIAN_POINT('Ctrl Pts',(-2.16249308944786,1.28007170317631,11.4819691313049));
#38824=CARTESIAN_POINT('Ctrl Pts',(-2.16774797314523,1.26705068510794,11.4840449452013));
#38825=CARTESIAN_POINT('Ctrl Pts',(-2.19963752356477,1.18803192158837,11.4966421358759));
#38826=CARTESIAN_POINT('Ctrl Pts',(-2.22751419897903,1.10771397257159,11.5092939385505));
#38827=CARTESIAN_POINT('Ctrl Pts',(-2.25120331746379,1.02636717479289,11.5220225137828));
#38828=CARTESIAN_POINT('Ctrl Pts',(-2.27454503464211,0.946213329121761,
11.5345644242532));
#38829=CARTESIAN_POINT('Ctrl Pts',(-2.29382118362004,0.865059764231561,
11.5471808720505));
#38830=CARTESIAN_POINT('Ctrl Pts',(-2.30881496364231,0.783166675687281,
11.5598930570057));
#38831=CARTESIAN_POINT('Ctrl Pts',(-2.3233692591387,0.703673965509062,11.572232633548));
#38832=CARTESIAN_POINT('Ctrl Pts',(-2.33388845327117,0.623483808186223,
11.5846624171728));
#38833=CARTESIAN_POINT('Ctrl Pts',(-2.34012749274977,0.542846284442329,
11.5972017976454));
#38834=CARTESIAN_POINT('Ctrl Pts',(-2.34523853245788,0.476787785015864,
11.6074740954455));
#38835=CARTESIAN_POINT('Ctrl Pts',(-2.34747636127652,0.410429125649976,
11.6178199429796));
#38836=CARTESIAN_POINT('Ctrl Pts',(-2.34668236863853,0.343918483395475,
11.62825));
#38837=CARTESIAN_POINT('',(-2.14415473270599,2.01243073062329,11.058));
#38838=CARTESIAN_POINT('Origin',(0.,0.,11.058));
#38839=CARTESIAN_POINT('Ctrl Pts',(-2.87036479087719,0.000779773978368722,
11.1339652973708));
#38840=CARTESIAN_POINT('Ctrl Pts',(-2.87200285191233,0.0427918449624727,
11.1324801566689));
#38841=CARTESIAN_POINT('Ctrl Pts',(-2.87264678506693,0.0847919926152422,
11.1309975229776));
#38842=CARTESIAN_POINT('Ctrl Pts',(-2.87228289058568,0.126751532711213,
11.1295170338848));
#38843=CARTESIAN_POINT('Ctrl Pts',(-2.87145802595519,0.221864106052536,
11.1261611075067));
#38844=CARTESIAN_POINT('Ctrl Pts',(-2.86545855469524,0.316767622116373,
11.1228162005919));
#38845=CARTESIAN_POINT('Ctrl Pts',(-2.85455763680452,0.411156736693552,
11.1194780920563));
#38846=CARTESIAN_POINT('Ctrl Pts',(-2.84342076253498,0.507588955704657,
11.1160677283208));
#38847=CARTESIAN_POINT('Ctrl Pts',(-2.82716775830471,0.603485022278454,
11.1126644604589));
#38848=CARTESIAN_POINT('Ctrl Pts',(-2.80603441756026,0.698520670355508,
11.1092637873076));
#38849=CARTESIAN_POINT('Ctrl Pts',(-2.79266006313991,0.75866451866233,11.1071116520374));
#38850=CARTESIAN_POINT('Ctrl Pts',(-2.77733000149192,0.818463754777881,
11.1049605559651));
#38851=CARTESIAN_POINT('Ctrl Pts',(-2.76009348614301,0.877834296726592,
11.1028093582138));
#38852=CARTESIAN_POINT('Ctrl Pts',(-2.74919109087412,0.915387195473845,
11.1014486882808));
#38853=CARTESIAN_POINT('Ctrl Pts',(-2.73752580613221,0.952768545576029,
11.1000879776682));
#38854=CARTESIAN_POINT('Ctrl Pts',(-2.72510854264357,0.989956497598032,
11.0987269376699));
#38855=CARTESIAN_POINT('Ctrl Pts',(-2.72027063675402,1.00444534308902,11.0981966611375));
#38856=CARTESIAN_POINT('Ctrl Pts',(-2.71531799003855,1.0189064745382,11.0976662739811));
#38857=CARTESIAN_POINT('Ctrl Pts',(-2.71025302608607,1.03333338889234,11.0971359498549));
#38858=CARTESIAN_POINT('Ctrl Pts',(-2.67741979989202,1.12685471435798,11.0936981658637));
#38859=CARTESIAN_POINT('Ctrl Pts',(-2.63998428261572,1.2186200392303,11.0902747408666));
#38860=CARTESIAN_POINT('Ctrl Pts',(-2.59822193704792,1.30830487286322,11.0868612068006));
#38861=CARTESIAN_POINT('Ctrl Pts',(-2.55598691495593,1.39900478155616,11.0834090375144));
#38862=CARTESIAN_POINT('Ctrl Pts',(-2.50932621498891,1.48757769234242,11.0799669843223));
#38863=CARTESIAN_POINT('Ctrl Pts',(-2.45847158858181,1.57367848927911,11.0765304257261));
#38864=CARTESIAN_POINT('Ctrl Pts',(-2.40788866695146,1.65931926911486,11.0731122278858));
#38865=CARTESIAN_POINT('Ctrl Pts',(-2.35315604081231,1.74251510638125,11.0696994660854));
#38866=CARTESIAN_POINT('Ctrl Pts',(-2.29445585803367,1.82290449738493,11.0662875925062));
#38867=CARTESIAN_POINT('Ctrl Pts',(-2.24693123162509,1.88798906090443,11.0635252839489));
#38868=CARTESIAN_POINT('Ctrl Pts',(-2.19680500482205,1.95123384018432,11.0607635576017));
#38869=CARTESIAN_POINT('Ctrl Pts',(-2.14415473270599,2.01243073062329,11.058));
#38870=CARTESIAN_POINT('',(-2.,-2.4492935982947E-16,12.));
#38871=CARTESIAN_POINT('',(-2.5,-3.06161699786838E-16,11.5));
#38872=CARTESIAN_POINT('Origin',(0.,0.,12.));
#38873=CARTESIAN_POINT('Ctrl Pts',(1.70810875200395,-2.39535560853238,-0.329233991005387));
#38874=CARTESIAN_POINT('Ctrl Pts',(2.49644455514999,-1.833199709811,-0.276854486500882));
#38875=CARTESIAN_POINT('Ctrl Pts',(3.46233357982621,0.120022568706166,-0.172095477491873));
#38876=CARTESIAN_POINT('Ctrl Pts',(1.80423238277522,2.96114098648209,-0.0149569639783592));
#38877=CARTESIAN_POINT('Ctrl Pts',(-1.47579564172449,3.13432118289611,0.142181549535154));
#38878=CARTESIAN_POINT('Ctrl Pts',(-3.42956675747562,0.496557026061836,
0.299320063048668));
#38879=CARTESIAN_POINT('Ctrl Pts',(-2.30343226514234,-2.58935922774548,
0.456458576562181));
#38880=CARTESIAN_POINT('Ctrl Pts',(0.891761112414455,-3.34848577424617,
0.613597090075694));
#38881=CARTESIAN_POINT('Ctrl Pts',(3.2859015926111,-1.1007252807108,0.770735603589207));
#38882=CARTESIAN_POINT('Ctrl Pts',(2.7288317609948,2.13597203247546,0.927874117102722));
#38883=CARTESIAN_POINT('Ctrl Pts',(-0.27919655644097,3.45406211813255,1.08501263061624));
#38884=CARTESIAN_POINT('Ctrl Pts',(-3.03644606033952,1.66993460430069,1.24215114412975));
#38885=CARTESIAN_POINT('Ctrl Pts',(-3.06648780987738,-1.61410638094873,
1.39928965764326));
#38886=CARTESIAN_POINT('Ctrl Pts',(-0.342327145073366,-3.44839767949667,
1.55642817115678));
#38887=CARTESIAN_POINT('Ctrl Pts',(2.68929601578421,-2.18548654390084,1.71356668467029));
#38888=CARTESIAN_POINT('Ctrl Pts',(3.30550092715682,1.04034856780235,1.8707051981838));
#38889=CARTESIAN_POINT('Ctrl Pts',(0.952834920914103,3.33178039838987,2.02784371169731));
#38890=CARTESIAN_POINT('Ctrl Pts',(-2.25562944112346,2.630740466173,2.18498222521083));
#38891=CARTESIAN_POINT('Ctrl Pts',(-3.43817673987435,-0.433127500149091,
2.34212073872434));
#38892=CARTESIAN_POINT('Ctrl Pts',(-1.53268946892128,-3.10797698807607,
2.49925925223786));
#38893=CARTESIAN_POINT('Ctrl Pts',(1.7493988709872,-2.99136460950407,2.65639776575137));
#38894=CARTESIAN_POINT('Ctrl Pts',(3.46024629894863,-0.188026617557356,
2.81353627926488));
#38895=CARTESIAN_POINT('Ctrl Pts',(2.06323722577413,2.78418938435949,2.97067479277839));
#38896=CARTESIAN_POINT('Ctrl Pts',(-1.18688998506621,3.25575653825361,3.12781330629191));
#38897=CARTESIAN_POINT('Ctrl Pts',(-3.3709995165217,0.803131807227777,3.28495181980542));
#38898=CARTESIAN_POINT('Ctrl Pts',(-2.52741049074122,-2.37083416635282,
3.44209033331894));
#38899=CARTESIAN_POINT('Ctrl Pts',(0.586198762341201,-3.41541058398195,
3.59922884683245));
#38900=CARTESIAN_POINT('Ctrl Pts',(3.17330745213002,-1.3924001776803,3.75636736034597));
#38901=CARTESIAN_POINT('Ctrl Pts',(2.91027678633445,1.88120904397026,3.91350587385948));
#38902=CARTESIAN_POINT('Ctrl Pts',(0.0333505152943699,3.46519064195013,
4.07064438737299));
#38903=CARTESIAN_POINT('Ctrl Pts',(-2.87352987075533,1.93687493734171,4.22778290088651));
#38904=CARTESIAN_POINT('Ctrl Pts',(-3.19951927885268,-1.33106529716661,
4.38492141440001));
#38905=CARTESIAN_POINT('Ctrl Pts',(-0.651826904677972,-3.40349528097662,
4.54205992791353));
#38906=CARTESIAN_POINT('Ctrl Pts',(2.48131063733581,-2.41904029776201,4.69919844142705));
#38907=CARTESIAN_POINT('Ctrl Pts',(3.38583301773356,0.738101088738959,4.85633695494055));
#38908=CARTESIAN_POINT('Ctrl Pts',(1.24933397805696,3.23230924456058,5.01347546845408));
#38909=CARTESIAN_POINT('Ctrl Pts',(-2.00926747133911,2.82338496663079,5.17061398196758));
#38910=CARTESIAN_POINT('Ctrl Pts',(-3.46322427730269,-0.12139211787978,
5.3277524954811));
#38911=CARTESIAN_POINT('Ctrl Pts',(-1.80664989208085,-2.95713959911133,
5.48489100899462));
#38912=CARTESIAN_POINT('Ctrl Pts',(1.47258603363221,-3.13690114838409,5.64202952250812));
#38913=CARTESIAN_POINT('Ctrl Pts',(3.4292033754596,-0.499222045701823,5.79916803602164));
#38914=CARTESIAN_POINT('Ctrl Pts',(2.30584575575073,2.58683857089803,5.95630654953515));
#38915=CARTESIAN_POINT('Ctrl Pts',(-0.888531402702859,3.34950300605675,
6.11344506304867));
#38916=CARTESIAN_POINT('Ctrl Pts',(-3.28486476693535,1.10377620199891,6.27058357656218));
#38917=CARTESIAN_POINT('Ctrl Pts',(-2.73086240406331,-2.13331876928079,
6.4277220900757));
#38918=CARTESIAN_POINT('Ctrl Pts',(0.275892655912234,-3.45435112336383,
6.5848606035892));
#38919=CARTESIAN_POINT('Ctrl Pts',(3.03485183459055,-1.67282180255638,6.74199911710273));
#38920=CARTESIAN_POINT('Ctrl Pts',(3.06802702248421,1.6111699572782,6.89913763061623));
#38921=CARTESIAN_POINT('Ctrl Pts',(0.345621576330127,3.44807252913389,7.05627614412975));
#38922=CARTESIAN_POINT('Ctrl Pts',(-2.68720751132516,2.18805261171336,7.21341465764325));
#38923=CARTESIAN_POINT('Ctrl Pts',(-3.30649300260574,-1.03718969811004,
7.37055317115678));
#38924=CARTESIAN_POINT('Ctrl Pts',(-0.956017138014702,-3.33086920560938,
7.52769168467029));
#38925=CARTESIAN_POINT('Ctrl Pts',(2.25311553735071,-2.63289362024357,7.68483019818381));
#38926=CARTESIAN_POINT('Ctrl Pts',(3.43858888024395,0.429842977951538,7.84196871169731));
#38927=CARTESIAN_POINT('Ctrl Pts',(1.53565755714059,3.10651158777771,7.99910722521083));
#38928=CARTESIAN_POINT('Ctrl Pts',(-1.74654067132524,2.99303427005181,8.15624573872433));
#38929=CARTESIAN_POINT('Ctrl Pts',(-3.46006514069016,0.191331803382343,
8.31338425223787));
#38930=CARTESIAN_POINT('Ctrl Pts',(-2.06589572612039,-2.78221724805058,
8.47052276575136));
#38931=CARTESIAN_POINT('Ctrl Pts',(1.183779392948,-3.25688886436581,8.62766127926489));
#38932=CARTESIAN_POINT('Ctrl Pts',(3.37023102179748,-0.806351310370959,
8.7847997927784));
#38933=CARTESIAN_POINT('Ctrl Pts',(2.52967359714463,2.36841856552378,8.94193830629191));
#38934=CARTESIAN_POINT('Ctrl Pts',(-0.582935293544439,3.41596954985013,
9.09907681980542));
#38935=CARTESIAN_POINT('Ctrl Pts',(-3.17197740603666,1.3954296219005,9.25621533331893));
#38936=CARTESIAN_POINT('Ctrl Pts',(-2.91206965945989,-1.87842613074489,
9.41335384683245));
#38937=CARTESIAN_POINT('Ctrl Pts',(-0.0366657672894424,-3.46516125435096,
9.57049236034596));
#38938=CARTESIAN_POINT('Ctrl Pts',(2.8716885037831,-1.93961114588268,9.72763087385947));
#38939=CARTESIAN_POINT('Ctrl Pts',(3.20077001198978,1.32799366090119,9.88476938737299));
#38940=CARTESIAN_POINT('Ctrl Pts',(0.655114493273841,3.40289939669598,10.0419079008865));
#38941=CARTESIAN_POINT('Ctrl Pts',(-2.47906919875826,2.42135526672317,10.1990464144));
#38942=CARTESIAN_POINT('Ctrl Pts',(-3.3864019310671,-0.734763106864168,
10.3561849279135));
#38943=CARTESIAN_POINT('Ctrl Pts',(-1.25267830620767,-3.23131219035953,
10.513323441427));
#38944=CARTESIAN_POINT('Ctrl Pts',(2.00706204302524,-2.82492459714601,10.6704619549406));
#38945=CARTESIAN_POINT('Ctrl Pts',(3.46239353138226,0.117358798249391,10.8276004684541));
#38946=CARTESIAN_POINT('Ctrl Pts',(1.81131357477516,2.9568147670617,10.9847389819676));
#38947=CARTESIAN_POINT('Ctrl Pts',(-1.47339811761136,3.13548357068097,11.1418774954811));
#38948=CARTESIAN_POINT('Ctrl Pts',(-2.77050414434575,1.38461669033425,11.2466365044901));
#38949=CARTESIAN_POINT('Ctrl Pts',(-2.91090525077877,0.426608275808828,
11.2990160089946));
#38950=CARTESIAN_POINT('Ctrl Pts',(1.59774743137964,-2.24059110187414,-0.219489327336925));
#38951=CARTESIAN_POINT('Ctrl Pts',(2.33514866714022,-1.71475623207252,-0.167109822832421));
#38952=CARTESIAN_POINT('Ctrl Pts',(3.23863136773739,0.11226788144075,-0.0623508138234118));
#38953=CARTESIAN_POINT('Ctrl Pts',(1.6876604910601,2.76982094937113,0.0947876996901019));
#38954=CARTESIAN_POINT('Ctrl Pts',(-1.38044412748324,2.93181193130462,0.251926213203615));
#38955=CARTESIAN_POINT('Ctrl Pts',(-3.2079816177237,0.464474356210045,0.409064726717129));
#38956=CARTESIAN_POINT('Ctrl Pts',(-2.15460694798876,-2.42206010021071,
0.566203240230643));
#38957=CARTESIAN_POINT('Ctrl Pts',(0.834144210720117,-3.13213929648004,
0.723341753744155));
#38958=CARTESIAN_POINT('Ctrl Pts',(3.07359869399491,-1.02960715343621,0.880480267257669));
#38959=CARTESIAN_POINT('Ctrl Pts',(2.55252127926951,1.99796636155783,1.03761878077118));
#38960=CARTESIAN_POINT('Ctrl Pts',(-0.261157599233816,3.2308943271893,1.19475729428469));
#38961=CARTESIAN_POINT('Ctrl Pts',(-2.84026054414775,1.56203972461538,1.35189580779821));
#38962=CARTESIAN_POINT('Ctrl Pts',(-2.86836128896387,-1.50981857631063,
1.50903432131172));
#38963=CARTESIAN_POINT('Ctrl Pts',(-0.320209305227662,-3.22559586930712,
1.66617283482524));
#38964=CARTESIAN_POINT('Ctrl Pts',(2.51553994814305,-2.04428172839443,1.82331134833875));
#38965=CARTESIAN_POINT('Ctrl Pts',(3.09193171078347,0.973131394588079,1.98044986185226));
#38966=CARTESIAN_POINT('Ctrl Pts',(0.891272025644291,3.1165132590083,2.13758837536578));
#38967=CARTESIAN_POINT('Ctrl Pts',(-2.10989267602029,2.4607676867899,2.29472688887929));
#38968=CARTESIAN_POINT('Ctrl Pts',(-3.21603530707201,-0.405143027346019,
2.4518654023928));
#38969=CARTESIAN_POINT('Ctrl Pts',(-1.43366203071003,-2.90716984129947,
2.60900391590632));
#38970=CARTESIAN_POINT('Ctrl Pts',(1.63636978576396,-2.79809181678146,2.76614242941983));
#38971=CARTESIAN_POINT('Ctrl Pts',(3.23667894658341,-0.175878172207005,
2.92328094293335));
#38972=CARTESIAN_POINT('Ctrl Pts',(1.92993096835312,2.60430223316632,3.08041945644686));
#38973=CARTESIAN_POINT('Ctrl Pts',(-1.11020473535129,3.04540131890859,3.23755796996037));
#38974=CARTESIAN_POINT('Ctrl Pts',(-3.15319842040834,0.751241266431068,
3.39469648347389));
#38975=CARTESIAN_POINT('Ctrl Pts',(-2.36411388612472,-2.21765399601942,
3.5518349969874));
#38976=CARTESIAN_POINT('Ctrl Pts',(0.548324318173406,-3.19474007803184,
3.70897351050091));
#38977=CARTESIAN_POINT('Ctrl Pts',(2.96827928823051,-1.30243686459143,3.86611202401443));
#38978=CARTESIAN_POINT('Ctrl Pts',(2.72224309752783,1.75966367151117,4.02325053752794));
#38979=CARTESIAN_POINT('Ctrl Pts',(0.0311957304148393,3.24130383438475,
4.18038905104146));
#38980=CARTESIAN_POINT('Ctrl Pts',(-2.68787040907414,1.81173297801481,4.33752756455496));
#38981=CARTESIAN_POINT('Ctrl Pts',(-2.99279756247315,-1.24506484557935,
4.49466607806848));
#38982=CARTESIAN_POINT('Ctrl Pts',(-0.609712210321215,-3.18359462564273,
4.65180459158199));
#38983=CARTESIAN_POINT('Ctrl Pts',(2.32099255542547,-2.26274551758992,4.80894310509551));
#38984=CARTESIAN_POINT('Ctrl Pts',(3.16707352551029,0.69041219843154,4.96608161860902));
#38985=CARTESIAN_POINT('Ctrl Pts',(1.16861420681437,3.02346896054623,5.12322013212254));
#38986=CARTESIAN_POINT('Ctrl Pts',(-1.87944821283798,2.64096537936348,5.28035864563605));
#38987=CARTESIAN_POINT('Ctrl Pts',(-3.23946451703395,-0.113548943710187,
5.43749715914956));
#38988=CARTESIAN_POINT('Ctrl Pts',(-1.68992180450333,-2.76607809260859,
5.59463567266307));
#38989=CARTESIAN_POINT('Ctrl Pts',(1.37744189294803,-2.93422520459686,5.75177418617659));
#38990=CARTESIAN_POINT('Ctrl Pts',(3.20764171390784,-0.466967188284919,
5.9089126996901));
#38991=CARTESIAN_POINT('Ctrl Pts',(2.15686450238375,2.41970230361335,6.06605121320362));
#38992=CARTESIAN_POINT('Ctrl Pts',(-0.831123173336083,3.13309080469669,
6.22318972671712));
#38993=CARTESIAN_POINT('Ctrl Pts',(-3.07262885787747,1.03246095396017,6.38032824023064));
#38994=CARTESIAN_POINT('Ctrl Pts',(-2.55442072199701,-1.99548452634149,
6.53746675374416));
#38995=CARTESIAN_POINT('Ctrl Pts',(0.258067164519323,-3.23116465972251,
6.69460526725767));
#38996=CARTESIAN_POINT('Ctrl Pts',(2.83876932171097,-1.56474038029172,6.85174378077119));
#38997=CARTESIAN_POINT('Ctrl Pts',(2.86980105267096,1.50707187568543,7.00888229428469));
#38998=CARTESIAN_POINT('Ctrl Pts',(0.323290882482136,3.22529172698812,7.1660208077982));
#38999=CARTESIAN_POINT('Ctrl Pts',(-2.51358638246349,2.04668200194341,7.32315932131173));
#39000=CARTESIAN_POINT('Ctrl Pts',(-3.09285968799709,-0.970176620232505,
7.48029783482524));
#39001=CARTESIAN_POINT('Ctrl Pts',(-0.89424863892644,-3.11566093861428,
7.63743634833875));
#39002=CARTESIAN_POINT('Ctrl Pts',(2.10754119617984,-2.46278172505391,7.79457486185227));
#39003=CARTESIAN_POINT('Ctrl Pts',(3.21642081895241,0.402070718924034,7.95171337536577));
#39004=CARTESIAN_POINT('Ctrl Pts',(1.43643835002984,2.90579912086969,8.1088518888793));
#39005=CARTESIAN_POINT('Ctrl Pts',(-1.63369625507517,2.79965360015637,8.2659904023928));
#39006=CARTESIAN_POINT('Ctrl Pts',(-3.23650949300394,0.178969809174445,
8.42312891590632));
#39007=CARTESIAN_POINT('Ctrl Pts',(-1.93241770234741,-2.6024575170625,8.58026742941983));
#39008=CARTESIAN_POINT('Ctrl Pts',(1.10729511934404,-3.04646048515613,8.73740594293334));
#39009=CARTESIAN_POINT('Ctrl Pts',(3.15247957831459,-0.75425275669555,8.89454445644686));
#39010=CARTESIAN_POINT('Ctrl Pts',(2.36623077267467,2.21539446774564,9.05168296996036));
#39011=CARTESIAN_POINT('Ctrl Pts',(-0.54527170288688,3.19526292897974,9.20882148347389));
#39012=CARTESIAN_POINT('Ctrl Pts',(-2.96703517673773,1.30527057568604,9.36595999698739));
#39013=CARTESIAN_POINT('Ctrl Pts',(-2.72392013268591,-1.75706056298405,
9.52309851050092));
#39014=CARTESIAN_POINT('Ctrl Pts',(-0.0342967831746755,-3.24127634552548,
9.68023702401442));
#39015=CARTESIAN_POINT('Ctrl Pts',(2.68614801326846,-1.81429239945851,9.83737553752795));
#39016=CARTESIAN_POINT('Ctrl Pts',(2.99396748543899,1.24219166847781,9.99451405104144));
#39017=CARTESIAN_POINT('Ctrl Pts',(0.612787387020777,3.18303724158995,10.151652564555));
#39018=CARTESIAN_POINT('Ctrl Pts',(-2.31889593673789,2.2649109158452,10.3087910780685));
#39019=CARTESIAN_POINT('Ctrl Pts',(-3.16760568121541,-0.687289884375024,
10.465929591582));
#39020=CARTESIAN_POINT('Ctrl Pts',(-1.17174245711238,-3.02253632625886,
10.6230681050955));
#39021=CARTESIAN_POINT('Ctrl Pts',(1.8773852777822,-2.64240553397781,10.780206618609));
#39022=CARTESIAN_POINT('Ctrl Pts',(3.23868744580887,0.109776217839061,10.9373451321225));
#39023=CARTESIAN_POINT('Ctrl Pts',(1.69428416552798,2.76577424803644,11.0944836456361));
#39024=CARTESIAN_POINT('Ctrl Pts',(-1.37820150798437,2.93289921693286,11.2516221591496));
#39025=CARTESIAN_POINT('Ctrl Pts',(-2.59150119982806,1.29515627025004,11.3563811681586));
#39026=CARTESIAN_POINT('Ctrl Pts',(-2.72283095673203,0.399045011671044,
11.4087606726631));
#39027=CARTESIAN_POINT('Ctrl Pts',(1.48738611075532,-2.08582659521589,-0.109744663668464));
#39028=CARTESIAN_POINT('Ctrl Pts',(2.17385277913045,-1.59631275433404,-0.0573651591639592));
#39029=CARTESIAN_POINT('Ctrl Pts',(3.01492915564857,0.104513194175331,0.0473938498450494));
#39030=CARTESIAN_POINT('Ctrl Pts',(1.57108859934498,2.57850091226017,0.204532363358563));
#39031=CARTESIAN_POINT('Ctrl Pts',(-1.28509261324199,2.72930267971312,0.361670876872076));
#39032=CARTESIAN_POINT('Ctrl Pts',(-2.98639647797178,0.432391686358259,
0.51880939038559));
#39033=CARTESIAN_POINT('Ctrl Pts',(-2.00578163083517,-2.25476097267596,
0.675947903899103));
#39034=CARTESIAN_POINT('Ctrl Pts',(0.776527309025778,-2.9157928187139,0.833086417412617));
#39035=CARTESIAN_POINT('Ctrl Pts',(2.86129579537873,-0.958489026161636,
0.99022493092613));
#39036=CARTESIAN_POINT('Ctrl Pts',(2.37621079754423,1.85996069064019,1.14736344443964));
#39037=CARTESIAN_POINT('Ctrl Pts',(-0.243118642026661,3.00772653624605,
1.30450195795316));
#39038=CARTESIAN_POINT('Ctrl Pts',(-2.64407502795598,1.45414484493007,1.46164047146667));
#39039=CARTESIAN_POINT('Ctrl Pts',(-2.67023476805036,-1.40553077167252,
1.61877898498018));
#39040=CARTESIAN_POINT('Ctrl Pts',(-0.298091465381954,-3.00279405911757,
1.7759174984937));
#39041=CARTESIAN_POINT('Ctrl Pts',(2.34178388050189,-1.90307691288803,1.93305601200721));
#39042=CARTESIAN_POINT('Ctrl Pts',(2.87836249441012,0.905914221373807,2.09019452552073));
#39043=CARTESIAN_POINT('Ctrl Pts',(0.829709130374474,2.90124611962672,2.24733303903424));
#39044=CARTESIAN_POINT('Ctrl Pts',(-1.96415591091712,2.2907949074068,2.40447155254775));
#39045=CARTESIAN_POINT('Ctrl Pts',(-2.99389387426969,-0.37715855454295,
2.56161006606126));
#39046=CARTESIAN_POINT('Ctrl Pts',(-1.33463459249878,-2.70636269452286,
2.71874857957478));
#39047=CARTESIAN_POINT('Ctrl Pts',(1.52334070054072,-2.60481902405885,2.87588709308829));
#39048=CARTESIAN_POINT('Ctrl Pts',(3.01311159421818,-0.163729726856653,
3.03302560660181));
#39049=CARTESIAN_POINT('Ctrl Pts',(1.79662471093212,2.42441508197314,3.19016412011532));
#39050=CARTESIAN_POINT('Ctrl Pts',(-1.03351948563637,2.83504609956357,3.34730263362884));
#39051=CARTESIAN_POINT('Ctrl Pts',(-2.93539732429499,0.699350725634357,
3.50444114714234));
#39052=CARTESIAN_POINT('Ctrl Pts',(-2.20081728150821,-2.06447382568602,
3.66157966065586));
#39053=CARTESIAN_POINT('Ctrl Pts',(0.510449874005612,-2.97406957208172,
3.81871817416937));
#39054=CARTESIAN_POINT('Ctrl Pts',(2.763251124331,-1.21247355150257,3.97585668768289));
#39055=CARTESIAN_POINT('Ctrl Pts',(2.5342094087212,1.63811829905208,4.1329952011964));
#39056=CARTESIAN_POINT('Ctrl Pts',(0.029040945535309,3.01741702681936,4.29013371470992));
#39057=CARTESIAN_POINT('Ctrl Pts',(-2.50221094739296,1.68659101868791,4.44727222822342));
#39058=CARTESIAN_POINT('Ctrl Pts',(-2.78607584609361,-1.1590643939921,4.60441074173694));
#39059=CARTESIAN_POINT('Ctrl Pts',(-0.56759751596446,-2.96369397030884,
4.76154925525046));
#39060=CARTESIAN_POINT('Ctrl Pts',(2.16067447351513,-2.10645073741783,4.91868776876396));
#39061=CARTESIAN_POINT('Ctrl Pts',(2.94831403328702,0.642723308124124,5.07582628227749));
#39062=CARTESIAN_POINT('Ctrl Pts',(1.08789443557179,2.81462867653188,5.23296479579099));
#39063=CARTESIAN_POINT('Ctrl Pts',(-1.74962895433684,2.45854579209617,5.39010330930451));
#39064=CARTESIAN_POINT('Ctrl Pts',(-3.01570475676522,-0.105705769540595,
5.54724182281802));
#39065=CARTESIAN_POINT('Ctrl Pts',(-1.57319371692581,-2.57501658610585,
5.70438033633154));
#39066=CARTESIAN_POINT('Ctrl Pts',(1.28229775226384,-2.73154926080963,5.86151884984505));
#39067=CARTESIAN_POINT('Ctrl Pts',(2.98608005235609,-0.434712330868017,
6.01865736335856));
#39068=CARTESIAN_POINT('Ctrl Pts',(2.00788324901678,2.25256603632868,6.17579587687208));
#39069=CARTESIAN_POINT('Ctrl Pts',(-0.773714943969305,2.91667860333663,
6.33293439038559));
#39070=CARTESIAN_POINT('Ctrl Pts',(-2.86039294881959,0.961145705921419,
6.4900729038991));
#39071=CARTESIAN_POINT('Ctrl Pts',(-2.37797903993071,-1.85765028340219,
6.64721141741262));
#39072=CARTESIAN_POINT('Ctrl Pts',(0.240241673126412,-3.0079781960812,6.80434993092612));
#39073=CARTESIAN_POINT('Ctrl Pts',(2.64268680883139,-1.45665895802706,6.96148844443965));
#39074=CARTESIAN_POINT('Ctrl Pts',(2.67157508285772,1.40297379409266,7.11862695795316));
#39075=CARTESIAN_POINT('Ctrl Pts',(0.300960188634146,3.00251092484234,7.27576547146667));
#39076=CARTESIAN_POINT('Ctrl Pts',(-2.33996525360183,1.90531139217345,7.43290398498018));
#39077=CARTESIAN_POINT('Ctrl Pts',(-2.87922637338843,-0.903163542354968,
7.5900424984937));
#39078=CARTESIAN_POINT('Ctrl Pts',(-0.832480139838179,-2.90045267161919,
7.74718101200721));
#39079=CARTESIAN_POINT('Ctrl Pts',(1.96196685500896,-2.29266982986425,7.90431952552073));
#39080=CARTESIAN_POINT('Ctrl Pts',(2.99425275766087,0.37429845989653,8.06145803903424));
#39081=CARTESIAN_POINT('Ctrl Pts',(1.33721914291908,2.70508665396167,8.21859655254775));
#39082=CARTESIAN_POINT('Ctrl Pts',(-1.5208518388251,2.60627293026094,8.37573506606126));
#39083=CARTESIAN_POINT('Ctrl Pts',(-3.01295384531772,0.166607814966547,
8.53287357957478));
#39084=CARTESIAN_POINT('Ctrl Pts',(-1.79893967857444,-2.42269778607442,
8.69001209308829));
#39085=CARTESIAN_POINT('Ctrl Pts',(1.03081084574009,-2.83603210594645,8.8471506066018));
#39086=CARTESIAN_POINT('Ctrl Pts',(2.9347281348317,-0.702154203020143,9.00428912011532));
#39087=CARTESIAN_POINT('Ctrl Pts',(2.20278794820472,2.06237036996751,9.16142763362883));
#39088=CARTESIAN_POINT('Ctrl Pts',(-0.507608112229325,2.97455630810935,
9.31856614714235));
#39089=CARTESIAN_POINT('Ctrl Pts',(-2.7620929474388,1.21511152947157,9.47570466065586));
#39090=CARTESIAN_POINT('Ctrl Pts',(-2.53577060591194,-1.63569499522321,
9.63284317416937));
#39091=CARTESIAN_POINT('Ctrl Pts',(-0.0319277990599106,-3.0173914367,9.78998168768289));
#39092=CARTESIAN_POINT('Ctrl Pts',(2.50060752275382,-1.68897365303435,9.94712020119639));
#39093=CARTESIAN_POINT('Ctrl Pts',(2.78716495888821,1.15638967605443,10.1042587147099));
#39094=CARTESIAN_POINT('Ctrl Pts',(0.570460280767717,2.96317508648391,10.2613972282234));
#39095=CARTESIAN_POINT('Ctrl Pts',(-2.15872267471752,2.10846656496723,10.4185357417369));
#39096=CARTESIAN_POINT('Ctrl Pts',(-2.94880943136371,-0.639816661885883,
10.5756742552505));
#39097=CARTESIAN_POINT('Ctrl Pts',(-1.09080660801709,-2.8137604621582,10.732812768764));
#39098=CARTESIAN_POINT('Ctrl Pts',(1.74770851253917,-2.4598864708096,10.8899512822775));
#39099=CARTESIAN_POINT('Ctrl Pts',(3.01498136023548,0.102193637428725,11.047089795791));
#39100=CARTESIAN_POINT('Ctrl Pts',(1.57725475628079,2.57473372901119,11.2042283093045));
#39101=CARTESIAN_POINT('Ctrl Pts',(-1.28300489835739,2.73031486318474,11.361366822818));
#39102=CARTESIAN_POINT('Ctrl Pts',(-2.41249825531037,1.20569585016584,11.466125831827));
#39103=CARTESIAN_POINT('Ctrl Pts',(-2.53475666268528,0.371481747533259,
11.5185053363315));
#39104=CARTESIAN_POINT('Ctrl Pts',(1.37702479013101,-1.93106208855765,-2.4980018054066E-15));
#39105=CARTESIAN_POINT('Ctrl Pts',(2.01255689112068,-1.47786927659557,0.052379504504502));
#39106=CARTESIAN_POINT('Ctrl Pts',(2.79122694355976,0.0967585069099138,
0.157138513513511));
#39107=CARTESIAN_POINT('Ctrl Pts',(1.45451670762985,2.3871808751492,0.314277027027025));
#39108=CARTESIAN_POINT('Ctrl Pts',(-1.18974109900074,2.52679342812162,0.471415540540538));
#39109=CARTESIAN_POINT('Ctrl Pts',(-2.76481133821986,0.40030901650647,0.628554054054051));
#39110=CARTESIAN_POINT('Ctrl Pts',(-1.85695631368159,-2.0874618451412,0.785692567567565));
#39111=CARTESIAN_POINT('Ctrl Pts',(0.718910407331439,-2.69944634094777,
0.942831081081078));
#39112=CARTESIAN_POINT('Ctrl Pts',(2.64899289676255,-0.887370898887054,
1.09996959459459));
#39113=CARTESIAN_POINT('Ctrl Pts',(2.19990031581894,1.72195501972256,1.25710810810811));
#39114=CARTESIAN_POINT('Ctrl Pts',(-0.225079684819506,2.78455874530281,
1.41424662162162));
#39115=CARTESIAN_POINT('Ctrl Pts',(-2.44788951176421,1.34624996524475,1.57138513513514));
#39116=CARTESIAN_POINT('Ctrl Pts',(-2.47210824713685,-1.30124296703442,
1.72852364864864));
#39117=CARTESIAN_POINT('Ctrl Pts',(-0.275973625536248,-2.77999224892802,
1.88566216216216));
#39118=CARTESIAN_POINT('Ctrl Pts',(2.16802781286073,-1.76187209738162,2.04280067567567));
#39119=CARTESIAN_POINT('Ctrl Pts',(2.66479327803676,0.838697048159531,2.19993918918919));
#39120=CARTESIAN_POINT('Ctrl Pts',(0.76814623510466,2.68597898024514,2.3570777027027));
#39121=CARTESIAN_POINT('Ctrl Pts',(-1.81841914581395,2.1208221280237,2.51421621621621));
#39122=CARTESIAN_POINT('Ctrl Pts',(-2.77175244146736,-0.349174081739879,
2.67135472972972));
#39123=CARTESIAN_POINT('Ctrl Pts',(-1.23560715428754,-2.50555554774625,
2.82849324324324));
#39124=CARTESIAN_POINT('Ctrl Pts',(1.41031161531747,-2.41154623133624,2.98563175675675));
#39125=CARTESIAN_POINT('Ctrl Pts',(2.78954424185296,-0.151581281506301,
3.14277027027027));
#39126=CARTESIAN_POINT('Ctrl Pts',(1.66331845351111,2.24452793077997,3.29990878378378));
#39127=CARTESIAN_POINT('Ctrl Pts',(-0.956834235921451,2.62469088021855,
3.45704729729729));
#39128=CARTESIAN_POINT('Ctrl Pts',(-2.71759622818163,0.647460184837647,
3.61418581081081));
#39129=CARTESIAN_POINT('Ctrl Pts',(-2.03752067689171,-1.91129365535261,
3.77132432432432));
#39130=CARTESIAN_POINT('Ctrl Pts',(0.47257542983782,-2.75339906613161,3.92846283783783));
#39131=CARTESIAN_POINT('Ctrl Pts',(2.55822296043148,-1.12251023841371,4.08560135135135));
#39132=CARTESIAN_POINT('Ctrl Pts',(2.34617571991457,1.51657292659299,4.24273986486486));
#39133=CARTESIAN_POINT('Ctrl Pts',(0.0268861606557786,2.79353021925399,
4.39987837837838));
#39134=CARTESIAN_POINT('Ctrl Pts',(-2.31655148571177,1.56144905936101,4.55701689189189));
#39135=CARTESIAN_POINT('Ctrl Pts',(-2.57935412971408,-1.07306394240484,
4.7141554054054));
#39136=CARTESIAN_POINT('Ctrl Pts',(-0.525482821607704,-2.74379331497496,
4.87129391891892));
#39137=CARTESIAN_POINT('Ctrl Pts',(2.00035639160479,-1.95015595724574,5.02843243243243));
#39138=CARTESIAN_POINT('Ctrl Pts',(2.72955454106374,0.595034417816705,5.18557094594594));
#39139=CARTESIAN_POINT('Ctrl Pts',(1.0071746643292,2.60578839251754,5.34270945945947));
#39140=CARTESIAN_POINT('Ctrl Pts',(-1.61980969583571,2.27612620482886,5.49984797297296));
#39141=CARTESIAN_POINT('Ctrl Pts',(-2.79194499649648,-0.0978625953710016,
5.6569864864865));
#39142=CARTESIAN_POINT('Ctrl Pts',(-1.45646562934828,-2.38395507960311,
5.81412499999999));
#39143=CARTESIAN_POINT('Ctrl Pts',(1.18715361157964,-2.5288733170224,5.97126351351352));
#39144=CARTESIAN_POINT('Ctrl Pts',(2.76451839080433,-0.402457473451116,
6.12840202702702));
#39145=CARTESIAN_POINT('Ctrl Pts',(1.8589019956498,2.08542976904401,6.28554054054054));
#39146=CARTESIAN_POINT('Ctrl Pts',(-0.716306714602523,2.70026640197657,
6.44267905405405));
#39147=CARTESIAN_POINT('Ctrl Pts',(-2.64815703976171,0.889830457882673,
6.59981756756756));
#39148=CARTESIAN_POINT('Ctrl Pts',(-2.20153735786441,-1.71981604046289,
6.75695608108108));
#39149=CARTESIAN_POINT('Ctrl Pts',(0.222416181733502,-2.78479173243988,
6.91409459459459));
#39150=CARTESIAN_POINT('Ctrl Pts',(2.4466042959518,-1.34857753576241,7.0712331081081));
#39151=CARTESIAN_POINT('Ctrl Pts',(2.47334911304448,1.29887571249989,7.22837162162162));
#39152=CARTESIAN_POINT('Ctrl Pts',(0.278629494786153,2.77973012269657,7.38551013513513));
#39153=CARTESIAN_POINT('Ctrl Pts',(-2.16634412474015,1.76394078240349,7.54264864864865));
#39154=CARTESIAN_POINT('Ctrl Pts',(-2.66559305877978,-0.83615046447743,
7.69978716216215));
#39155=CARTESIAN_POINT('Ctrl Pts',(-0.770711640749916,-2.68524440462409,
7.85692567567567));
#39156=CARTESIAN_POINT('Ctrl Pts',(1.81639251383808,-2.12255793467458,8.01406418918919));
#39157=CARTESIAN_POINT('Ctrl Pts',(2.77208469636934,0.346526200869026,8.1712027027027));
#39158=CARTESIAN_POINT('Ctrl Pts',(1.23799993580832,2.50437418705365,8.32834121621622));
#39159=CARTESIAN_POINT('Ctrl Pts',(-1.40800742257503,2.4128922603655,8.48547972972973));
#39160=CARTESIAN_POINT('Ctrl Pts',(-2.78939819763151,0.154245820758651,
8.64261824324324));
#39161=CARTESIAN_POINT('Ctrl Pts',(-1.66546165480147,-2.24293805508635,
8.79975675675676));
#39162=CARTESIAN_POINT('Ctrl Pts',(0.954326572136137,-2.62560372673677,
8.95689527027026));
#39163=CARTESIAN_POINT('Ctrl Pts',(2.71697669134881,-0.650055649344734,
9.11403378378378));
#39164=CARTESIAN_POINT('Ctrl Pts',(2.03934512373477,1.90934627218937,9.2711722972973));
#39165=CARTESIAN_POINT('Ctrl Pts',(-0.469944521571767,2.75384968723896,
9.42831081081079));
#39166=CARTESIAN_POINT('Ctrl Pts',(-2.55715071813987,1.12495248325711,9.58544932432433));
#39167=CARTESIAN_POINT('Ctrl Pts',(-2.34762107913798,-1.51432942746238,
9.74258783783783));
#39168=CARTESIAN_POINT('Ctrl Pts',(-0.0295588149451427,-2.79350652787453,
9.89972635135136));
#39169=CARTESIAN_POINT('Ctrl Pts',(2.31506703223917,-1.56365490661018,10.0568648648649));
#39170=CARTESIAN_POINT('Ctrl Pts',(2.58036243233743,1.07058768363104,10.2140033783784));
#39171=CARTESIAN_POINT('Ctrl Pts',(0.528133174514654,2.74331293137788,10.3711418918919));
#39172=CARTESIAN_POINT('Ctrl Pts',(-1.99854941269714,1.95202221408926,10.5282804054054));
#39173=CARTESIAN_POINT('Ctrl Pts',(-2.73001318151202,-0.59234343939674,
10.6854189189189));
#39174=CARTESIAN_POINT('Ctrl Pts',(-1.0098707589218,-2.60498459805753,10.8425574324324));
#39175=CARTESIAN_POINT('Ctrl Pts',(1.61803174729613,-2.2773674076414,10.999695945946));
#39176=CARTESIAN_POINT('Ctrl Pts',(2.79127527466209,0.0946110570183949,
11.1568344594594));
#39177=CARTESIAN_POINT('Ctrl Pts',(1.46022534703361,2.38369320998594,11.313972972973));
#39178=CARTESIAN_POINT('Ctrl Pts',(-1.1878082887304,2.52773050943662,11.4711114864865));
#39179=CARTESIAN_POINT('Ctrl Pts',(-2.23349531079268,1.11623543008163,11.5758704954955));
#39180=CARTESIAN_POINT('Ctrl Pts',(-2.34668236863853,0.343918483395475,
11.62825));
#39181=CARTESIAN_POINT('',(1.37702479013102,-1.93106208855765,0.));
#39182=CARTESIAN_POINT('Ctrl Pts',(1.37702479013101,-1.93106208855765,-2.4980018054066E-15));
#39183=CARTESIAN_POINT('Ctrl Pts',(2.01255689112068,-1.47786927659557,0.052379504504502));
#39184=CARTESIAN_POINT('Ctrl Pts',(2.79122694355976,0.0967585069099138,
0.157138513513511));
#39185=CARTESIAN_POINT('Ctrl Pts',(1.45451670762985,2.3871808751492,0.314277027027025));
#39186=CARTESIAN_POINT('Ctrl Pts',(-1.18974109900074,2.52679342812162,0.471415540540538));
#39187=CARTESIAN_POINT('Ctrl Pts',(-2.31615344009055,1.00603694073732,0.583793234229858));
#39188=CARTESIAN_POINT('Ctrl Pts',(-2.37458477423974,0.11510370689526,0.643791423414673));
#39189=CARTESIAN_POINT('Ctrl Pts',(-2.37366757034868,0.001844716469488,
0.651410108094984));
#39190=CARTESIAN_POINT('Ctrl Pts',(1.29197400994444,2.64783394680711,-2.46330733588707E-16));
#39191=CARTESIAN_POINT('Ctrl Pts',(1.37074936016223,2.60046826619745,-2.90204607120186E-16));
#39192=CARTESIAN_POINT('Ctrl Pts',(1.44700091320012,2.54930204226795,-5.92854700626308E-16));
#39193=CARTESIAN_POINT('Ctrl Pts',(1.5204041597113,2.49432533414619,-4.68375338513738E-16));
#39194=CARTESIAN_POINT('Ctrl Pts',(1.59876972116939,2.43563200920691,-3.1748808003354E-16));
#39195=CARTESIAN_POINT('Ctrl Pts',(1.67388955782072,2.37259497158855,9.42702435984343E-17));
#39196=CARTESIAN_POINT('Ctrl Pts',(1.74558455766593,2.30559334150577,2.91433543964104E-16));
#39197=CARTESIAN_POINT('Ctrl Pts',(1.78514524738377,2.26862241321206,4.00226572297347E-16));
#39198=CARTESIAN_POINT('Ctrl Pts',(1.82366240526687,2.23044382157621,2.41712413072573E-16));
#39199=CARTESIAN_POINT('Ctrl Pts',(1.86109995619813,2.19111823230724,2.56739074444567E-16));
#39200=CARTESIAN_POINT('Ctrl Pts',(1.87813922122651,2.17321964863167,2.63578284255041E-16));
#39201=CARTESIAN_POINT('Ctrl Pts',(1.89495840460327,2.15507923207588,-5.32738877742354E-17));
#39202=CARTESIAN_POINT('Ctrl Pts',(1.91153266312519,2.13672660521873,-9.0205620750794E-17));
#39203=CARTESIAN_POINT('Ctrl Pts',(1.97664662778045,2.0646261070319,-2.35296368099375E-16));
#39204=CARTESIAN_POINT('Ctrl Pts',(2.03804038590891,1.98919650283574,-3.72373475267393E-16));
#39205=CARTESIAN_POINT('Ctrl Pts',(2.09554796148623,1.91081666271006,-8.32667268468867E-17));
#39206=CARTESIAN_POINT('Ctrl Pts',(2.14343533270609,1.8455486617107,1.57476549926517E-16));
#39207=CARTESIAN_POINT('Ctrl Pts',(2.18862729734747,1.77823406218829,2.53857300975798E-16));
#39208=CARTESIAN_POINT('Ctrl Pts',(2.23100237945407,1.70908145885149,3.19189119579733E-16));
#39209=CARTESIAN_POINT('Ctrl Pts',(2.2495414778757,1.67882719489164,3.47771790218954E-16));
#39210=CARTESIAN_POINT('Ctrl Pts',(2.26754109313608,1.64822104628506,2.94521883274651E-16));
#39211=CARTESIAN_POINT('Ctrl Pts',(2.28498954152194,1.61728023964544,3.19189119579733E-16));
#39212=CARTESIAN_POINT('Ctrl Pts',(2.29543189661598,1.59876312668031,3.33951695310829E-16));
#39213=CARTESIAN_POINT('Ctrl Pts',(2.30567682494647,1.58012614919259,-6.61366324171955E-18));
#39214=CARTESIAN_POINT('Ctrl Pts',(2.31572165746038,1.56137299470242,-1.38777878078145E-17));
#39215=CARTESIAN_POINT('Ctrl Pts',(2.32292320728395,1.54792809393149,-1.90857347710862E-17));
#39216=CARTESIAN_POINT('Ctrl Pts',(2.33002152872364,1.53442403232929,-1.12870283643031E-16));
#39217=CARTESIAN_POINT('Ctrl Pts',(2.33700969851763,1.52087413145422,-1.11022302462516E-16));
#39218=CARTESIAN_POINT('Ctrl Pts',(2.38058260792534,1.43638725996736,-9.94996979838631E-17));
#39219=CARTESIAN_POINT('Ctrl Pts',(2.41994184512486,1.3499998824768,-3.77842799305168E-16));
#39220=CARTESIAN_POINT('Ctrl Pts',(2.45492973401008,1.26206183108408,-3.7470027081099E-16));
#39221=CARTESIAN_POINT('Ctrl Pts',(2.48961375478266,1.17488751738912,-3.71585035023886E-16));
#39222=CARTESIAN_POINT('Ctrl Pts',(2.52000223755862,1.08618841594484,-4.13121512185277E-16));
#39223=CARTESIAN_POINT('Ctrl Pts',(2.54589150534161,0.996296170221892,-3.7470027081099E-16));
#39224=CARTESIAN_POINT('Ctrl Pts',(2.57095558696702,0.909269120898709,-3.37503655671981E-16));
#39225=CARTESIAN_POINT('Ctrl Pts',(2.59180267862827,0.821123009321661,-1.98135956264892E-16));
#39226=CARTESIAN_POINT('Ctrl Pts',(2.60819974692058,0.732162501184589,-2.77555756156289E-16));
#39227=CARTESIAN_POINT('Ctrl Pts',(2.61796168819389,0.679200152025794,-3.24838075693952E-16));
#39228=CARTESIAN_POINT('Ctrl Pts',(2.62614545111416,0.625949276096869,-2.51374357035676E-17));
#39229=CARTESIAN_POINT('Ctrl Pts',(2.63269335080009,0.572476447093945,0.));
#39230=CARTESIAN_POINT('Ctrl Pts',(2.6352683765624,0.5514477327168,9.88554309620052E-18));
#39231=CARTESIAN_POINT('Ctrl Pts',(2.63759088070415,0.530377846603737,-5.43523939458827E-17));
#39232=CARTESIAN_POINT('Ctrl Pts',(2.63965388200594,0.50930758122065,-2.77555756156289E-17));
#39233=CARTESIAN_POINT('Ctrl Pts',(2.64834931960739,0.420497565576959,8.43485582923526E-17));
#39234=CARTESIAN_POINT('Ctrl Pts',(2.65245297898025,0.3315870178655,7.13394232030532E-17));
#39235=CARTESIAN_POINT('Ctrl Pts',(2.65178792227632,0.242870082265014,1.11022302462516E-16));
#39236=CARTESIAN_POINT('Ctrl Pts',(2.65141677862428,0.193360428001277,1.33167855834344E-16));
#39237=CARTESIAN_POINT('Ctrl Pts',(2.64955959473733,0.143911103160085,2.55410202784461E-16));
#39238=CARTESIAN_POINT('Ctrl Pts',(2.64617859082989,0.0945743399740305,
2.77555756156289E-16));
#39239=CARTESIAN_POINT('Ctrl Pts',(2.63998980161557,0.00426541509996067,
2.91350122435194E-16));
#39240=CARTESIAN_POINT('Ctrl Pts',(2.62869784498548,-0.0856678806083358,
1.22336690906674E-16));
#39241=CARTESIAN_POINT('Ctrl Pts',(2.61249699286393,-0.174890907412304,
1.94289029309402E-16));
#39242=CARTESIAN_POINT('Ctrl Pts',(2.59606370990205,-0.265394001643718,
2.67273655542046E-16));
#39243=CARTESIAN_POINT('Ctrl Pts',(2.57457910556097,-0.355167245076682,
-8.63540186836622E-17));
#39244=CARTESIAN_POINT('Ctrl Pts',(2.54820206281091,-0.443829678011398,
-1.94289029309402E-16));
#39245=CARTESIAN_POINT('Ctrl Pts',(2.5433159398537,-0.460253640057088,-2.14283072550056E-16));
#39246=CARTESIAN_POINT('Ctrl Pts',(2.53826078384047,-0.476642310793062,
2.54370247567095E-16));
#39247=CARTESIAN_POINT('Ctrl Pts',(2.53304532831965,-0.49296952041645,2.4980018054066E-16));
#39248=CARTESIAN_POINT('Ctrl Pts',(2.5060606614482,-0.577446189974434,2.26154741365496E-16));
#39249=CARTESIAN_POINT('Ctrl Pts',(2.47475215402615,-0.660408357948197,
3.47506847049484E-16));
#39250=CARTESIAN_POINT('Ctrl Pts',(2.43933604293942,-0.741555503604727,
2.77555756156289E-16));
#39251=CARTESIAN_POINT('Ctrl Pts',(2.40393876465244,-0.822659498618874,
2.07641862313994E-16));
#39252=CARTESIAN_POINT('Ctrl Pts',(2.3644375894048,-0.901951185787608,-1.23823437954767E-16));
#39253=CARTESIAN_POINT('Ctrl Pts',(2.32100582430644,-0.979100944080977,
-1.11022302462516E-16));
#39254=CARTESIAN_POINT('Ctrl Pts',(2.27823644108386,-1.05507408425856,-9.84163982743666E-17));
#39255=CARTESIAN_POINT('Ctrl Pts',(2.23165476456022,-1.1289707546069,2.53313632717541E-16));
#39256=CARTESIAN_POINT('Ctrl Pts',(2.18139506127574,-1.20043719637909,2.77555756156289E-16));
#39257=CARTESIAN_POINT('Ctrl Pts',(2.16608689289344,-1.2222045418435,2.84939454890925E-16));
#39258=CARTESIAN_POINT('Ctrl Pts',(2.15043733121093,-1.24374612322857,4.37114965090439E-17));
#39259=CARTESIAN_POINT('Ctrl Pts',(2.13444972694369,-1.26505107698559,0.));
#39260=CARTESIAN_POINT('Ctrl Pts',(2.12083931058568,-1.28318820912085,-3.72120586158607E-17));
#39261=CARTESIAN_POINT('Ctrl Pts',(2.10698390104784,-1.30115384375424,6.4814165885223E-17));
#39262=CARTESIAN_POINT('Ctrl Pts',(2.09288546869145,-1.31894102140198,5.55111512312578E-17));
#39263=CARTESIAN_POINT('Ctrl Pts',(2.08472665052523,-1.32923453095322,5.01274601200272E-17));
#39264=CARTESIAN_POINT('Ctrl Pts',(2.07648733901943,-1.33946704131009,1.07093663002969E-16));
#39265=CARTESIAN_POINT('Ctrl Pts',(2.06817568052718,-1.3496280615777,1.11022302462516E-16));
#39266=CARTESIAN_POINT('Ctrl Pts',(2.0141423836499,-1.41568388247163,1.36562011828508E-16));
#39267=CARTESIAN_POINT('Ctrl Pts',(1.95696807639868,-1.47883106712894,-2.06909962337776E-16));
#39268=CARTESIAN_POINT('Ctrl Pts',(1.89681447147471,-1.5387754276769,-2.22044604925031E-16));
#39269=CARTESIAN_POINT('Ctrl Pts',(1.83758356202805,-1.5978003023447,-2.36947097397864E-16));
#39270=CARTESIAN_POINT('Ctrl Pts',(1.77546340770889,-1.65372037608364,4.0590157288843E-16));
#39271=CARTESIAN_POINT('Ctrl Pts',(1.71058212140457,-1.70621256947127,4.44089209850063E-16));
#39272=CARTESIAN_POINT('Ctrl Pts',(1.64772546517897,-1.75706673624623,4.81085195985522E-16));
#39273=CARTESIAN_POINT('Ctrl Pts',(1.58227673616169,-1.80470390837557,2.58606592525932E-16));
#39274=CARTESIAN_POINT('Ctrl Pts',(1.5143365021986,-1.84878472647799,2.77555756156289E-16));
#39275=CARTESIAN_POINT('Ctrl Pts',(1.46963595841736,-1.87778722506477,2.90023153883192E-16));
#39276=CARTESIAN_POINT('Ctrl Pts',(1.42385657678108,-1.90524929950103,3.23574125955808E-17));
#39277=CARTESIAN_POINT('Ctrl Pts',(1.37702479013104,-1.93106208855763,5.55111512312578E-17));
#39278=CARTESIAN_POINT('Ctrl Pts',(0.261124777554701,2.92529416030267,11.058));
#39279=CARTESIAN_POINT('Ctrl Pts',(0.712806568001128,2.88599464153458,11.0335796606559));
#39280=CARTESIAN_POINT('Ctrl Pts',(1.15551467718148,2.74786827548953,11.0091593213117));
#39281=CARTESIAN_POINT('Ctrl Pts',(1.53904161881194,2.51335023952951,10.9847389819676));
#39282=CARTESIAN_POINT('Ctrl Pts',(2.36167356031087,2.01032944412425,10.9323594774631));
#39283=CARTESIAN_POINT('Ctrl Pts',(2.91203354584656,1.06384412118684,10.8799799729586));
#39284=CARTESIAN_POINT('Ctrl Pts',(2.94465829055491,0.100220893818898,10.8276004684541));
#39285=CARTESIAN_POINT('Ctrl Pts',(2.97728303526326,-0.863402333549067,
10.7752209639496));
#39286=CARTESIAN_POINT('Ctrl Pts',(2.49217253914424,-1.84416346534755,10.7228414594451));
#39287=CARTESIAN_POINT('Ctrl Pts',(1.70632723287924,-2.40227529678238,10.6704619549406));
#39288=CARTESIAN_POINT('Ctrl Pts',(0.92048192661426,-2.96038712821718,10.6180824504361));
#39289=CARTESIAN_POINT('Ctrl Pts',(-0.166098189796688,-3.09584965928835,
10.5657029459315));
#39290=CARTESIAN_POINT('Ctrl Pts',(-1.0650088521454,-2.74748941090806,10.513323441427));
#39291=CARTESIAN_POINT('Ctrl Pts',(-1.96391951449414,-2.39912916252775,
10.4609439369225));
#39292=CARTESIAN_POINT('Ctrl Pts',(-2.67516072278063,-1.56694613469595,
10.408564432418));
#39293=CARTESIAN_POINT('Ctrl Pts',(-2.87955920487239,-0.624834891848815,
10.3561849279135));
#39294=CARTESIAN_POINT('Ctrl Pts',(-2.92379628688831,-0.420937818389941,
10.3448486576389));
#39295=CARTESIAN_POINT('Ctrl Pts',(-2.94429281596354,-0.211891698741057,
10.3335123873642));
#39296=CARTESIAN_POINT('Ctrl Pts',(-2.94242444587263,-0.00248500551853048,
10.3221761170896));
#39297=CARTESIAN_POINT('Origin',(0.,0.,-1.84858989190501));
#39298=CARTESIAN_POINT('',(-1.37702479013099,-1.93106208855767,0.));
#39299=CARTESIAN_POINT('Ctrl Pts',(-1.37989654081094,-1.93326688769301,
3.07371315899641E-16));
#39300=CARTESIAN_POINT('Ctrl Pts',(-0.801986922861967,-2.34019513141193,
0.0475906520026623));
#39301=CARTESIAN_POINT('Ctrl Pts',(0.824868299691477,-2.62988338064349,
0.147626409229032));
#39302=CARTESIAN_POINT('Ctrl Pts',(2.66596861578497,-0.838738147770652,
0.30010727167911));
#39303=CARTESIAN_POINT('Ctrl Pts',(2.16631806184957,1.76615982799916,0.457442587350233));
#39304=CARTESIAN_POINT('Ctrl Pts',(-0.283824062622952,2.78024166545816,
0.614777903021357));
#39305=CARTESIAN_POINT('Ctrl Pts',(-2.10236314538525,1.54689613835291,0.745160337872953));
#39306=CARTESIAN_POINT('Ctrl Pts',(-2.3682722008076,0.381486792202907,0.823097667500842));
#39307=CARTESIAN_POINT('Ctrl Pts',(-2.36802324146013,0.000186122305323062,
0.848589891905023));
#39308=CARTESIAN_POINT('Origin',(0.,0.,0.));
#39309=CARTESIAN_POINT('Ctrl Pts',(-1.03908919352509,2.13201587949044,-0.329233991005384));
#39310=CARTESIAN_POINT('Ctrl Pts',(-1.74163600084562,1.78961280339009,-0.276788885781676));
#39311=CARTESIAN_POINT('Ctrl Pts',(-2.77044124913769,0.362429281341372,
-0.171898675334261));
#39312=CARTESIAN_POINT('Ctrl Pts',(-1.82442757362648,-2.1194917921021,-0.0145633596631371));
#39313=CARTESIAN_POINT('Ctrl Pts',(0.766254154833431,-2.68690713172521,
0.142771956007986));
#39314=CARTESIAN_POINT('Ctrl Pts',(2.66596861578497,-0.838738147770652,
0.30010727167911));
#39315=CARTESIAN_POINT('Ctrl Pts',(2.16631806184957,1.76615982799916,0.457442587350233));
#39316=CARTESIAN_POINT('Ctrl Pts',(-0.283824062622952,2.78024166545816,
0.614777903021357));
#39317=CARTESIAN_POINT('Ctrl Pts',(-2.47829466728951,1.29193683314281,0.772113218692479));
#39318=CARTESIAN_POINT('Ctrl Pts',(-2.44182858239548,-1.35964121596809,
0.929448534363604));
#39319=CARTESIAN_POINT('Ctrl Pts',(-0.207121339063888,-2.78711087979173,
1.08678385003473));
#39320=CARTESIAN_POINT('Ctrl Pts',(2.21401803077907,-1.70561830406782,1.24411916570585));
#39321=CARTESIAN_POINT('Ctrl Pts',(2.64205485235054,0.911349150745493,1.40145448137697));
#39322=CARTESIAN_POINT('Ctrl Pts',(0.691640660298454,2.70787919402874,1.5587897970481));
#39323=CARTESIAN_POINT('Ctrl Pts',(-1.88140253096646,2.06671733364312,1.71612511271922));
#39324=CARTESIAN_POINT('Ctrl Pts',(-2.76076141176456,-0.43496057134077,
1.87346042839035));
#39325=CARTESIAN_POINT('Ctrl Pts',(-1.15481219883121,-2.54507342378116,
2.03079574406147));
#39326=CARTESIAN_POINT('Ctrl Pts',(1.49072764255621,-2.36404822464922,2.18813105973259));
#39327=CARTESIAN_POINT('Ctrl Pts',(2.79427705549031,-0.0548463935276453,
2.34546637540372));
#39328=CARTESIAN_POINT('Ctrl Pts',(1.5823475414007,2.30372918060613,2.50280169107483));
#39329=CARTESIAN_POINT('Ctrl Pts',(-1.05405113312049,2.58842974112365,2.66013700674597));
#39330=CARTESIAN_POINT('Ctrl Pts',(-2.74156638658485,0.542960359863138,
2.81747232241708));
#39331=CARTESIAN_POINT('Ctrl Pts',(-1.9610543025963,-1.99129560121778,2.97480763808821));
#39332=CARTESIAN_POINT('Ctrl Pts',(0.584848394656438,-2.73293698550247,
3.13214295375933));
#39333=CARTESIAN_POINT('Ctrl Pts',(2.60425579784155,-1.01431944186932,3.28947826943046));
#39334=CARTESIAN_POINT('Ctrl Pts',(2.27924634057658,1.61741407950708,3.44681358510158));
#39335=CARTESIAN_POINT('Ctrl Pts',(-0.0975982492034651,2.79311059143494,
3.6041489007727));
#39336=CARTESIAN_POINT('Ctrl Pts',(-2.38658243027454,1.45437838755459,3.76148421644382));
#39337=CARTESIAN_POINT('Ctrl Pts',(-2.52710481755741,-1.19362198012869,
3.91881953211495));
#39338=CARTESIAN_POINT('Ctrl Pts',(-0.392663608746353,-2.76709368867159,
4.07615484778607));
#39339=CARTESIAN_POINT('Ctrl Pts',(2.09526330020315,-1.8495577562663,4.23349016345719));
#39340=CARTESIAN_POINT('Ctrl Pts',(2.69698125586998,0.732996791565816,4.39082547912832));
#39341=CARTESIAN_POINT('Ctrl Pts',(0.870808554093777,2.65568911080063,4.54816079479944));
#39342=CARTESIAN_POINT('Ctrl Pts',(-1.73928800639316,2.18766300463189,4.70549611047057));
#39343=CARTESIAN_POINT('Ctrl Pts',(-2.78363356575401,-0.249752602863106,
4.86283142614169));
#39344=CARTESIAN_POINT('Ctrl Pts',(-1.32208186928512,-2.46233460804071,
5.02016674181281));
#39345=CARTESIAN_POINT('Ctrl Pts',(1.32964132424929,-2.45826079574207,5.17750205748394));
#39346=CARTESIAN_POINT('Ctrl Pts',(2.78438780839412,-0.241198514719961,
5.33483737315506));
#39347=CARTESIAN_POINT('Ctrl Pts',(1.73255804842731,2.19299676239354,5.49217268882618));
#39348=CARTESIAN_POINT('Ctrl Pts',(-0.878964234485193,2.65300095467984,
5.64950800449731));
#39349=CARTESIAN_POINT('Ctrl Pts',(-2.69922070918587,0.72470666765315,5.80684332016843));
#39350=CARTESIAN_POINT('Ctrl Pts',(-2.08957051396587,-1.85598686908106,
5.96417863583956));
#39351=CARTESIAN_POINT('Ctrl Pts',(0.401163844498212,-2.76587414046649,
6.12151395151068));
#39352=CARTESIAN_POINT('Ctrl Pts',(2.53076037597685,-1.18585163930103,6.2788492671818));
#39353=CARTESIAN_POINT('Ctrl Pts',(2.38210248511723,1.46170446446183,6.43618458285292));
#39354=CARTESIAN_POINT('Ctrl Pts',(0.0890157606711408,2.793397283841,6.59351989852405));
#39355=CARTESIAN_POINT('Ctrl Pts',(-2.28420520026003,1.61040330172691,6.75085521419516));
#39356=CARTESIAN_POINT('Ctrl Pts',(-2.60112693645964,-1.02231641451357,
6.9081905298663));
#39357=CARTESIAN_POINT('Ctrl Pts',(-0.57644849505612,-2.73472106868152,
7.06552584553741));
#39358=CARTESIAN_POINT('Ctrl Pts',(1.96716344393165,-1.98526073259378,7.22286116120855));
#39359=CARTESIAN_POINT('Ctrl Pts',(2.73988515609665,0.551381466653972,7.38019647687966));
#39360=CARTESIAN_POINT('Ctrl Pts',(1.04609303646807,2.5916561403346,7.53753179255079));
#39361=CARTESIAN_POINT('Ctrl Pts',(-1.58941846186445,2.2988564868904,7.69486710822191));
#39362=CARTESIAN_POINT('Ctrl Pts',(-2.79409530723714,-0.0634318507917163,
7.85220242389303));
#39363=CARTESIAN_POINT('Ctrl Pts',(-1.48345697628832,-2.36861723168749,
8.00953773956416));
#39364=CARTESIAN_POINT('Ctrl Pts',(1.16262680634646,-2.54151354917186,8.16687305523529));
#39365=CARTESIAN_POINT('Ctrl Pts',(2.76208455499713,-0.426475157784177,
8.3242083709064));
#39366=CARTESIAN_POINT('Ctrl Pts',(1.8750440359881,2.07248692819523,8.48154368657753));
#39367=CARTESIAN_POINT('Ctrl Pts',(-0.699958537943023,2.7057439570526,8.63887900224866));
#39368=CARTESIAN_POINT('Ctrl Pts',(-2.6448406647993,0.903221864868725,8.79621431791976));
#39369=CARTESIAN_POINT('Ctrl Pts',(-2.20877058145475,-1.7124032551425,8.95354963359091));
#39370=CARTESIAN_POINT('Ctrl Pts',(0.215690902196592,-2.78647992051942,
9.11088494926201));
#39371=CARTESIAN_POINT('Ctrl Pts',(2.4459813653409,-1.35209655994371,9.26822026493315));
#39372=CARTESIAN_POINT('Ctrl Pts',(2.47433880171217,1.29947749716991,9.42555558060427));
#39373=CARTESIAN_POINT('Ctrl Pts',(0.275231669725872,2.78123058171878,9.58289089627539));
#39374=CARTESIAN_POINT('Ctrl Pts',(-2.17164161907558,1.7592467736877,9.74022621194653));
#39375=CARTESIAN_POINT('Ctrl Pts',(-2.66355657074516,-0.846449946443288,
9.89756152761763));
#39376=CARTESIAN_POINT('Ctrl Pts',(-0.757654725048104,-2.69016151139635,
10.0548968432888));
#39377=CARTESIAN_POINT('Ctrl Pts',(1.83027666927001,-2.11210170665972,10.2122321589599));
#39378=CARTESIAN_POINT('Ctrl Pts',(2.77060484795253,0.367287133540841,10.369567474631));
#39379=CARTESIAN_POINT('Ctrl Pts',(1.21665350181368,2.51610800548609,10.5269027903021));
#39380=CARTESIAN_POINT('Ctrl Pts',(-1.43234772356642,2.39972494583597,10.6842381059733));
#39381=CARTESIAN_POINT('Ctrl Pts',(-2.79231938150401,0.123316482315984,
10.8415734216444));
#39382=CARTESIAN_POINT('Ctrl Pts',(-1.63779792657952,-2.26461658842463,
10.9989087373155));
#39383=CARTESIAN_POINT('Ctrl Pts',(0.989622905930635,-2.61290295808564,
11.1562440529866));
#39384=CARTESIAN_POINT('Ctrl Pts',(2.72902843688469,-0.61088887604173,11.3135793686578));
#39385=CARTESIAN_POINT('Ctrl Pts',(2.00599839187704,1.9449087769569,11.4709146843289));
#39386=CARTESIAN_POINT('Ctrl Pts',(0.328567026486064,2.47549058867235,11.5758048947763));
#39387=CARTESIAN_POINT('Ctrl Pts',(-0.439445221994061,2.3306835819919,11.62825));
#39388=CARTESIAN_POINT('Ctrl Pts',(-1.12236674703447,2.30288577939268,-0.219489327336923));
#39389=CARTESIAN_POINT('Ctrl Pts',(-1.881218999262,1.93304089110777,-0.167044222113215));
#39390=CARTESIAN_POINT('Ctrl Pts',(-2.9924775967461,0.391476088928602,-0.0621540116657994));
#39391=CARTESIAN_POINT('Ctrl Pts',(-1.97064588273166,-2.28935795203269,
0.0951813040053245));
#39392=CARTESIAN_POINT('Ctrl Pts',(0.82766540978493,-2.90224865758394,0.252516619676447));
#39393=CARTESIAN_POINT('Ctrl Pts',(2.87963202931947,-0.905958614903406,
0.409851935347572));
#39394=CARTESIAN_POINT('Ctrl Pts',(2.33993710190716,1.90770828264466,0.567187251018694));
#39395=CARTESIAN_POINT('Ctrl Pts',(-0.306571073860874,3.00306346507554,
0.724522566689817));
#39396=CARTESIAN_POINT('Ctrl Pts',(-2.67691699735827,1.39547879991837,0.881857882360941));
#39397=CARTESIAN_POINT('Ctrl Pts',(-2.63752834686069,-1.46860933422193,
1.03919319803207));
#39398=CARTESIAN_POINT('Ctrl Pts',(-0.223721028969555,-3.01048321093979,
1.19652851370319));
#39399=CARTESIAN_POINT('Ctrl Pts',(2.39145997337443,-1.84231467283839,1.35386382937431));
#39400=CARTESIAN_POINT('Ctrl Pts',(2.85380170306596,0.984389009248359,1.51119914504543));
#39401=CARTESIAN_POINT('Ctrl Pts',(0.747072034675363,2.92490152077689,1.66853446071656));
#39402=CARTESIAN_POINT('Ctrl Pts',(-2.03218708432488,2.23235389729304,1.82586977638768));
#39403=CARTESIAN_POINT('Ctrl Pts',(-2.98202197113476,-0.469820381720866,
1.98320509205881));
#39404=CARTESIAN_POINT('Ctrl Pts',(-1.24736434476896,-2.74904772122835,
2.14054040772993));
#39405=CARTESIAN_POINT('Ctrl Pts',(1.61020165094208,-2.55351430104939,2.29787572340105));
#39406=CARTESIAN_POINT('Ctrl Pts',(3.01822371806624,-0.0592420445461263,
2.45521103907218));
#39407=CARTESIAN_POINT('Ctrl Pts',(1.70916440454448,2.48836100172844,2.6125463547433));
#39408=CARTESIAN_POINT('Ctrl Pts',(-1.13852780768032,2.79587882019688,2.76988167041443));
#39409=CARTESIAN_POINT('Ctrl Pts',(-2.9612885652785,0.586475787319947,2.92721698608554));
#39410=CARTESIAN_POINT('Ctrl Pts',(-2.11822252803541,-2.15088750826171,
3.08455230175667));
#39411=CARTESIAN_POINT('Ctrl Pts',(0.631720928587459,-2.95196756292179,
3.24188761742779));
#39412=CARTESIAN_POINT('Ctrl Pts',(2.81297325242419,-1.09561182958951,3.39922293309892));
#39413=CARTESIAN_POINT('Ctrl Pts',(2.46191599037299,1.74704134191371,3.55655824877004));
#39414=CARTESIAN_POINT('Ctrl Pts',(-0.105420237413036,3.01696376802969,
3.71389356444116));
#39415=CARTESIAN_POINT('Ctrl Pts',(-2.57785450516496,1.57093919364055,3.87122888011228));
#39416=CARTESIAN_POINT('Ctrl Pts',(-2.72963902538035,-1.28928452665457,
4.02856419578341));
#39417=CARTESIAN_POINT('Ctrl Pts',(-0.424133539231963,-2.98886174685155,
4.18589951145453));
#39418=CARTESIAN_POINT('Ctrl Pts',(2.26318767347756,-1.99779011781522,4.34323482712566));
#39419=CARTESIAN_POINT('Ctrl Pts',(2.91313016998542,0.791742643136777,4.50057014279678));
#39420=CARTESIAN_POINT('Ctrl Pts',(0.940599296228219,2.86852867588043,4.6579054584679));
#39421=CARTESIAN_POINT('Ctrl Pts',(-1.87868282535885,2.36299272999521,4.81524077413902));
#39422=CARTESIAN_POINT('Ctrl Pts',(-3.00672720840483,-0.269768965152914,
4.97257608981016));
#39423=CARTESIAN_POINT('Ctrl Pts',(-1.42803980273229,-2.65967782299944,
5.12991140548127));
#39424=CARTESIAN_POINT('Ctrl Pts',(1.43620510839645,-2.65527751599392,5.28724672115241));
#39425=CARTESIAN_POINT('Ctrl Pts',(3.00754189963992,-0.260529311672868,
5.44458203682351));
#39426=CARTESIAN_POINT('Ctrl Pts',(1.87141349653044,2.36875396048986,5.60191735249465));
#39427=CARTESIAN_POINT('Ctrl Pts',(-0.949408611663097,2.86562507813386,
5.75925266816576));
#39428=CARTESIAN_POINT('Ctrl Pts',(-2.9155491037487,0.782788109236974,5.9165879838369));
#39429=CARTESIAN_POINT('Ctrl Pts',(-2.25703864025646,-2.00473449033026,
6.07392329950801));
#39430=CARTESIAN_POINT('Ctrl Pts',(0.433315024333776,-2.98754445824887,
6.23125861517914));
#39431=CARTESIAN_POINT('Ctrl Pts',(2.73358755765012,-1.28089143373012,6.38859393085026));
#39432=CARTESIAN_POINT('Ctrl Pts',(2.57301551588047,1.57885241721953,6.54592924652138));
#39433=CARTESIAN_POINT('Ctrl Pts',(0.0961499074014511,3.01727343732968,
6.70326456219251));
#39434=CARTESIAN_POINT('Ctrl Pts',(-2.46727227667312,1.73946868703451,6.86059987786364));
#39435=CARTESIAN_POINT('Ctrl Pts',(-2.80959362919934,-1.104249717683,7.01793519353475));
#39436=CARTESIAN_POINT('Ctrl Pts',(-0.622647821053927,-2.95389463101813,
7.17527050920589));
#39437=CARTESIAN_POINT('Ctrl Pts',(2.12482128503379,-2.14436897654329,7.33260582487699));
#39438=CARTESIAN_POINT('Ctrl Pts',(2.95947259297716,0.59557180168919,7.48994114054813));
#39439=CARTESIAN_POINT('Ctrl Pts',(1.12993191128569,2.79936379839662,7.64727645621924));
#39440=CARTESIAN_POINT('Ctrl Pts',(-1.71680202222819,2.4830977871468,7.80461177189038));
#39441=CARTESIAN_POINT('Ctrl Pts',(-3.01802740364303,-0.0685155812177535,
7.96194708756148));
#39442=CARTESIAN_POINT('Ctrl Pts',(-1.60234827887482,-2.55844949005786,
8.11928240323263));
#39443=CARTESIAN_POINT('Ctrl Pts',(1.25580525212405,-2.74520254132467,8.27661771890373));
#39444=CARTESIAN_POINT('Ctrl Pts',(2.98345115736347,-0.460654906735591,
8.43395303457487));
#39445=CARTESIAN_POINT('Ctrl Pts',(2.02531898929576,2.23858589461288,8.591288350246));
#39446=CARTESIAN_POINT('Ctrl Pts',(-0.756056546623237,2.92259515574686,
8.74862366591711));
#39447=CARTESIAN_POINT('Ctrl Pts',(-2.85681078378342,0.975610363999675,
8.90595898158824));
#39448=CARTESIAN_POINT('Ctrl Pts',(-2.38579196848608,-1.84964340218511,
9.06329429725935));
#39449=CARTESIAN_POINT('Ctrl Pts',(0.232977397678477,-3.00980168358836,
9.2206296129305));
#39450=CARTESIAN_POINT('Ctrl Pts',(2.6420139535965,-1.46046001355504,9.37796492860159));
#39451=CARTESIAN_POINT('Ctrl Pts',(2.67264408988566,1.40362380865033,9.53530024427275));
#39452=CARTESIAN_POINT('Ctrl Pts',(0.297290045701602,3.00413163779202,9.69263555994384));
#39453=CARTESIAN_POINT('Ctrl Pts',(-2.34568731434669,1.90024118325806,9.84997087561499));
#39454=CARTESIAN_POINT('Ctrl Pts',(-2.87702667151006,-0.914288473825907,
10.0073061912861));
#39455=CARTESIAN_POINT('Ctrl Pts',(-0.818376780767691,-2.90576385873112,
10.1646415069572));
#39456=CARTESIAN_POINT('Ctrl Pts',(1.97696375273877,-2.2813755899699,10.3219768226283));
#39457=CARTESIAN_POINT('Ctrl Pts',(2.99265430714862,0.396723272524227,10.4793121382995));
#39458=CARTESIAN_POINT('Ctrl Pts',(1.31416190410585,2.71776087645035,10.6366474539706));
#39459=CARTESIAN_POINT('Ctrl Pts',(-1.54714288738549,2.59205032447523,10.7939827696417));
#39460=CARTESIAN_POINT('Ctrl Pts',(-3.01610914676913,0.133199652133039,
10.9513180853128));
#39461=CARTESIAN_POINT('Ctrl Pts',(-1.76905884750739,-2.44611374025332,
11.108653400984));
#39462=CARTESIAN_POINT('Ctrl Pts',(1.06893599571762,-2.82231343724637,11.2659887166551));
#39463=CARTESIAN_POINT('Ctrl Pts',(2.94774576461505,-0.659848418090555,
11.4233240323262));
#39464=CARTESIAN_POINT('Ctrl Pts',(2.1667686505423,2.10078302312668,11.5806593479973));
#39465=CARTESIAN_POINT('Ctrl Pts',(0.35489995180194,2.67388818653474,11.6855495584447));
#39466=CARTESIAN_POINT('Ctrl Pts',(-0.474664453622185,2.51747565713064,
11.7379946636685));
#39467=CARTESIAN_POINT('Ctrl Pts',(-1.20564430054384,2.47375567929493,-0.109744663668461));
#39468=CARTESIAN_POINT('Ctrl Pts',(-2.02080199767838,2.07646897882546,-0.0572995584447534));
#39469=CARTESIAN_POINT('Ctrl Pts',(-3.21451394435451,0.420522896515832,
0.0475906520026618));
#39470=CARTESIAN_POINT('Ctrl Pts',(-2.11686419183683,-2.45922411196328,
0.204925967673786));
#39471=CARTESIAN_POINT('Ctrl Pts',(0.88907666473643,-3.11759018344267,0.362261283344908));
#39472=CARTESIAN_POINT('Ctrl Pts',(3.09329544285396,-0.973179082036162,
0.519596599016033));
#39473=CARTESIAN_POINT('Ctrl Pts',(2.51355614196476,2.04925673729017,0.676931914687155));
#39474=CARTESIAN_POINT('Ctrl Pts',(-0.329318085098797,3.22588526469291,
0.83426723035828));
#39475=CARTESIAN_POINT('Ctrl Pts',(-2.87553932742704,1.49902076669393,0.991602546029402));
#39476=CARTESIAN_POINT('Ctrl Pts',(-2.8332281113259,-1.57757745247578,1.14893786170053));
#39477=CARTESIAN_POINT('Ctrl Pts',(-0.240320718875223,-3.23385554208785,
1.30627317737165));
#39478=CARTESIAN_POINT('Ctrl Pts',(2.5689019159698,-1.97901104160895,1.46360849304277));
#39479=CARTESIAN_POINT('Ctrl Pts',(3.06554855378139,1.05742886775122,1.6209438087139));
#39480=CARTESIAN_POINT('Ctrl Pts',(0.802503409052275,3.14192384752506,1.77827912438502));
#39481=CARTESIAN_POINT('Ctrl Pts',(-2.18297163768331,2.39799046094296,1.93561444005614));
#39482=CARTESIAN_POINT('Ctrl Pts',(-3.20328253050495,-0.504680192100957,
2.09294975572727));
#39483=CARTESIAN_POINT('Ctrl Pts',(-1.33991649070671,-2.95302201867555,
2.25028507139839));
#39484=CARTESIAN_POINT('Ctrl Pts',(1.72967565932795,-2.74298037744955,2.40762038706951));
#39485=CARTESIAN_POINT('Ctrl Pts',(3.24217038064216,-0.0636376955646108,
2.56495570274064));
#39486=CARTESIAN_POINT('Ctrl Pts',(1.83598126768827,2.67299282285076,2.72229101841176));
#39487=CARTESIAN_POINT('Ctrl Pts',(-1.22300448224015,3.00332789927011,2.87962633408289));
#39488=CARTESIAN_POINT('Ctrl Pts',(-3.18101074397215,0.629991214776759,
3.036961649754));
#39489=CARTESIAN_POINT('Ctrl Pts',(-2.27539075347452,-2.31047941530565,
3.19429696542514));
#39490=CARTESIAN_POINT('Ctrl Pts',(0.678593462518484,-3.1709981403411,3.35163228109625));
#39491=CARTESIAN_POINT('Ctrl Pts',(3.02169070700682,-1.1769042173097,3.50896759676738));
#39492=CARTESIAN_POINT('Ctrl Pts',(2.64458564016939,1.87666860432035,3.6663029124385));
#39493=CARTESIAN_POINT('Ctrl Pts',(-0.113242225622608,3.24081694462443,
3.82363822810962));
#39494=CARTESIAN_POINT('Ctrl Pts',(-2.76912658005537,1.68749999972651,3.98097354378075));
#39495=CARTESIAN_POINT('Ctrl Pts',(-2.93217323320329,-1.38494707318046,
4.13830885945187));
#39496=CARTESIAN_POINT('Ctrl Pts',(-0.45560346971757,-3.21062980503151,
4.295644175123));
#39497=CARTESIAN_POINT('Ctrl Pts',(2.43111204675198,-2.14602247936414,4.45297949079412));
#39498=CARTESIAN_POINT('Ctrl Pts',(3.12927908410086,0.850488494707743,4.61031480646524));
#39499=CARTESIAN_POINT('Ctrl Pts',(1.01039003836266,3.08136824096022,4.76765012213636));
#39500=CARTESIAN_POINT('Ctrl Pts',(-2.01807764432454,2.53832245535854,4.92498543780749));
#39501=CARTESIAN_POINT('Ctrl Pts',(-3.22982085105565,-0.289785327442726,
5.08232075347861));
#39502=CARTESIAN_POINT('Ctrl Pts',(-1.53399773617946,-2.85702103795818,
5.23965606914974));
#39503=CARTESIAN_POINT('Ctrl Pts',(1.5427688925436,-2.85229423624577,5.39699138482085));
#39504=CARTESIAN_POINT('Ctrl Pts',(3.23069599088573,-0.279860108625777,
5.55432670049199));
#39505=CARTESIAN_POINT('Ctrl Pts',(2.01026894463356,2.54451115858618,5.7116620161631));
#39506=CARTESIAN_POINT('Ctrl Pts',(-1.019852988841,3.07824920158788,5.86899733183423));
#39507=CARTESIAN_POINT('Ctrl Pts',(-3.13187749831153,0.840869550820803,
6.02633264750535));
#39508=CARTESIAN_POINT('Ctrl Pts',(-2.42450676654705,-2.15348211157947,
6.18366796317648));
#39509=CARTESIAN_POINT('Ctrl Pts',(0.465466204169338,-3.20921477603124,
6.3410032788476));
#39510=CARTESIAN_POINT('Ctrl Pts',(2.93641473932339,-1.3759312281592,6.49833859451872));
#39511=CARTESIAN_POINT('Ctrl Pts',(2.76392854664371,1.69600036997724,6.65567391018985));
#39512=CARTESIAN_POINT('Ctrl Pts',(0.103284054131762,3.24114959081836,6.81300922586097));
#39513=CARTESIAN_POINT('Ctrl Pts',(-2.65033935308621,1.86853407234211,6.97034454153209));
#39514=CARTESIAN_POINT('Ctrl Pts',(-3.01806032193904,-1.18618302085242,
7.12767985720322));
#39515=CARTESIAN_POINT('Ctrl Pts',(-0.668847147051728,-3.17306819335475,
7.28501517287434));
#39516=CARTESIAN_POINT('Ctrl Pts',(2.28247912613591,-2.30347722049279,7.44235048854546));
#39517=CARTESIAN_POINT('Ctrl Pts',(3.17906002985769,0.639762136724403,7.59968580421659));
#39518=CARTESIAN_POINT('Ctrl Pts',(1.2137707861033,3.00707145645863,7.75702111988771));
#39519=CARTESIAN_POINT('Ctrl Pts',(-1.84418558259193,2.66733908740319,7.91435643555884));
#39520=CARTESIAN_POINT('Ctrl Pts',(-3.24195950004891,-0.0735993116437874,
8.07169175122995));
#39521=CARTESIAN_POINT('Ctrl Pts',(-1.7212395814613,-2.74828174842822,8.22902706690109));
#39522=CARTESIAN_POINT('Ctrl Pts',(1.34898369790163,-2.94889153347749,8.38636238257219));
#39523=CARTESIAN_POINT('Ctrl Pts',(3.20481775972981,-0.494834655687006,
8.54369769824334));
#39524=CARTESIAN_POINT('Ctrl Pts',(2.17559394260342,2.40468486103055,8.70103301391445));
#39525=CARTESIAN_POINT('Ctrl Pts',(-0.812154555303452,3.13944635444111,
8.85836832958556));
#39526=CARTESIAN_POINT('Ctrl Pts',(-3.06878090276754,1.04799886313063,9.01570364525671));
#39527=CARTESIAN_POINT('Ctrl Pts',(-2.56281335551741,-1.98688354922771,
9.17303896092782));
#39528=CARTESIAN_POINT('Ctrl Pts',(0.250263893160364,-3.23312344665729,
9.33037427659894));
#39529=CARTESIAN_POINT('Ctrl Pts',(2.83804654185209,-1.56882346716636,9.48770959227006));
#39530=CARTESIAN_POINT('Ctrl Pts',(2.87094937805915,1.50777012013074,9.64504490794121));
#39531=CARTESIAN_POINT('Ctrl Pts',(0.31934842167733,3.22703269386527,9.8023802236123));
#39532=CARTESIAN_POINT('Ctrl Pts',(-2.5197330096178,2.04123559282842,9.95971553928346));
#39533=CARTESIAN_POINT('Ctrl Pts',(-3.09049677227496,-0.982127001208522,
10.1170508549545));
#39534=CARTESIAN_POINT('Ctrl Pts',(-0.879098836487281,-3.1213662060659,
10.2743861706257));
#39535=CARTESIAN_POINT('Ctrl Pts',(2.12365083620754,-2.45064947328008,10.4317214862968));
#39536=CARTESIAN_POINT('Ctrl Pts',(3.2147037663447,0.426159411507612,10.5890568019679));
#39537=CARTESIAN_POINT('Ctrl Pts',(1.41167030639802,2.9194137474146,10.7463921176391));
#39538=CARTESIAN_POINT('Ctrl Pts',(-1.66193805120456,2.78437570311449,10.9037274333102));
#39539=CARTESIAN_POINT('Ctrl Pts',(-3.23989891203425,0.143082821950096,
11.0610627489813));
#39540=CARTESIAN_POINT('Ctrl Pts',(-1.90031976843527,-2.627610892082,11.2183980646524));
#39541=CARTESIAN_POINT('Ctrl Pts',(1.1482490855046,-3.0317239164071,11.3757333803236));
#39542=CARTESIAN_POINT('Ctrl Pts',(3.16646309234541,-0.708807960139384,
11.5330686959947));
#39543=CARTESIAN_POINT('Ctrl Pts',(2.32753890920755,2.25665726929647,11.6904040116658));
#39544=CARTESIAN_POINT('Ctrl Pts',(0.381232877117816,2.87228578439713,11.7952942221132));
#39545=CARTESIAN_POINT('Ctrl Pts',(-0.50988368525031,2.70426773226937,11.8477393273369));
#39546=CARTESIAN_POINT('Ctrl Pts',(-1.28892185405322,2.64462557919718,0.));
#39547=CARTESIAN_POINT('Ctrl Pts',(-2.16038499609476,2.21989706654315,0.0524451052237078));
#39548=CARTESIAN_POINT('Ctrl Pts',(-3.43655029196293,0.449569704103062,
0.157335315671123));
#39549=CARTESIAN_POINT('Ctrl Pts',(-2.26308250094201,-2.62909027189387,
0.314670631342247));
#39550=CARTESIAN_POINT('Ctrl Pts',(0.950487919687924,-3.33293170930141,
0.47200594701337));
#39551=CARTESIAN_POINT('Ctrl Pts',(3.30695885638846,-1.04039954916892,0.629341262684495));
#39552=CARTESIAN_POINT('Ctrl Pts',(2.68717518202235,2.19080519193567,0.786676578355616));
#39553=CARTESIAN_POINT('Ctrl Pts',(-0.352065096336719,3.44870706431028,
0.944011894026741));
#39554=CARTESIAN_POINT('Ctrl Pts',(-3.0741616574958,1.60256273346949,1.10134720969786));
#39555=CARTESIAN_POINT('Ctrl Pts',(-3.02892787579111,-1.68654557072963,
1.25868252536899));
#39556=CARTESIAN_POINT('Ctrl Pts',(-0.256920408780888,-3.45722787323591,
1.41601784104011));
#39557=CARTESIAN_POINT('Ctrl Pts',(2.74634385856517,-2.11570741037952,1.57335315671124));
#39558=CARTESIAN_POINT('Ctrl Pts',(3.27729540449682,1.13046872625408,1.73068847238236));
#39559=CARTESIAN_POINT('Ctrl Pts',(0.857934783429182,3.35894617427322,1.88802378805348));
#39560=CARTESIAN_POINT('Ctrl Pts',(-2.33375619104173,2.56362702459287,2.0453591037246));
#39561=CARTESIAN_POINT('Ctrl Pts',(-3.42454308987515,-0.539540002481048,
2.20269441939573));
#39562=CARTESIAN_POINT('Ctrl Pts',(-1.43246863664446,-3.15699631612275,
2.36002973506685));
#39563=CARTESIAN_POINT('Ctrl Pts',(1.84914966771382,-2.93244645384971,2.51736505073797));
#39564=CARTESIAN_POINT('Ctrl Pts',(3.46611704321809,-0.0680333465830936,
2.6747003664091));
#39565=CARTESIAN_POINT('Ctrl Pts',(1.96279813083206,2.85762464397308,2.83203568208022));
#39566=CARTESIAN_POINT('Ctrl Pts',(-1.30748115679998,3.21077697834334,2.98937099775135));
#39567=CARTESIAN_POINT('Ctrl Pts',(-3.40073292266579,0.673506642233569,
3.14670631342246));
#39568=CARTESIAN_POINT('Ctrl Pts',(-2.43255897891363,-2.47007132234958,
3.3040416290936));
#39569=CARTESIAN_POINT('Ctrl Pts',(0.725465996449509,-3.39002871776042,
3.46137694476471));
#39570=CARTESIAN_POINT('Ctrl Pts',(3.23040816158946,-1.2581966050299,3.61871226043584));
#39571=CARTESIAN_POINT('Ctrl Pts',(2.8272552899658,2.00629586672699,3.77604757610696));
#39572=CARTESIAN_POINT('Ctrl Pts',(-0.12106421383218,3.46467012121918,3.93338289177809));
#39573=CARTESIAN_POINT('Ctrl Pts',(-2.96039865494578,1.80406080581246,4.09071820744921));
#39574=CARTESIAN_POINT('Ctrl Pts',(-3.13470744102623,-1.48060961970634,
4.24805352312033));
#39575=CARTESIAN_POINT('Ctrl Pts',(-0.48707340020318,-3.43239786321147,
4.40538883879146));
#39576=CARTESIAN_POINT('Ctrl Pts',(2.59903642002639,-2.29425484091306,4.56272415446258));
#39577=CARTESIAN_POINT('Ctrl Pts',(3.3454279982163,0.909234346278705,4.7200594701337));
#39578=CARTESIAN_POINT('Ctrl Pts',(1.0801807804971,3.29420780604002,4.87739478580482));
#39579=CARTESIAN_POINT('Ctrl Pts',(-2.15747246329023,2.71365218072187,5.03473010147595));
#39580=CARTESIAN_POINT('Ctrl Pts',(-3.45291449370647,-0.309801689732533,
5.19206541714708));
#39581=CARTESIAN_POINT('Ctrl Pts',(-1.63995566962662,-3.05436425291692,
5.34940073281819));
#39582=CARTESIAN_POINT('Ctrl Pts',(1.64933267669075,-3.04931095649762,5.50673604848933));
#39583=CARTESIAN_POINT('Ctrl Pts',(3.45385008213154,-0.299190905578683,
5.66407136416044));
#39584=CARTESIAN_POINT('Ctrl Pts',(2.14912439273668,2.7202683566825,5.82140667983157));
#39585=CARTESIAN_POINT('Ctrl Pts',(-1.0902973660189,3.2908733250419,5.97874199550268));
#39586=CARTESIAN_POINT('Ctrl Pts',(-3.34820589287437,0.898950992404627,
6.13607731117382));
#39587=CARTESIAN_POINT('Ctrl Pts',(-2.59197489283764,-2.30222973282867,
6.29341262684493));
#39588=CARTESIAN_POINT('Ctrl Pts',(0.497617384004899,-3.43088509381362,
6.45074794251607));
#39589=CARTESIAN_POINT('Ctrl Pts',(3.13924192099666,-1.47097102258828,6.60808325818718));
#39590=CARTESIAN_POINT('Ctrl Pts',(2.95484157740695,1.81314832273494,6.76541857385831));
#39591=CARTESIAN_POINT('Ctrl Pts',(0.110418200862072,3.46502574430704,6.92275388952943));
#39592=CARTESIAN_POINT('Ctrl Pts',(-2.8334064294993,1.9975994576497,7.08008920520056));
#39593=CARTESIAN_POINT('Ctrl Pts',(-3.22652701467874,-1.26811632402185,
7.23742452087168));
#39594=CARTESIAN_POINT('Ctrl Pts',(-0.715046473049532,-3.39224175569136,
7.3947598365428));
#39595=CARTESIAN_POINT('Ctrl Pts',(2.44013696723805,-2.46258546444229,7.55209515221393));
#39596=CARTESIAN_POINT('Ctrl Pts',(3.39864746673821,0.683952471759619,7.70943046788505));
#39597=CARTESIAN_POINT('Ctrl Pts',(1.29760966092091,3.21477911452065,7.86676578355617));
#39598=CARTESIAN_POINT('Ctrl Pts',(-1.97156914295567,2.85158038765959,8.0241010992273));
#39599=CARTESIAN_POINT('Ctrl Pts',(-3.4658915964548,-0.0786830420698247,
8.18143641489842));
#39600=CARTESIAN_POINT('Ctrl Pts',(-1.84013088404779,-2.93811400679859,
8.33877173056954));
#39601=CARTESIAN_POINT('Ctrl Pts',(1.44216214367922,-3.1525805256303,8.49610704624066));
#39602=CARTESIAN_POINT('Ctrl Pts',(3.42618436209615,-0.529014404638419,
8.6534423619118));
#39603=CARTESIAN_POINT('Ctrl Pts',(2.32586889591107,2.57078382744821,8.81077767758291));
#39604=CARTESIAN_POINT('Ctrl Pts',(-0.868252563983666,3.35629755313536,
8.96811299325404));
#39605=CARTESIAN_POINT('Ctrl Pts',(-3.28075102175166,1.12038736226158,9.12544830892515));
#39606=CARTESIAN_POINT('Ctrl Pts',(-2.73983474254873,-2.12412369627032,
9.28278362459629));
#39607=CARTESIAN_POINT('Ctrl Pts',(0.267550388642249,-3.45644520972622,
9.44011894026741));
#39608=CARTESIAN_POINT('Ctrl Pts',(3.03407913010768,-1.67718692077769,9.59745425593853));
#39609=CARTESIAN_POINT('Ctrl Pts',(3.06925466623264,1.61191643161116,9.75478957160966));
#39610=CARTESIAN_POINT('Ctrl Pts',(0.341406797653059,3.4499337499385,9.91212488728077));
#39611=CARTESIAN_POINT('Ctrl Pts',(-2.69377870488891,2.18223000239878,10.0694602029519));
#39612=CARTESIAN_POINT('Ctrl Pts',(-3.30396687303986,-1.04996552859114,
10.226795518623));
#39613=CARTESIAN_POINT('Ctrl Pts',(-0.939820892206868,-3.33696855340067,
10.3841308342941));
#39614=CARTESIAN_POINT('Ctrl Pts',(2.2703379196763,-2.61992335659027,10.5414661499653));
#39615=CARTESIAN_POINT('Ctrl Pts',(3.43675322554079,0.455595550491001,10.6988014656364));
#39616=CARTESIAN_POINT('Ctrl Pts',(1.50917870869019,3.12106661837885,10.8561367813075));
#39617=CARTESIAN_POINT('Ctrl Pts',(-1.77673321502363,2.97670108175376,11.0134720969786));
#39618=CARTESIAN_POINT('Ctrl Pts',(-3.46368867729937,0.152965991767152,
11.1708074126498));
#39619=CARTESIAN_POINT('Ctrl Pts',(-2.03158068936315,-2.80910804391069,
11.3281427283209));
#39620=CARTESIAN_POINT('Ctrl Pts',(1.22756217529158,-3.24113439556783,11.485478043992));
#39621=CARTESIAN_POINT('Ctrl Pts',(3.38518042007578,-0.757767502188211,
11.6428133596631));
#39622=CARTESIAN_POINT('Ctrl Pts',(2.48830916787281,2.41253151546626,11.8001486753343));
#39623=CARTESIAN_POINT('Ctrl Pts',(0.407565802433691,3.07068338225952,11.9050388857817));
#39624=CARTESIAN_POINT('Ctrl Pts',(-0.545102916878434,2.89105980740811,
11.9574839910054));
#39625=CARTESIAN_POINT('Ctrl Pts',(-2.93989309841074,-0.00232834448912937,
10.1778238829104));
#39626=CARTESIAN_POINT('Ctrl Pts',(-2.94219554736775,-0.304542880453153,
10.1941477614813));
#39627=CARTESIAN_POINT('Ctrl Pts',(-2.89923296915434,-0.606119063222061,
10.2104716400522));
#39628=CARTESIAN_POINT('Ctrl Pts',(-2.80824451487588,-0.892433444227729,
10.226795518623));
#39629=CARTESIAN_POINT('Ctrl Pts',(-2.5159182127622,-1.81229987019432,10.2792406238467));
#39630=CARTESIAN_POINT('Ctrl Pts',(-1.72786955248453,-2.5746342117975,10.3316857290704));
#39631=CARTESIAN_POINT('Ctrl Pts',(-0.798818753698492,-2.83629384979735,
10.3841308342941));
#39632=CARTESIAN_POINT('Ctrl Pts',(0.130232045087536,-3.0979534877972,10.4365759395179));
#39633=CARTESIAN_POINT('Ctrl Pts',(1.20028498238192,-2.85893842219374,10.4890210447416));
#39634=CARTESIAN_POINT('Ctrl Pts',(1.92971400200653,-2.22684440487846,10.5414661499653));
#39635=CARTESIAN_POINT('Ctrl Pts',(2.65914302163113,-1.59475038756318,10.593911255189));
#39636=CARTESIAN_POINT('Ctrl Pts',(3.04794812358597,-0.569577418536059,
10.6463563604127));
#39637=CARTESIAN_POINT('Ctrl Pts',(2.92108825508827,0.387254243958792,10.6988014656364));
#39638=CARTESIAN_POINT('Ctrl Pts',(2.79422838659058,1.34408590645364,10.7512465708601));
#39639=CARTESIAN_POINT('Ctrl Pts',(2.15170354764038,2.23257626241624,10.8036916760838));
#39640=CARTESIAN_POINT('Ctrl Pts',(1.28278914087964,2.6527605176267,10.8561367813075));
#39641=CARTESIAN_POINT('Ctrl Pts',(0.413874734118906,3.07294477283715,10.9085818865312));
#39642=CARTESIAN_POINT('Ctrl Pts',(-0.681429240452357,3.02482292729546,
10.9610269917549));
#39643=CARTESIAN_POINT('Ctrl Pts',(-1.51024047145062,2.53013948952684,11.0134720969786));
#39644=CARTESIAN_POINT('Ctrl Pts',(-1.74480463118476,2.39013776105746,11.0283147313191));
#39645=CARTESIAN_POINT('Ctrl Pts',(-1.95802372783935,2.21436813426865,11.0431573656595));
#39646=CARTESIAN_POINT('Ctrl Pts',(-2.14415473270596,2.01243073062332,11.058));
#39647=CARTESIAN_POINT('Ctrl Pts',(-1.37989654081095,-1.933266887693,1.56125112837913E-17));
#39648=CARTESIAN_POINT('Ctrl Pts',(-1.44414345926609,-1.89839188587405,
5.80920822621902E-18));
#39649=CARTESIAN_POINT('Ctrl Pts',(-1.5065284577229,-1.86047032724736,-1.41833741640826E-16));
#39650=CARTESIAN_POINT('Ctrl Pts',(-1.56680444439783,-1.81955553349441,
-1.49186218934005E-16));
#39651=CARTESIAN_POINT('Ctrl Pts',(-1.63448180748404,-1.77361675247786,
-1.62745475426733E-16));
#39652=CARTESIAN_POINT('Ctrl Pts',(-1.69950176926845,-1.72390575990714,
4.47554715783556E-16));
#39653=CARTESIAN_POINT('Ctrl Pts',(-1.76178079551988,-1.6707784873017,5.27355936696949E-16));
#39654=CARTESIAN_POINT('Ctrl Pts',(-1.80277525259689,-1.63580806744237,
5.79884178102324E-16));
#39655=CARTESIAN_POINT('Ctrl Pts',(-1.84258178887229,-1.59935636303953,
9.13682232518509E-17));
#39656=CARTESIAN_POINT('Ctrl Pts',(-1.88117141744704,-1.56151405921777,
1.59594559789866E-16));
#39657=CARTESIAN_POINT('Ctrl Pts',(-1.89157558896771,-1.55131137434519,
1.77989100856589E-16));
#39658=CARTESIAN_POINT('Ctrl Pts',(-1.90188938652621,-1.54100934347453,
3.40635361961997E-16));
#39659=CARTESIAN_POINT('Ctrl Pts',(-1.91210630257196,-1.53061605927472,
3.05311331771918E-16));
#39660=CARTESIAN_POINT('Ctrl Pts',(-1.9724409846318,-1.46923985779222,9.67098202152561E-17));
#39661=CARTESIAN_POINT('Ctrl Pts',(-2.02946085491381,-1.40462521591101,
1.4935214824922E-16));
#39662=CARTESIAN_POINT('Ctrl Pts',(-2.08307562783518,-1.33717477526203,
1.38777878078145E-16));
#39663=CARTESIAN_POINT('Ctrl Pts',(-2.12998855414138,-1.27815563969417,
1.29525391678454E-16));
#39664=CARTESIAN_POINT('Ctrl Pts',(-2.17429437900105,-1.21696417926775,
2.01441503266146E-16));
#39665=CARTESIAN_POINT('Ctrl Pts',(-2.21591583956505,-1.15384057343859,
1.52655665885959E-16));
#39666=CARTESIAN_POINT('Ctrl Pts',(-2.23664963326987,-1.12239545345888,
1.28352927004359E-16));
#39667=CARTESIAN_POINT('Ctrl Pts',(-2.25671701785544,-1.09047047206691,
-2.37280165770185E-16));
#39668=CARTESIAN_POINT('Ctrl Pts',(-2.2761066605572,-1.05809323638609,-2.63677968348475E-16));
#39669=CARTESIAN_POINT('Ctrl Pts',(-2.28578146762193,-1.0419380388242,-2.76849621421526E-16));
#39670=CARTESIAN_POINT('Ctrl Pts',(-2.29528887628369,-1.02566760843717,
-1.10809144900277E-17));
#39671=CARTESIAN_POINT('Ctrl Pts',(-2.30461525834334,-1.0093071858719,0.));
#39672=CARTESIAN_POINT('Ctrl Pts',(-2.34846766322256,-0.932380906234359,
5.21021705459412E-17));
#39673=CARTESIAN_POINT('Ctrl Pts',(-2.38837887518559,-0.853373340579809,
-1.59588577561705E-17));
#39674=CARTESIAN_POINT('Ctrl Pts',(-2.42425706703596,-0.772682188207588,
-2.77555756156289E-17));
#39675=CARTESIAN_POINT('Ctrl Pts',(-2.46075963346513,-0.690586798283878,
-3.97575872863117E-17));
#39676=CARTESIAN_POINT('Ctrl Pts',(-2.49308822244858,-0.606748001409621,
2.24945356107799E-18));
#39677=CARTESIAN_POINT('Ctrl Pts',(-2.52111243497218,-0.521542915861604,
-2.77555756156289E-17));
#39678=CARTESIAN_POINT('Ctrl Pts',(-2.54406484395513,-0.4517581906252,-5.23303143573299E-17));
#39679=CARTESIAN_POINT('Ctrl Pts',(-2.56412941494483,-0.381055975787894,
-5.2234519399031E-17));
#39680=CARTESIAN_POINT('Ctrl Pts',(-2.58121358727312,-0.309628512371508,
-5.55111512312578E-17));
#39681=CARTESIAN_POINT('Ctrl Pts',(-2.59402671651933,-0.256057914809218,
-5.79686251054279E-17));
#39682=CARTESIAN_POINT('Ctrl Pts',(-2.6051630020304,-0.202079063721199,
-1.68485553630616E-16));
#39683=CARTESIAN_POINT('Ctrl Pts',(-2.61457527537642,-0.147769877191515,
-1.94289029309402E-16));
#39684=CARTESIAN_POINT('Ctrl Pts',(-2.617136534184,-0.132991313371873,-2.01310646395843E-16));
#39685=CARTESIAN_POINT('Ctrl Pts',(-2.6195700893165,-0.118188277474481,
-3.31395093795537E-16));
#39686=CARTESIAN_POINT('Ctrl Pts',(-2.6218748923051,-0.103362317982878,
-3.33066907387547E-16));
#39687=CARTESIAN_POINT('Ctrl Pts',(-2.62397146608191,-0.089875821288789,
-3.34587679685255E-16));
#39688=CARTESIAN_POINT('Ctrl Pts',(-2.62596008221826,-0.076379405564125,
-2.78772373994456E-16));
#39689=CARTESIAN_POINT('Ctrl Pts',(-2.62784009463941,-0.0628763941457686,
-2.77555756156289E-16));
#39690=CARTESIAN_POINT('Ctrl Pts',(-2.64060982150785,0.0288409614284714,
-2.69292046128659E-16));
#39691=CARTESIAN_POINT('Ctrl Pts',(-2.64837710873961,0.12089024959815,-1.76997536955934E-16));
#39692=CARTESIAN_POINT('Ctrl Pts',(-2.65101366112809,0.212875307143708,
-1.38777878078145E-16));
#39693=CARTESIAN_POINT('Ctrl Pts',(-2.65226659852151,0.256588270610049,
-1.20615204739669E-16));
#39694=CARTESIAN_POINT('Ctrl Pts',(-2.65236023741492,0.300287183221066,
-4.34987190636111E-16));
#39695=CARTESIAN_POINT('Ctrl Pts',(-2.6512772014093,0.343931535522003,-4.16333634234434E-16));
#39696=CARTESIAN_POINT('Ctrl Pts',(-2.64907421925761,0.432707650667494,
-4.32903459206313E-16));
#39697=CARTESIAN_POINT('Ctrl Pts',(-2.64200629387468,0.521257644934972,
-8.62622134822235E-17));
#39698=CARTESIAN_POINT('Ctrl Pts',(-2.63031624428264,0.609320814221094,
-8.32667268468867E-17));
#39699=CARTESIAN_POINT('Ctrl Pts',(-2.61839797794639,0.699103179787949,
-8.02127613999854E-17));
#39700=CARTESIAN_POINT('Ctrl Pts',(-2.60167524897612,0.788380265268053,
1.49019320792917E-16));
#39701=CARTESIAN_POINT('Ctrl Pts',(-2.58035146554209,0.876878238745711,
2.4980018054066E-16));
#39702=CARTESIAN_POINT('Ctrl Pts',(-2.57698234718955,0.890860754912604,
2.65723370025807E-16));
#39703=CARTESIAN_POINT('Ctrl Pts',(-2.57349826551832,0.904823813068977,
1.71128026421916E-16));
#39704=CARTESIAN_POINT('Ctrl Pts',(-2.56989990586492,0.918766319054272,
1.94289029309402E-16));
#39705=CARTESIAN_POINT('Ctrl Pts',(-2.56629916621592,0.932718046770052,
2.17465351145046E-16));
#39706=CARTESIAN_POINT('Ctrl Pts',(-2.56258611805641,0.946640891227604,
-7.03868084514403E-16));
#39707=CARTESIAN_POINT('Ctrl Pts',(-2.55876298044222,0.960529869852388,
-6.93889390390723E-16));
#39708=CARTESIAN_POINT('Ctrl Pts',(-2.53419843880054,1.04976976342104,-6.29773977327716E-16));
#39709=CARTESIAN_POINT('Ctrl Pts',(-2.50508011125346,1.13766264916498,6.87890529294335E-17));
#39710=CARTESIAN_POINT('Ctrl Pts',(-2.47169823504828,1.22392740477737,8.32667268468867E-17));
#39711=CARTESIAN_POINT('Ctrl Pts',(-2.43767482619284,1.31184999582573,9.80226325947151E-17));
#39712=CARTESIAN_POINT('Ctrl Pts',(-2.39922225163329,1.39808205966622,-2.50151931196036E-16));
#39713=CARTESIAN_POINT('Ctrl Pts',(-2.35659236008881,1.48232869936419,-2.77555756156289E-16));
#39714=CARTESIAN_POINT('Ctrl Pts',(-2.31360056696885,1.56729054124849,-3.05192222745878E-16));
#39715=CARTESIAN_POINT('Ctrl Pts',(-2.26635993703635,1.65023397727082,5.65740922539343E-17));
#39716=CARTESIAN_POINT('Ctrl Pts',(-2.21507658716517,1.73084671943837,5.55111512312578E-17));
#39717=CARTESIAN_POINT('Ctrl Pts',(-2.18435464293681,1.77913880985734,5.48743828668913E-17));
#39718=CARTESIAN_POINT('Ctrl Pts',(-2.15218088295609,1.82659422289983,-3.64380860772878E-16));
#39719=CARTESIAN_POINT('Ctrl Pts',(-2.11859145320912,1.87314213253736,-3.88578058618805E-16));
#39720=CARTESIAN_POINT('Ctrl Pts',(-2.10923966749503,1.88610174750099,-3.95314910385597E-16));
#39721=CARTESIAN_POINT('Ctrl Pts',(-2.09977706809611,1.89899226435558,-9.16981750261902E-17));
#39722=CARTESIAN_POINT('Ctrl Pts',(-2.0902160744712,1.91179680016256,-1.11022302462516E-16));
#39723=CARTESIAN_POINT('Ctrl Pts',(-2.03140899114824,1.99055403331781,-2.29879778669894E-16));
#39724=CARTESIAN_POINT('Ctrl Pts',(-1.96879105165951,2.06618994280669,4.68887291460301E-17));
#39725=CARTESIAN_POINT('Ctrl Pts',(-1.90263522085423,2.13839704217079,0.));
#39726=CARTESIAN_POINT('Ctrl Pts',(-1.83630675569242,2.21079256674222,-4.70110857922477E-17));
#39727=CARTESIAN_POINT('Ctrl Pts',(-1.76642150904269,2.27974226115238,-1.93865480317173E-16));
#39728=CARTESIAN_POINT('Ctrl Pts',(-1.6932045763485,2.34492041918897,-1.66533453693773E-16));
#39729=CARTESIAN_POINT('Ctrl Pts',(-1.62138195170811,2.40885735573024,-1.39721925040515E-16));
#39730=CARTESIAN_POINT('Ctrl Pts',(-1.54635279514513,2.46916580377976,-2.38947154895597E-16));
#39731=CARTESIAN_POINT('Ctrl Pts',(-1.46828869930752,2.52551090354043,-2.77555756156289E-16));
#39732=CARTESIAN_POINT('Ctrl Pts',(-1.41016377964657,2.56746430557163,-3.06302926317174E-16));
#39733=CARTESIAN_POINT('Ctrl Pts',(-1.35035542782446,2.60721994910279,8.78385754915914E-18));
#39734=CARTESIAN_POINT('Ctrl Pts',(-1.28892185405322,2.64462557919718,0.));
#39735=CARTESIAN_POINT('Origin',(0.,0.,0.));
#39736=CARTESIAN_POINT('Origin',(-1.44337567297407,-2.5,-6.));
#39737=CARTESIAN_POINT('',(-1.44337567297407,-2.5,-6.));
#39738=CARTESIAN_POINT('',(1.44337567297406,-2.5,-6.));
#39739=CARTESIAN_POINT('',(-0.721687836487033,-2.5,-6.));
#39740=CARTESIAN_POINT('',(-1.44337567297407,-2.5,-3.));
#39741=CARTESIAN_POINT('',(-1.44337567297407,-2.5,-6.));
#39742=CARTESIAN_POINT('',(1.44337567297406,-2.5,-3.));
#39743=CARTESIAN_POINT('',(-1.44337567297407,-2.5,-3.));
#39744=CARTESIAN_POINT('',(1.44337567297406,-2.5,-6.));
#39745=CARTESIAN_POINT('Origin',(-2.88675134594813,3.53525079574969E-16,
-6.));
#39746=CARTESIAN_POINT('',(-2.88675134594813,3.53525079574969E-16,-6.));
#39747=CARTESIAN_POINT('',(-2.52590742770461,-0.625,-6.));
#39748=CARTESIAN_POINT('',(-2.88675134594813,5.55111512312578E-16,-3.));
#39749=CARTESIAN_POINT('',(-2.88675134594813,3.53525079574969E-16,-6.));
#39750=CARTESIAN_POINT('',(-2.88675134594813,3.53525079574969E-16,-3.));
#39751=CARTESIAN_POINT('Origin',(-1.44337567297406,2.5,-6.));
#39752=CARTESIAN_POINT('',(-1.44337567297406,2.5,-6.));
#39753=CARTESIAN_POINT('',(-1.80421959121758,1.875,-6.));
#39754=CARTESIAN_POINT('',(-1.44337567297406,2.5,-3.));
#39755=CARTESIAN_POINT('',(-1.44337567297406,2.5,-6.));
#39756=CARTESIAN_POINT('',(-1.44337567297406,2.5,-3.));
#39757=CARTESIAN_POINT('Origin',(1.44337567297406,2.5,-6.));
#39758=CARTESIAN_POINT('',(1.44337567297406,2.5,-6.));
#39759=CARTESIAN_POINT('',(0.721687836487033,2.5,-6.));
#39760=CARTESIAN_POINT('',(1.44337567297406,2.5,-3.));
#39761=CARTESIAN_POINT('',(1.44337567297406,2.5,-6.));
#39762=CARTESIAN_POINT('',(1.44337567297406,2.5,-3.));
#39763=CARTESIAN_POINT('Origin',(2.88675134594813,0.,-6.));
#39764=CARTESIAN_POINT('',(2.88675134594813,0.,-6.));
#39765=CARTESIAN_POINT('',(2.52590742770461,0.625,-6.));
#39766=CARTESIAN_POINT('',(2.88675134594813,0.,-3.));
#39767=CARTESIAN_POINT('',(2.88675134594813,0.,-6.));
#39768=CARTESIAN_POINT('',(2.88675134594813,0.,-3.));
#39769=CARTESIAN_POINT('Origin',(1.44337567297406,-2.5,-6.));
#39770=CARTESIAN_POINT('',(1.80421959121758,-1.875,-6.));
#39771=CARTESIAN_POINT('',(1.44337567297406,-2.5,-3.));
#39772=CARTESIAN_POINT('Origin',(0.,0.,-3.));
#39773=CARTESIAN_POINT('Origin',(0.,0.,0.));
#39774=CARTESIAN_POINT('',(-5.,-6.12323399573677E-16,0.));
#39775=CARTESIAN_POINT('Origin',(0.,0.,0.));
#39776=CARTESIAN_POINT('Origin',(0.,0.,-6.));
#39777=CARTESIAN_POINT('',(-5.,-6.12323399573677E-16,-6.));
#39778=CARTESIAN_POINT('',(-5.,-6.12323399573677E-16,-6.));
#39779=CARTESIAN_POINT('Origin',(0.,0.,-6.));
#39780=CARTESIAN_POINT('Origin',(0.,0.,-6.));
#39781=CARTESIAN_POINT('Origin',(0.,0.,12.));
#39782=CARTESIAN_POINT('',(0.,0.,0.));
#39783=CARTESIAN_POINT('Origin',(0.,0.,0.));
#39784=CARTESIAN_POINT('',(-7.92502372531584,0.000203888857960161,0.482686825365204));
#39785=CARTESIAN_POINT('',(-7.92493078473506,0.000130763509288048,0.267313174634791));
#39786=CARTESIAN_POINT('',(-7.925,-9.70532588324277E-16,0.));
#39787=CARTESIAN_POINT('',(3.45478907940189,7.13232482552817,0.));
#39788=CARTESIAN_POINT('Ctrl Pts',(-7.92502372531584,0.000203888857960161,
0.482686825365204));
#39789=CARTESIAN_POINT('Ctrl Pts',(-7.92532623227895,0.295954310302644,
0.473777398238157));
#39790=CARTESIAN_POINT('Ctrl Pts',(-7.90908776172729,0.591671595388266,
0.46486797111111));
#39791=CARTESIAN_POINT('Ctrl Pts',(-7.87605276584388,0.88550030186303,0.455958543984063));
#39792=CARTESIAN_POINT('Ctrl Pts',(-7.72921199846845,2.19157077597367,0.416356083586355));
#39793=CARTESIAN_POINT('Ctrl Pts',(-7.25050411141088,3.46032655960519,0.376753623188647));
#39794=CARTESIAN_POINT('Ctrl Pts',(-6.49799558141544,4.53787932192357,0.33715116279094));
#39795=CARTESIAN_POINT('Ctrl Pts',(-5.74548705142,5.61543208424195,0.297548702393232));
#39796=CARTESIAN_POINT('Ctrl Pts',(-4.7191778784867,6.50178182524719,0.257946241995526));
#39797=CARTESIAN_POINT('Ctrl Pts',(-3.54355620222258,7.0893994069169,0.218343781597818));
#39798=CARTESIAN_POINT('Ctrl Pts',(-2.36793452595845,7.67701698858661,0.178741321200111));
#39799=CARTESIAN_POINT('Ctrl Pts',(-1.04300034636349,7.96590241092079,0.139138860802403));
#39800=CARTESIAN_POINT('Ctrl Pts',(0.270533623218387,7.92104793571692,0.0995364004046956));
#39801=CARTESIAN_POINT('Ctrl Pts',(1.37100770006842,7.88346901630132,0.0663576002697969));
#39802=CARTESIAN_POINT('Ctrl Pts',(2.46347993683329,7.61163710618861,0.0331788001348983));
#39803=CARTESIAN_POINT('Ctrl Pts',(3.45507168555157,7.13251860299055,-2.84060969191202E-16));
#39804=CARTESIAN_POINT('',(-3.45478907940191,7.13232482552816,0.));
#39805=CARTESIAN_POINT('Origin',(0.,0.,0.));
#39806=CARTESIAN_POINT('Ctrl Pts',(-3.45478907940191,7.13232482552816,6.24500451351651E-16));
#39807=CARTESIAN_POINT('Ctrl Pts',(-4.63794475549662,6.55922230860771,0.0396024603977076));
#39808=CARTESIAN_POINT('Ctrl Pts',(-5.67516414283391,5.6863469211646,0.0792049207954145));
#39809=CARTESIAN_POINT('Ctrl Pts',(-6.44101552295666,4.61843342960788,0.118807381193121));
#39810=CARTESIAN_POINT('Ctrl Pts',(-7.20686690307942,3.55051993805114,0.158409841590829));
#39811=CARTESIAN_POINT('Ctrl Pts',(-7.70135027598763,2.28756834238077,0.198012301988537));
#39812=CARTESIAN_POINT('Ctrl Pts',(-7.86443494073275,0.983361388757709,
0.237614762386245));
#39813=CARTESIAN_POINT('Ctrl Pts',(-7.90520139443602,0.657347336624382,
0.24751423313576));
#39814=CARTESIAN_POINT('Ctrl Pts',(-7.92526021663928,0.328755420640525,
0.257413703885276));
#39815=CARTESIAN_POINT('Ctrl Pts',(-7.92493078473506,0.000130763509288048,
0.267313174634791));
#39816=CARTESIAN_POINT('Origin',(0.,0.,0.));
#39817=CARTESIAN_POINT('',(-7.92532948546385,-0.000170658577658411,1.9826868253652));
#39818=CARTESIAN_POINT('',(-7.92542130335282,-0.000150527452605021,1.76731317463479));
#39819=CARTESIAN_POINT('',(-7.925,-9.70532588324277E-16,0.));
#39820=CARTESIAN_POINT('Ctrl Pts',(-7.92532948546385,-0.000170658577658411,
1.9826868253652));
#39821=CARTESIAN_POINT('Ctrl Pts',(-7.92427024157546,1.11771666749154,1.94900692301065));
#39822=CARTESIAN_POINT('Ctrl Pts',(-7.68542693347382,2.23604223578417,1.91532702065609));
#39823=CARTESIAN_POINT('Ctrl Pts',(-7.22635584668683,3.25516459727708,1.88164711830153));
#39824=CARTESIAN_POINT('Ctrl Pts',(-6.68655782878211,4.45349802878656,1.84204465790382));
#39825=CARTESIAN_POINT('Ctrl Pts',(-5.84226858153731,5.5146711684689,1.80244219750611));
#39826=CARTESIAN_POINT('Ctrl Pts',(-4.7958983657642,6.30996626240027,1.76283973710841));
#39827=CARTESIAN_POINT('Ctrl Pts',(-3.7495281499911,7.10526135633162,1.7232372767107));
#39828=CARTESIAN_POINT('Ctrl Pts',(-2.50107696568969,7.634678404512,1.68363481631299));
#39829=CARTESIAN_POINT('Ctrl Pts',(-1.20197894693782,7.83400038341452,1.64403235591528));
#39830=CARTESIAN_POINT('Ctrl Pts',(0.0971190718140523,8.03332236231703,
1.60442989551758));
#39831=CARTESIAN_POINT('Ctrl Pts',(1.4468639250164,7.90254927194168,1.56482743511987));
#39832=CARTESIAN_POINT('Ctrl Pts',(2.68353479884886,7.4575435850056,1.52522497472216));
#39833=CARTESIAN_POINT('Ctrl Pts',(3.92020567268132,7.01253789806953,1.48562251432445));
#39834=CARTESIAN_POINT('Ctrl Pts',(5.04380256714389,6.25329961457273,1.44602005392675));
#39835=CARTESIAN_POINT('Ctrl Pts',(5.91803587468444,5.27192249672745,1.40641759352904));
#39836=CARTESIAN_POINT('Ctrl Pts',(6.79226918222501,4.29054537888217,1.36681513313133));
#39837=CARTESIAN_POINT('Ctrl Pts',(7.41713890284356,3.08702942668839,1.32721267273363));
#39838=CARTESIAN_POINT('Ctrl Pts',(7.71684983649437,1.8073582788516,1.28761021233592));
#39839=CARTESIAN_POINT('Ctrl Pts',(8.01656077014517,0.527687131014814,1.24800775193821));
#39840=CARTESIAN_POINT('Ctrl Pts',(7.99111291682824,-0.828139212464995,
1.2084052915405));
#39841=CARTESIAN_POINT('Ctrl Pts',(7.64359304336192,-2.09566234689561,1.1688028311428));
#39842=CARTESIAN_POINT('Ctrl Pts',(7.29607316989561,-3.36318548132621,1.12920037074509));
#39843=CARTESIAN_POINT('Ctrl Pts',(6.62648127627991,-4.54240540670763,1.08959791034738));
#39844=CARTESIAN_POINT('Ctrl Pts',(5.71603724686592,-5.49028541995301,1.04999544994967));
#39845=CARTESIAN_POINT('Ctrl Pts',(4.80559321745193,-6.4381654331984,1.01039298955197));
#39846=CARTESIAN_POINT('Ctrl Pts',(3.65429705223965,-7.15470553430775,0.970790529154259));
#39847=CARTESIAN_POINT('Ctrl Pts',(2.40179822718111,-7.55299143001374,0.931188068756552));
#39848=CARTESIAN_POINT('Ctrl Pts',(1.14929940212257,-7.95127732571973,0.891585608358844));
#39849=CARTESIAN_POINT('Ctrl Pts',(-0.204402082782219,-8.03130901602234,
0.851983147961137));
#39850=CARTESIAN_POINT('Ctrl Pts',(-1.49510550858021,-7.78337825673035,
0.81238068756343));
#39851=CARTESIAN_POINT('Ctrl Pts',(-2.78580893437819,-7.53544749743836,
0.772778227165722));
#39852=CARTESIAN_POINT('Ctrl Pts',(-4.01351430106938,-6.95955428855176,
0.733175766768014));
#39853=CARTESIAN_POINT('Ctrl Pts',(-5.02930384455586,-6.12555425440213,
0.693573306370307));
#39854=CARTESIAN_POINT('Ctrl Pts',(-6.04509338804233,-5.29155422025249,
0.6539708459726));
#39855=CARTESIAN_POINT('Ctrl Pts',(-6.84896710832411,-4.19944736083982,
0.614368385574893));
#39856=CARTESIAN_POINT('Ctrl Pts',(-7.34341714461835,-2.98170134883861,
0.574765925177185));
#39857=CARTESIAN_POINT('Ctrl Pts',(-7.72662998700875,-2.03791355166095,
0.544072891906525));
#39858=CARTESIAN_POINT('Ctrl Pts',(-7.92398158689877,-1.01865819910462,
0.513379858635864));
#39859=CARTESIAN_POINT('Ctrl Pts',(-7.92502372531584,0.000203888857960161,
0.482686825365204));
#39860=CARTESIAN_POINT('Ctrl Pts',(-7.92493078473506,0.000130763509288048,
0.267313174634791));
#39861=CARTESIAN_POINT('Ctrl Pts',(-7.92394233669697,-0.985895160087429,
0.297016164282983));
#39862=CARTESIAN_POINT('Ctrl Pts',(-7.73940303358924,-1.97221584485231,
0.326719153931175));
#39863=CARTESIAN_POINT('Ctrl Pts',(-7.37994005288748,-2.89008119835739,
0.356422143579367));
#39864=CARTESIAN_POINT('Ctrl Pts',(-6.90067454371506,-4.11385452027366,
0.396024603977074));
#39865=CARTESIAN_POINT('Ctrl Pts',(-6.11045756878819,-5.21593885253046,
0.435627064374781));
#39866=CARTESIAN_POINT('Ctrl Pts',(-5.10512425767101,-6.06252668852639,
0.475229524772489));
#39867=CARTESIAN_POINT('Ctrl Pts',(-4.09979094655382,-6.90911452452231,
0.514831985170196));
#39868=CARTESIAN_POINT('Ctrl Pts',(-2.87934129924631,-7.50020586425735,
0.554434445567904));
#39869=CARTESIAN_POINT('Ctrl Pts',(-1.59182128379852,-7.7641673765801,0.594036905965611));
#39870=CARTESIAN_POINT('Ctrl Pts',(-0.304301268350717,-8.02812888890286,
0.633639366363318));
#39871=CARTESIAN_POINT('Ctrl Pts',(1.05028911523738,-7.96496057381331,0.673241826761026));
#39872=CARTESIAN_POINT('Ctrl Pts',(2.30764556912295,-7.5822916411342,0.712844287158734));
#39873=CARTESIAN_POINT('Ctrl Pts',(3.56500202300852,-7.1996227084551,0.752446747556441));
#39874=CARTESIAN_POINT('Ctrl Pts',(4.72512454719156,-6.49745315818644,0.792049207954148));
#39875=CARTESIAN_POINT('Ctrl Pts',(5.64729088391455,-5.56097129020032,0.831651668351856));
#39876=CARTESIAN_POINT('Ctrl Pts',(6.56945722063754,-4.6244894222142,0.871254128749563));
#39877=CARTESIAN_POINT('Ctrl Pts',(7.25366736990048,-3.45369523651063,0.910856589147271));
#39878=CARTESIAN_POINT('Ctrl Pts',(7.61692939337572,-2.19059467623739,0.950459049544978));
#39879=CARTESIAN_POINT('Ctrl Pts',(7.98019141685096,-0.927494115964165,
0.990061509942686));
#39880=CARTESIAN_POINT('Ctrl Pts',(8.0225053145385,0.427912818878729,1.02966397034039));
#39881=CARTESIAN_POINT('Ctrl Pts',(7.73873794470293,1.71121413696055,1.0692664307381));
#39882=CARTESIAN_POINT('Ctrl Pts',(7.45497057486737,2.99451545504238,1.10886889113581));
#39883=CARTESIAN_POINT('Ctrl Pts',(6.8451219375087,4.20571115636314,1.14847135153352));
#39884=CARTESIAN_POINT('Ctrl Pts',(5.98316549926359,5.19788834344375,1.18807381193122));
#39885=CARTESIAN_POINT('Ctrl Pts',(5.12120906101848,6.19006553052436,1.22767627232893));
#39886=CARTESIAN_POINT('Ctrl Pts',(4.00714482188693,6.9632242033648,1.26727873272664));
#39887=CARTESIAN_POINT('Ctrl Pts',(2.77610595421604,7.42358092802782,1.30688119312434));
#39888=CARTESIAN_POINT('Ctrl Pts',(1.54506708654514,7.88393765269083,1.34648365352205));
#39889=CARTESIAN_POINT('Ctrl Pts',(0.197053590334899,8.03149242917641,1.38608611391976));
#39890=CARTESIAN_POINT('Ctrl Pts',(-1.10442365502742,7.84834779953031,1.42568857431747));
#39891=CARTESIAN_POINT('Ctrl Pts',(-2.40590090038974,7.66520316988421,1.46529103471517));
#39892=CARTESIAN_POINT('Ctrl Pts',(-3.66084189490413,7.15135913410644,1.50489349511288));
#39893=CARTESIAN_POINT('Ctrl Pts',(-4.71702534436858,6.36914344397809,1.54449595551059));
#39894=CARTESIAN_POINT('Ctrl Pts',(-5.77320879383302,5.58692775384975,1.5840984159083));
#39895=CARTESIAN_POINT('Ctrl Pts',(-6.63063469824751,4.53634040937083,1.62370087630601));
#39896=CARTESIAN_POINT('Ctrl Pts',(-7.18529933225044,3.34481528739395,1.66330333670371));
#39897=CARTESIAN_POINT('Ctrl Pts',(-7.67088009423164,2.30169546114194,1.69797328268074));
#39898=CARTESIAN_POINT('Ctrl Pts',(-7.92442114724993,1.15055930628868,1.73264322865776));
#39899=CARTESIAN_POINT('Ctrl Pts',(-7.92542130335282,-0.000150527452605021,
1.76731317463479));
#39900=CARTESIAN_POINT('Origin',(0.,0.,0.));
#39901=CARTESIAN_POINT('',(-7.92433472984446,2.91513625877426E-5,3.4826868253652));
#39902=CARTESIAN_POINT('',(-7.92432847716457,-1.12691906257078E-6,3.26731317463479));
#39903=CARTESIAN_POINT('',(-7.925,-9.70532588324277E-16,0.));
#39904=CARTESIAN_POINT('Ctrl Pts',(-7.92433472984446,2.91513625877426E-5,
3.4826868253652));
#39905=CARTESIAN_POINT('Ctrl Pts',(-7.92441529464847,0.625845985284648,
3.46383890818084));
#39906=CARTESIAN_POINT('Ctrl Pts',(-7.8511761824248,1.25164427548606,3.44499099099648));
#39907=CARTESIAN_POINT('Ctrl Pts',(-7.70440497514907,1.85969334967445,3.42614307381212));
#39908=CARTESIAN_POINT('Ctrl Pts',(-7.39601541322528,3.13730079801299,3.38654061341441));
#39909=CARTESIAN_POINT('Ctrl Pts',(-6.76299144473731,4.33654782151547,3.34693815301671));
#39910=CARTESIAN_POINT('Ctrl Pts',(-5.8821173587817,5.31196863257356,3.307335692619));
#39911=CARTESIAN_POINT('Ctrl Pts',(-5.00124327282608,6.28738944363165,3.26773323222129));
#39912=CARTESIAN_POINT('Ctrl Pts',(-3.87251906940282,7.03898404224534,3.22813077182358));
#39913=CARTESIAN_POINT('Ctrl Pts',(-2.63285628719021,7.47558580627131,3.18852831142588));
#39914=CARTESIAN_POINT('Ctrl Pts',(-1.3931935049776,7.91218757029729,3.14892585102817));
#39915=CARTESIAN_POINT('Ctrl Pts',(-0.0425921439756402,8.03379649973554,
3.10932339063046));
#39916=CARTESIAN_POINT('Ctrl Pts',(1.25512309008608,7.82566172311737,3.06972093023275));
#39917=CARTESIAN_POINT('Ctrl Pts',(2.5528383241478,7.6175269464992,3.03011846983505));
#39918=CARTESIAN_POINT('Ctrl Pts',(3.79766743126929,7.0796484638246,2.99051600943734));
#39919=CARTESIAN_POINT('Ctrl Pts',(4.8386156264262,6.27726964496666,2.95091354903963));
#39920=CARTESIAN_POINT('Ctrl Pts',(5.87956382158311,5.47489082610872,2.91131108864192));
#39921=CARTESIAN_POINT('Ctrl Pts',(6.71663110477544,4.40801167106745,2.87170862824421));
#39922=CARTESIAN_POINT('Ctrl Pts',(7.2482832222225,3.20604206247861,2.83210616784651));
#39923=CARTESIAN_POINT('Ctrl Pts',(7.77993533966956,2.00407245388978,2.7925037074488));
#39924=CARTESIAN_POINT('Ctrl Pts',(8.00617229137134,0.667012391753384,2.7529012470511));
#39925=CARTESIAN_POINT('Ctrl Pts',(7.8995520777056,-0.642955945262401,2.71329878665339));
#39926=CARTESIAN_POINT('Ctrl Pts',(7.79293186403986,-1.9529242822782,2.67369632625568));
#39927=CARTESIAN_POINT('Ctrl Pts',(7.35345448500659,-3.23580089417338,2.63409386585797));
#39928=CARTESIAN_POINT('Ctrl Pts',(6.63442749261576,-4.33597592487487,2.59449140546026));
#39929=CARTESIAN_POINT('Ctrl Pts',(5.91540050022493,-5.43615095557636,2.55488894506255));
#39930=CARTESIAN_POINT('Ctrl Pts',(4.91682389447654,-6.35362440508415,2.51528648466485));
#39931=CARTESIAN_POINT('Ctrl Pts',(3.75982262260237,-6.97710894444533,2.47568402426714));
#39932=CARTESIAN_POINT('Ctrl Pts',(2.60282135072821,-7.60059348380651,2.43608156386943));
#39933=CARTESIAN_POINT('Ctrl Pts',(1.28739541272828,-7.93008911302109,2.39647910347173));
#39934=CARTESIAN_POINT('Ctrl Pts',(-0.0268971801072414,-7.92562880264182,
2.35687664307402));
#39935=CARTESIAN_POINT('Ctrl Pts',(-1.34118977294278,-7.92116849226255,
2.31727418267631));
#39936=CARTESIAN_POINT('Ctrl Pts',(-2.65434902061391,-7.58275224228942,
2.2776717222786));
#39937=CARTESIAN_POINT('Ctrl Pts',(-3.80709185594238,-6.95142913198073,
2.2380692618809));
#39938=CARTESIAN_POINT('Ctrl Pts',(-4.95983469127085,-6.32010602167203,
2.19846680148319));
#39939=CARTESIAN_POINT('Ctrl Pts',(-5.95216111425665,-5.39587605102776,
2.15886434108548));
#39940=CARTESIAN_POINT('Ctrl Pts',(-6.66370430982927,-4.29084609912597,
2.11926188068777));
#39941=CARTESIAN_POINT('Ctrl Pts',(-7.37524750540189,-3.18581614722418,
2.07965942029007));
#39942=CARTESIAN_POINT('Ctrl Pts',(-7.80600747356133,-1.89998621406488,
2.04005695989236));
#39943=CARTESIAN_POINT('Ctrl Pts',(-7.90373406335874,-0.58932438581693,
2.00045449949465));
#39944=CARTESIAN_POINT('Ctrl Pts',(-7.9183490997636,-0.393314575446958,
1.9945319414515));
#39945=CARTESIAN_POINT('Ctrl Pts',(-7.92551575184149,-0.196749392822418,
1.98860938340835));
#39946=CARTESIAN_POINT('Ctrl Pts',(-7.92532948546385,-0.000170658577658411,
1.9826868253652));
#39947=CARTESIAN_POINT('Ctrl Pts',(-7.92542130335282,-0.000150527452605021,
1.76731317463479));
#39948=CARTESIAN_POINT('Ctrl Pts',(-7.92556359617334,-0.163862719352453,
1.77224568905547));
#39949=CARTESIAN_POINT('Ctrl Pts',(-7.92059422714886,-0.327566282117818,
1.77717820347615));
#39950=CARTESIAN_POINT('Ctrl Pts',(-7.91045415923277,-0.490948934636991,
1.78211071789683));
#39951=CARTESIAN_POINT('Ctrl Pts',(-7.82904098862079,-1.80272513521619,
1.82171317829454));
#39952=CARTESIAN_POINT('Ctrl Pts',(-7.41431128380546,-3.09381463689972,
1.86131563869225));
#39953=CARTESIAN_POINT('Ctrl Pts',(-6.71657075814878,-4.20761134022216,
1.90091809908996));
#39954=CARTESIAN_POINT('Ctrl Pts',(-6.01883023249209,-5.3214080435446,1.94052055948766));
#39955=CARTESIAN_POINT('Ctrl Pts',(-5.03807888599404,-6.25791194850595,
1.98012301988537));
#39956=CARTESIAN_POINT('Ctrl Pts',(-3.89327950730805,-6.9035273977777,2.01972548028308));
#39957=CARTESIAN_POINT('Ctrl Pts',(-2.74848012862205,-7.54914284704945,
2.05932794068079));
#39958=CARTESIAN_POINT('Ctrl Pts',(-1.43963271774809,-7.90386984063161,
2.0989304010785));
#39959=CARTESIAN_POINT('Ctrl Pts',(-0.125497325076411,-7.92468083470104,
2.1385328614762));
#39960=CARTESIAN_POINT('Ctrl Pts',(1.18863806759526,-7.94549182877046,2.17813532187391));
#39961=CARTESIAN_POINT('Ctrl Pts',(2.50806144206467,-7.63238682332716,2.21773778227162));
#39962=CARTESIAN_POINT('Ctrl Pts',(3.67272990690861,-7.02334470981914,2.25734024266932));
#39963=CARTESIAN_POINT('Ctrl Pts',(4.83739837175256,-6.41430259631112,2.29694270306703));
#39964=CARTESIAN_POINT('Ctrl Pts',(5.84731192697105,-5.50932337473839,2.33654516346474));
#39965=CARTESIAN_POINT('Ctrl Pts',(6.57997048089828,-4.41817885144047,2.37614762386244));
#39966=CARTESIAN_POINT('Ctrl Pts',(7.31262903482551,-3.32703432814256,2.41575008426015));
#39967=CARTESIAN_POINT('Ctrl Pts',(7.76803258746148,-2.04972450311947,2.45535254465786));
#39968=CARTESIAN_POINT('Ctrl Pts',(7.89094177996011,-0.741183995942706,
2.49495500505557));
#39969=CARTESIAN_POINT('Ctrl Pts',(8.01385097245874,0.567356511234078,2.53455746545328));
#39970=CARTESIAN_POINT('Ctrl Pts',(7.80426580482004,1.90712770056451,2.57415992585098));
#39971=CARTESIAN_POINT('Ctrl Pts',(7.28760845528799,3.11561854086603,2.61376238624869));
#39972=CARTESIAN_POINT('Ctrl Pts',(6.77095110575595,4.32410938116752,2.6533648466464));
#39973=CARTESIAN_POINT('Ctrl Pts',(5.94722157433056,5.40131987244009,2.69296730704411));
#39974=CARTESIAN_POINT('Ctrl Pts',(4.91633627744731,6.21658696537909,2.73256976744181));
#39975=CARTESIAN_POINT('Ctrl Pts',(3.88545098056406,7.03185405831809,2.77217222783952));
#39976=CARTESIAN_POINT('Ctrl Pts',(2.64740991822295,7.58517775292355,2.81177468823723));
#39977=CARTESIAN_POINT('Ctrl Pts',(1.35238450192072,7.80944121234524,2.85137714863493));
#39978=CARTESIAN_POINT('Ctrl Pts',(0.0573590856184794,8.03370467176694,
2.89097960903264));
#39979=CARTESIAN_POINT('Ctrl Pts',(-1.29465068464487,7.92890789600487,2.93058206943035));
#39980=CARTESIAN_POINT('Ctrl Pts',(-2.53964926648632,7.50776248251543,2.97018452982806));
#39981=CARTESIAN_POINT('Ctrl Pts',(-3.78464784832777,7.08661706902599,3.00978699022577));
#39982=CARTESIAN_POINT('Ctrl Pts',(-4.92263524174732,6.34912301780917,3.04938945062347));
#39983=CARTESIAN_POINT('Ctrl Pts',(-5.81557630533137,5.38473658847692,3.08899191102118));
#39984=CARTESIAN_POINT('Ctrl Pts',(-6.70851736891541,4.42035015914468,3.12859437141889));
#39985=CARTESIAN_POINT('Ctrl Pts',(-7.35641210266396,3.229071351697,3.16819683181659));
#39986=CARTESIAN_POINT('Ctrl Pts',(-7.6806724293244,1.95539942822157,3.2077992922143));
#39987=CARTESIAN_POINT('Ctrl Pts',(-7.84310333858861,1.31738215745299,3.22763725302113));
#39988=CARTESIAN_POINT('Ctrl Pts',(-7.92432520227825,0.658690118588125,
3.24747521382796));
#39989=CARTESIAN_POINT('Ctrl Pts',(-7.92432847716457,-1.12691906257078E-6,
3.26731317463479));
#39990=CARTESIAN_POINT('Origin',(0.,0.,0.));
#39991=CARTESIAN_POINT('',(-7.92549788412615,0.000128118915216219,4.9826868253652));
#39992=CARTESIAN_POINT('',(-7.92541478162738,0.000152176599558203,4.76731317463479));
#39993=CARTESIAN_POINT('',(-7.925,-9.70532588324277E-16,0.));
#39994=CARTESIAN_POINT('Ctrl Pts',(-7.92549788412615,0.000128118915216219,
4.9826868253652));
#39995=CARTESIAN_POINT('Ctrl Pts',(-7.9256005347688,0.133414831212393,4.97867089335104));
#39996=CARTESIAN_POINT('Ctrl Pts',(-7.92230720286013,0.266696470636857,
4.97465496133688));
#39997=CARTESIAN_POINT('Ctrl Pts',(-7.91558408688892,0.399804876554018,
4.97063902932271));
#39998=CARTESIAN_POINT('Ctrl Pts',(-7.84928517220114,1.71243177246342,4.931036568925));
#39999=CARTESIAN_POINT('Ctrl Pts',(-7.44945356408088,3.00821240714173,4.89143410852729));
#40000=CARTESIAN_POINT('Ctrl Pts',(-6.76458787761404,4.12997169747715,4.85183164812959));
#40001=CARTESIAN_POINT('Ctrl Pts',(-6.0797221911472,5.2517309878126,4.81222918773188));
#40002=CARTESIAN_POINT('Ctrl Pts',(-5.10982242633376,6.19946893380517,4.77262672733417));
#40003=CARTESIAN_POINT('Ctrl Pts',(-3.97253509838228,6.8582271957151,4.73302426693646));
#40004=CARTESIAN_POINT('Ctrl Pts',(-2.83524777043081,7.51698545762502,4.69342180653876));
#40005=CARTESIAN_POINT('Ctrl Pts',(-1.5305728793413,7.88676403545229,4.65381934614105));
#40006=CARTESIAN_POINT('Ctrl Pts',(-0.216764360195708,7.92270967460465,
4.61421688574334));
#40007=CARTESIAN_POINT('Ctrl Pts',(1.09704415894986,7.95865531375702,4.57461442534563));
#40008=CARTESIAN_POINT('Ctrl Pts',(2.4199863061515,7.66076801423447,4.53501196494793));
#40009=CARTESIAN_POINT('Ctrl Pts',(3.59159237197411,7.0651807909991,4.49540950455022));
#40010=CARTESIAN_POINT('Ctrl Pts',(4.76319843779671,6.46959356776373,4.45580704415251));
#40011=CARTESIAN_POINT('Ctrl Pts',(5.78346842224027,5.57630642081553,4.4162045837548));
#40012=CARTESIAN_POINT('Ctrl Pts',(6.52864602326593,4.4936729385681,4.3766021233571));
#40013=CARTESIAN_POINT('Ctrl Pts',(7.27382362429159,3.41103945632067,4.33699966295939));
#40014=CARTESIAN_POINT('Ctrl Pts',(7.74390884189933,2.13905963877403,4.29739720256168));
#40015=CARTESIAN_POINT('Ctrl Pts',(7.88188146667275,0.832021587007101,4.25779474216397));
#40016=CARTESIAN_POINT('Ctrl Pts',(8.01985409144617,-0.475016464759823,
4.21819228176627));
#40017=CARTESIAN_POINT('Ctrl Pts',(7.82571412338525,-1.81711275074703,4.17858982136856));
#40018=CARTESIAN_POINT('Ctrl Pts',(7.32301027497934,-3.03147421042508,4.13898736097086));
#40019=CARTESIAN_POINT('Ctrl Pts',(6.82030642657341,-4.24583567010315,4.09938490057315));
#40020=CARTESIAN_POINT('Ctrl Pts',(6.00903869782248,-5.33246230347208,4.05978244017544));
#40021=CARTESIAN_POINT('Ctrl Pts',(4.98761191843291,-6.15954890613194,4.02017997977773));
#40022=CARTESIAN_POINT('Ctrl Pts',(3.96618513904335,-6.9866355087918,3.98057751938002));
#40023=CARTESIAN_POINT('Ctrl Pts',(2.73459930901516,-7.55418208074261,3.94097505898231));
#40024=CARTESIAN_POINT('Ctrl Pts',(1.44224283562455,-7.79334658404302,3.90137259858461));
#40025=CARTESIAN_POINT('Ctrl Pts',(0.149886362233948,-8.03251108734343,
3.8617701381869));
#40026=CARTESIAN_POINT('Ctrl Pts',(-1.20324075451908,-7.94329352199344,
3.82216767778919));
#40027=CARTESIAN_POINT('Ctrl Pts',(-2.45300744079018,-7.5365157646855,3.78256521739149));
#40028=CARTESIAN_POINT('Ctrl Pts',(-3.70277412706129,-7.12973800737757,
3.74296275699378));
#40029=CARTESIAN_POINT('Ctrl Pts',(-4.84918038285048,-6.40540005811169,
3.70336029659607));
#40030=CARTESIAN_POINT('Ctrl Pts',(-5.75316987893714,-5.45136237284001,
3.66375783619837));
#40031=CARTESIAN_POINT('Ctrl Pts',(-6.65715937502381,-4.49732468756832,
3.62415537580066));
#40032=CARTESIAN_POINT('Ctrl Pts',(-7.31873211140794,-3.31358726629082,
3.58455291540295));
#40033=CARTESIAN_POINT('Ctrl Pts',(-7.6576409019202,-2.04373461906477,3.54495045500524));
#40034=CARTESIAN_POINT('Ctrl Pts',(-7.83525353172734,-1.37824031954997,
3.5241959117919));
#40035=CARTESIAN_POINT('Ctrl Pts',(-7.92424601523,-0.689094341500147,3.50344136857855));
#40036=CARTESIAN_POINT('Ctrl Pts',(-7.92433472984446,2.91513625877426E-5,
3.4826868253652));
#40037=CARTESIAN_POINT('Ctrl Pts',(-7.92432847716457,-1.12691906257078E-6,
3.26731317463479));
#40038=CARTESIAN_POINT('Ctrl Pts',(-7.92433173992378,-0.656253197336447,
3.28707767422567));
#40039=CARTESIAN_POINT('Ctrl Pts',(-7.84371681523565,-1.31250448026098,
3.30684217381655));
#40040=CARTESIAN_POINT('Ctrl Pts',(-7.68247426549688,-1.94830825344823,
3.32660667340742));
#40041=CARTESIAN_POINT('Ctrl Pts',(-7.35938985543661,-3.22227897213938,
3.36620913380513));
#40042=CARTESIAN_POINT('Ctrl Pts',(-6.71259511574375,-4.4141553700185,3.40581159420284));
#40043=CARTESIAN_POINT('Ctrl Pts',(-5.82054469703419,-5.37936569869396,
3.44541405460055));
#40044=CARTESIAN_POINT('Ctrl Pts',(-4.92849427832463,-6.34457602736943,
3.48501651499825));
#40045=CARTESIAN_POINT('Ctrl Pts',(-3.79118818059835,-7.08312028684125,
3.52461897539596));
#40046=CARTESIAN_POINT('Ctrl Pts',(-2.54657890572889,-7.50541482979923,
3.56422143579367));
#40047=CARTESIAN_POINT('Ctrl Pts',(-1.30196963085945,-7.92770937275721,
3.60382389619138));
#40048=CARTESIAN_POINT('Ctrl Pts',(0.0499428211531797,-8.03375419920136,
3.64342635658908));
#40049=CARTESIAN_POINT('Ctrl Pts',(1.34517471238414,-7.81068632602966,3.68302881698679));
#40050=CARTESIAN_POINT('Ctrl Pts',(2.6404066036151,-7.58761845285795,3.7226312773845));
#40051=CARTESIAN_POINT('Ctrl Pts',(3.87895793406438,-7.0354378800704,3.76223373778221));
#40052=CARTESIAN_POINT('Ctrl Pts',(4.91059539796127,-6.22112278676367,3.80183619817991));
#40053=CARTESIAN_POINT('Ctrl Pts',(5.94223286185817,-5.40680769345693,3.84143865857762));
#40054=CARTESIAN_POINT('Ctrl Pts',(6.76695645920266,-4.33035807963103,3.88104111897533));
#40055=CARTESIAN_POINT('Ctrl Pts',(7.28472919570126,-3.12234470162488,3.92064357937303));
#40056=CARTESIAN_POINT('Ctrl Pts',(7.80250193219985,-1.91433132361873,3.96024603977074));
#40057=CARTESIAN_POINT('Ctrl Pts',(8.01332380785255,-0.574754181432342,
3.99984850016845));
#40058=CARTESIAN_POINT('Ctrl Pts',(7.89162263479,0.733899230506076,4.03945096056616));
#40059=CARTESIAN_POINT('Ctrl Pts',(7.76992146172746,2.0425526424445,4.07905342096387));
#40060=CARTESIAN_POINT('Ctrl Pts',(7.31569723994968,3.32028232413496,4.11865588136157));
#40061=CARTESIAN_POINT('Ctrl Pts',(6.58404627812082,4.41210272976854,4.15825834175928));
#40062=CARTESIAN_POINT('Ctrl Pts',(5.85239531629196,5.50392313540212,4.19786080215699));
#40063=CARTESIAN_POINT('Ctrl Pts',(4.84331761441201,6.40983426497883,4.2374632625547));
#40064=CARTESIAN_POINT('Ctrl Pts',(3.67921187748911,7.01995127127036,4.2770657229524));
#40065=CARTESIAN_POINT('Ctrl Pts',(2.51510614056621,7.63006827756189,4.31666818335011));
#40066=CARTESIAN_POINT('Ctrl Pts',(1.19597236860035,7.94439116056824,4.35627064374782));
#40067=CARTESIAN_POINT('Ctrl Pts',(-0.118181675755223,7.92479330847078,
4.39587310414552));
#40068=CARTESIAN_POINT('Ctrl Pts',(-1.43233572011079,7.90519545637331,4.43547556454323));
#40069=CARTESIAN_POINT('Ctrl Pts',(-2.74151003685607,7.55167686917203,4.47507802494094));
#40070=CARTESIAN_POINT('Ctrl Pts',(-3.88690492136875,6.90711850359517,4.51468048533865));
#40071=CARTESIAN_POINT('Ctrl Pts',(-5.03229980588144,6.26256013801832,4.55428294573635));
#40072=CARTESIAN_POINT('Ctrl Pts',(-6.01391525816152,5.32696199406589,4.59388540613406));
#40073=CARTESIAN_POINT('Ctrl Pts',(-6.71268367821032,4.21380988260697,4.63348786653177));
#40074=CARTESIAN_POINT('Ctrl Pts',(-7.41145209825913,3.10065777114805,4.67309032692948));
#40075=CARTESIAN_POINT('Ctrl Pts',(-7.82737348607664,1.80995169218265,4.71269278732718));
#40076=CARTESIAN_POINT('Ctrl Pts',(-7.90999757489035,0.498251197385663,
4.75229524772489));
#40077=CARTESIAN_POINT('Ctrl Pts',(-7.92044172839613,0.332444814308169,
4.75730122336152));
#40078=CARTESIAN_POINT('Ctrl Pts',(-7.92556032633143,0.166302974182222,
4.76230719899816));
#40079=CARTESIAN_POINT('Ctrl Pts',(-7.92541478162738,0.000152176599558203,
4.76731317463479));
#40080=CARTESIAN_POINT('Origin',(0.,0.,0.));
#40081=CARTESIAN_POINT('',(-7.92482915763566,-0.000199399977182102,6.4826868253652));
#40082=CARTESIAN_POINT('',(-7.92492875745862,-0.000203300716254766,6.26731317463479));
#40083=CARTESIAN_POINT('',(-7.925,-9.70532588324277E-16,0.));
#40084=CARTESIAN_POINT('Ctrl Pts',(-7.92482915763566,-0.000199399977182102,
6.4826868253652));
#40085=CARTESIAN_POINT('Ctrl Pts',(-7.92390949144967,0.955439152281158,
6.45390041812353));
#40086=CARTESIAN_POINT('Ctrl Pts',(-7.75084131112706,1.91140179707541,6.42511401088185));
#40087=CARTESIAN_POINT('Ctrl Pts',(-7.41274235439825,2.80491820972297,6.39632760364018));
#40088=CARTESIAN_POINT('Ctrl Pts',(-6.94760787506061,4.03415977674095,6.35672514324247));
#40089=CARTESIAN_POINT('Ctrl Pts',(-6.17012854586171,5.14521272810185,6.31712268284476));
#40090=CARTESIAN_POINT('Ctrl Pts',(-5.1746107446823,6.0033090056188,6.27752022244705));
#40091=CARTESIAN_POINT('Ctrl Pts',(-4.17909294350288,6.86140528313575,6.23791776204934));
#40092=CARTESIAN_POINT('Ctrl Pts',(-2.96553667034296,7.46654488680876,6.19831530165164));
#40093=CARTESIAN_POINT('Ctrl Pts',(-1.68114339047374,7.74532583411388,6.15871284125393));
#40094=CARTESIAN_POINT('Ctrl Pts',(-0.396750110604525,8.02410678141899,
6.11911038085622));
#40095=CARTESIAN_POINT('Ctrl Pts',(0.958480175973984,7.9765290723562,6.07950792045851));
#40096=CARTESIAN_POINT('Ctrl Pts',(2.22016128596198,7.60836376892173,6.03990546006081));
#40097=CARTESIAN_POINT('Ctrl Pts',(3.48184239594998,7.24019846548726,6.0003029996631));
#40098=CARTESIAN_POINT('Ctrl Pts',(4.64997432934747,6.5514455676811,5.9607005392654));
#40099=CARTESIAN_POINT('Ctrl Pts',(5.58286548434806,5.62564915006263,5.92109807886769));
#40100=CARTESIAN_POINT('Ctrl Pts',(6.51575663934865,4.69985273244416,5.88149561846998));
#40101=CARTESIAN_POINT('Ctrl Pts',(7.21340701595235,3.53701279501336,5.84189315807227));
#40102=CARTESIAN_POINT('Ctrl Pts',(7.59119329676186,2.2781790331585,5.80229069767456));
#40103=CARTESIAN_POINT('Ctrl Pts',(7.96897957757138,1.01934527130364,5.76268823727685));
#40104=CARTESIAN_POINT('Ctrl Pts',(8.02690176258671,-0.335482314975283,
5.72308577687915));
#40105=CARTESIAN_POINT('Ctrl Pts',(7.7579340296894,-1.62196638895895,5.68348331648145));
#40106=CARTESIAN_POINT('Ctrl Pts',(7.48896629679208,-2.90845046294262,5.64388085608374));
#40107=CARTESIAN_POINT('Ctrl Pts',(6.89310864598212,-4.12659102463103,5.60427839568602));
#40108=CARTESIAN_POINT('Ctrl Pts',(6.04263718116354,-5.12863054554968,5.56467593528832));
#40109=CARTESIAN_POINT('Ctrl Pts',(5.19216571634494,-6.13067006646835,5.52507347489061));
#40110=CARTESIAN_POINT('Ctrl Pts',(4.08708043751773,-6.91660854661725,5.48547101449291));
#40111=CARTESIAN_POINT('Ctrl Pts',(2.86142553850362,-7.39111353339431,5.4458685540952));
#40112=CARTESIAN_POINT('Ctrl Pts',(1.63577063948951,-7.86561852017137,5.40626609369749));
#40113=CARTESIAN_POINT('Ctrl Pts',(0.289546120288506,-8.0286900135766,5.36666363329978));
#40114=CARTESIAN_POINT('Ctrl Pts',(-1.01395421378253,-7.86054783257998,
5.32706117290207));
#40115=CARTESIAN_POINT('Ctrl Pts',(-2.31745454785354,-7.69240565158337,
5.28745871250436));
#40116=CARTESIAN_POINT('Ctrl Pts',(-3.57823069679459,-7.19304979618491,
5.24785625210666));
#40117=CARTESIAN_POINT('Ctrl Pts',(-4.64335353765705,-6.42305093396068,
5.20825379170896));
#40118=CARTESIAN_POINT('Ctrl Pts',(-5.70847637851951,-5.65305207173644,
5.16865133131125));
#40119=CARTESIAN_POINT('Ctrl Pts',(-6.57794591130339,-4.61241020268642,
5.12904887091354));
#40120=CARTESIAN_POINT('Ctrl Pts',(-7.14629756706768,-3.42735268959116,
5.08944641051583));
#40121=CARTESIAN_POINT('Ctrl Pts',(-7.65701488428923,-2.36246726574673,
5.05385988213228));
#40122=CARTESIAN_POINT('Ctrl Pts',(-7.92458826215163,-1.1809704040634,5.01827335374875));
#40123=CARTESIAN_POINT('Ctrl Pts',(-7.92549788412615,0.000128118915216219,
4.9826868253652));
#40124=CARTESIAN_POINT('Ctrl Pts',(-7.92541478162738,0.000152176599558203,
4.76731317463479));
#40125=CARTESIAN_POINT('Ctrl Pts',(-7.92440891673685,-1.14812219664027,
4.80190965939586));
#40126=CARTESIAN_POINT('Ctrl Pts',(-7.67197476697247,-2.29682439984853,
4.83650614415694));
#40127=CARTESIAN_POINT('Ctrl Pts',(-7.18838400348709,-3.33818083825282,
4.87110262891801));
#40128=CARTESIAN_POINT('Ctrl Pts',(-6.63481955346023,-4.53021746846575,
4.91070508931572));
#40129=CARTESIAN_POINT('Ctrl Pts',(-5.77836386359658,-5.58159581826305,
4.95030754971343));
#40130=CARTESIAN_POINT('Ctrl Pts',(-4.7229029549041,-6.36478621550053,4.98991001011114));
#40131=CARTESIAN_POINT('Ctrl Pts',(-3.66744204621164,-7.14797661273799,
5.02951247050884));
#40132=CARTESIAN_POINT('Ctrl Pts',(-2.41297591869036,-7.66297905741564,
5.06911493090655));
#40133=CARTESIAN_POINT('Ctrl Pts',(-1.11166830482495,-7.84732498820554,
5.10871739130425));
#40134=CARTESIAN_POINT('Ctrl Pts',(0.189639309040495,-8.03167091899544,
5.14831985170196));
#40135=CARTESIAN_POINT('Ctrl Pts',(1.53778840925007,-7.88536033589756,5.18792231209968));
#40136=CARTESIAN_POINT('Ctrl Pts',(2.76925174342659,-7.42614036172198,5.22752477249738));
#40137=CARTESIAN_POINT('Ctrl Pts',(4.0007150776031,-6.96692038754639,5.26712723289509));
#40138=CARTESIAN_POINT('Ctrl Pts',(5.11549264574657,-6.1947910222931,5.30672969329279));
#40139=CARTESIAN_POINT('Ctrl Pts',(5.97836460258773,-5.20340970604791,5.3463321536905));
#40140=CARTESIAN_POINT('Ctrl Pts',(6.84123655942888,-4.21202838980272,5.38593461408821));
#40141=CARTESIAN_POINT('Ctrl Pts',(7.45220290496774,-3.00139512256563,5.42553707448592));
#40142=CARTESIAN_POINT('Ctrl Pts',(7.73715488686723,-1.71835681600012,5.46513953488363));
#40143=CARTESIAN_POINT('Ctrl Pts',(8.02210686876671,-0.435318509434607,
5.50474199528134));
#40144=CARTESIAN_POINT('Ctrl Pts',(7.98104448702682,0.920124836459304,5.54434445567904));
#40145=CARTESIAN_POINT('Ctrl Pts',(7.61894851006622,2.1835611947979,5.58394691607674));
#40146=CARTESIAN_POINT('Ctrl Pts',(7.25685253310561,3.44699755313651,5.62354937647445));
#40147=CARTESIAN_POINT('Ctrl Pts',(6.57372296092429,4.61842692391978,5.66315183687216));
#40148=CARTESIAN_POINT('Ctrl Pts',(5.65242177217065,5.5557577340952,5.70275429726987));
#40149=CARTESIAN_POINT('Ctrl Pts',(4.73112058341702,6.4930885442706,5.74235675766758));
#40150=CARTESIAN_POINT('Ctrl Pts',(3.57164777809107,7.19632079383816,5.78195921806528));
#40151=CARTESIAN_POINT('Ctrl Pts',(2.31464462653267,7.58015409759795,5.82156167846299));
#40152=CARTESIAN_POINT('Ctrl Pts',(1.05764147497426,7.96398740135773,5.8611641388607));
#40153=CARTESIAN_POINT('Ctrl Pts',(-0.296892022816619,8.02842175930975,
5.90076659925841));
#40154=CARTESIAN_POINT('Ctrl Pts',(-1.58465420234887,7.76564143837748,5.94036905965612));
#40155=CARTESIAN_POINT('Ctrl Pts',(-2.87241638188114,7.50286111744522,5.97997152005382));
#40156=CARTESIAN_POINT('Ctrl Pts',(-4.09340724315476,6.91286611762868,6.01957398045153));
#40157=CARTESIAN_POINT('Ctrl Pts',(-5.09952352319192,6.06722141732769,6.05917644084924));
#40158=CARTESIAN_POINT('Ctrl Pts',(-6.10563980322905,5.22157671702672,6.09877890124694));
#40159=CARTESIAN_POINT('Ctrl Pts',(-6.8968815020297,4.12028231624131,6.13838136164465));
#40160=CARTESIAN_POINT('Ctrl Pts',(-7.37727289928889,2.896922584379,6.17798382204235));
#40161=CARTESIAN_POINT('Ctrl Pts',(-7.73847143827851,1.97709814470656,6.2077602729065));
#40162=CARTESIAN_POINT('Ctrl Pts',(-7.92393718090885,0.98826659176352,6.23753672377064));
#40163=CARTESIAN_POINT('Ctrl Pts',(-7.92492875745862,-0.000203300716254766,
6.26731317463479));
#40164=CARTESIAN_POINT('Origin',(0.,0.,0.));
#40165=CARTESIAN_POINT('',(-7.92455486516943,0.000157560269493928,7.9826868253652));
#40166=CARTESIAN_POINT('',(-7.92448697665393,0.000136394684465916,7.76731317463479));
#40167=CARTESIAN_POINT('',(-7.925,-9.70532588324277E-16,0.));
#40168=CARTESIAN_POINT('Ctrl Pts',(-7.92455486516943,0.000157560269493928,
7.9826868253652));
#40169=CARTESIAN_POINT('Ctrl Pts',(-7.92488905702959,0.463456370592923,
7.96873240329372));
#40170=CARTESIAN_POINT('Ctrl Pts',(-7.88492338787207,0.926698172538998,
7.95477798122224));
#40171=CARTESIAN_POINT('Ctrl Pts',(-7.80412960742409,1.38270620395372,7.94082355915076));
#40172=CARTESIAN_POINT('Ctrl Pts',(-7.57483795534541,2.67685080647717,7.90122109875306));
#40173=CARTESIAN_POINT('Ctrl Pts',(-7.01670987890586,3.9127334135031,7.86161863835535));
#40174=CARTESIAN_POINT('Ctrl Pts',(-6.19744497513114,4.94044442901112,7.82201617795764));
#40175=CARTESIAN_POINT('Ctrl Pts',(-5.37818007135641,5.96815544451915,7.78241371755994));
#40176=CARTESIAN_POINT('Ctrl Pts',(-4.2977783402465,6.78769486850925,7.74281125716223));
#40177=CARTESIAN_POINT('Ctrl Pts',(-3.08728992048746,7.29965453448188,7.70320879676452));
#40178=CARTESIAN_POINT('Ctrl Pts',(-1.87680150072842,7.8116142004545,7.66360633636682));
#40179=CARTESIAN_POINT('Ctrl Pts',(-0.536226392320244,8.01599410840963,
7.62400387596911));
#40180=CARTESIAN_POINT('Ctrl Pts',(0.771826859399493,7.88800346570884,7.5844014155714));
#40181=CARTESIAN_POINT('Ctrl Pts',(2.07988011111925,7.76001282300805,7.54479895517369));
#40182=CARTESIAN_POINT('Ctrl Pts',(3.35541150615052,7.29965162965135,7.50519649477599));
#40183=CARTESIAN_POINT('Ctrl Pts',(4.44370214558388,6.56276059423613,7.46559403437828));
#40184=CARTESIAN_POINT('Ctrl Pts',(5.53199278501721,5.82586955882093,7.42599157398057));
#40185=CARTESIAN_POINT('Ctrl Pts',(6.43304266885262,4.81244868134719,7.38638911358286));
#40186=CARTESIAN_POINT('Ctrl Pts',(7.03755660731061,3.64542348360573,7.34678665318516));
#40187=CARTESIAN_POINT('Ctrl Pts',(7.64207054576862,2.47839828586421,7.30718419278745));
#40188=CARTESIAN_POINT('Ctrl Pts',(7.95004853884922,1.15776876785491,7.26758173238974));
#40189=CARTESIAN_POINT('Ctrl Pts',(7.92413359466385,-0.156275877361342,
7.22797927199203));
#40190=CARTESIAN_POINT('Ctrl Pts',(7.89821865047848,-1.47032052257757,7.18837681159432));
#40191=CARTESIAN_POINT('Ctrl Pts',(7.53841076902715,-2.77778029500072,7.14877435119662));
#40192=CARTESIAN_POINT('Ctrl Pts',(6.88835378334602,-3.92006346012254,7.10917189079891));
#40193=CARTESIAN_POINT('Ctrl Pts',(6.23829679766489,-5.06234662524434,7.0695694304012));
#40194=CARTESIAN_POINT('Ctrl Pts',(5.29799070775395,-6.0394531830648,7.0299669700035));
#40195=CARTESIAN_POINT('Ctrl Pts',(4.18149238703527,-6.73286245166878,6.99036450960579));
#40196=CARTESIAN_POINT('Ctrl Pts',(3.06499406631659,-7.42627172027276,6.95076204920808));
#40197=CARTESIAN_POINT('Ctrl Pts',(1.77230351479016,-7.83598369966026,6.91115958881037));
#40198=CARTESIAN_POINT('Ctrl Pts',(0.460220995892857,-7.91230130940832,
6.87155712841267));
#40199=CARTESIAN_POINT('Ctrl Pts',(-0.851861523004442,-7.98861891915639,
6.83195466801496));
#40200=CARTESIAN_POINT('Ctrl Pts',(-2.18333600927261,-7.73154215926501,
6.79235220761725));
#40201=CARTESIAN_POINT('Ctrl Pts',(-3.37269780121221,-7.17225382412137,
6.75274974721954));
#40202=CARTESIAN_POINT('Ctrl Pts',(-4.56205959315182,-6.61296548897771,
6.71314728682183));
#40203=CARTESIAN_POINT('Ctrl Pts',(-5.60930869076286,-5.75146557858178,
6.67354482642413));
#40204=CARTESIAN_POINT('Ctrl Pts',(-6.38741629028751,-4.69225196579373,
6.63394236602643));
#40205=CARTESIAN_POINT('Ctrl Pts',(-7.16552388981217,-3.63303835300566,
6.59433990562872));
#40206=CARTESIAN_POINT('Ctrl Pts',(-7.67448999125043,-2.37611103782545,
6.554737445231));
#40207=CARTESIAN_POINT('Ctrl Pts',(-7.85257822723136,-1.07393228889779,
6.51513498483329));
#40208=CARTESIAN_POINT('Ctrl Pts',(-7.90121691804727,-0.71828684602346,
6.50431893167726));
#40209=CARTESIAN_POINT('Ctrl Pts',(-7.92517470816823,-0.359266000140281,
6.49350287852123));
#40210=CARTESIAN_POINT('Ctrl Pts',(-7.92482915763566,-0.000199399977182102,
6.4826868253652));
#40211=CARTESIAN_POINT('Ctrl Pts',(-7.92492875745862,-0.000203300716254766,
6.26731317463479));
#40212=CARTESIAN_POINT('Ctrl Pts',(-7.92525597041882,-0.326391086878601,
6.27713918416835));
#40213=CARTESIAN_POINT('Ctrl Pts',(-7.90549484318086,-0.652539489974055,
6.28696519370192));
#40214=CARTESIAN_POINT('Ctrl Pts',(-7.86533125816864,-0.976155771249044,
6.29679120323548));
#40215=CARTESIAN_POINT('Ctrl Pts',(-7.70345712407144,-2.28044933207546,
6.33639366363319));
#40216=CARTESIAN_POINT('Ctrl Pts',(-7.2101677601593,-3.54361139078904,6.3759961240309));
#40217=CARTESIAN_POINT('Ctrl Pts',(-6.44529798314124,-4.61242341930822,
6.4155985844286));
#40218=CARTESIAN_POINT('Ctrl Pts',(-5.68042820612317,-5.68123544782742,
6.45520104482631));
#40219=CARTESIAN_POINT('Ctrl Pts',(-4.64397801599918,-6.55569744615223,
6.49480350522402));
#40220=CARTESIAN_POINT('Ctrl Pts',(-3.4616663349496,-7.12973927124577,6.53440596562173));
#40221=CARTESIAN_POINT('Ctrl Pts',(-2.27935465390004,-7.70378109633929,
6.57400842601944));
#40222=CARTESIAN_POINT('Ctrl Pts',(-0.951181481924927,-7.97740274820154,
6.61361088641714));
#40223=CARTESIAN_POINT('Ctrl Pts',(0.361748960782006,-7.91741457673151,
6.65321334681485));
#40224=CARTESIAN_POINT('Ctrl Pts',(1.67467940348893,-7.85742640526148,6.69281580721256));
#40225=CARTESIAN_POINT('Ctrl Pts',(2.97236711692768,-7.46382841045917,6.73241826761026));
#40226=CARTESIAN_POINT('Ctrl Pts',(4.09740569390686,-6.78436308506606,6.77202072800797));
#40227=CARTESIAN_POINT('Ctrl Pts',(5.22244427088606,-6.10489775967295,6.81162318840568));
#40228=CARTESIAN_POINT('Ctrl Pts',(6.1748337114057,-5.13956510368905,6.85122564880339));
#40229=CARTESIAN_POINT('Ctrl Pts',(6.8390514605963,-4.00545765297588,6.89082810920109));
#40230=CARTESIAN_POINT('Ctrl Pts',(7.5032692097869,-2.87135020226273,6.9304305695988));
#40231=CARTESIAN_POINT('Ctrl Pts',(7.87931526764847,-1.56846795682031,6.97003302999651));
#40232=CARTESIAN_POINT('Ctrl Pts',(7.92157614929286,-0.254847408113207,
7.00963549039422));
#40233=CARTESIAN_POINT('Ctrl Pts',(7.96383703093724,1.05877314059392,7.04923795079192));
#40234=CARTESIAN_POINT('Ctrl Pts',(7.67231273636446,2.38313199256569,7.08884041118962));
#40235=CARTESIAN_POINT('Ctrl Pts',(7.08236446329754,3.5575875954764,7.12844287158733));
#40236=CARTESIAN_POINT('Ctrl Pts',(6.49241619023065,4.73204319838707,7.16804533198504));
#40237=CARTESIAN_POINT('Ctrl Pts',(5.60404393866961,5.75659555223666,7.20764779238275));
#40238=CARTESIAN_POINT('Ctrl Pts',(4.52500513200579,6.50696891384835,7.24725025278046));
#40239=CARTESIAN_POINT('Ctrl Pts',(3.44596632534194,7.25734227546006,7.28685271317817));
#40240=CARTESIAN_POINT('Ctrl Pts',(2.17626096357527,7.73353664483391,7.32645517357588));
#40241=CARTESIAN_POINT('Ctrl Pts',(0.869901261753817,7.87779078709676,7.36605763397359));
#40242=CARTESIAN_POINT('Ctrl Pts',(-0.436458440067604,8.0220449293596,7.40566009437129));
#40243=CARTESIAN_POINT('Ctrl Pts',(-1.7794724819438,7.83435884451148,7.445262554769));
#40244=CARTESIAN_POINT('Ctrl Pts',(-2.99623648175723,7.33749840448736,7.48486501516671));
#40245=CARTESIAN_POINT('Ctrl Pts',(-4.21300048157064,6.84063796446325,7.52446747556441));
#40246=CARTESIAN_POINT('Ctrl Pts',(-5.30351443932127,6.03460316926317,7.56406993596212));
#40247=CARTESIAN_POINT('Ctrl Pts',(-6.13550162748532,5.01716410630472,7.60367239635983));
#40248=CARTESIAN_POINT('Ctrl Pts',(-6.9674888156494,3.99972504334623,7.64327485675754));
#40249=CARTESIAN_POINT('Ctrl Pts',(-7.54094923422687,2.77088171262934,7.68287731715525));
#40250=CARTESIAN_POINT('Ctrl Pts',(-7.78632350986467,1.47968986284162,7.72247977755296));
#40251=CARTESIAN_POINT('Ctrl Pts',(-7.87891844986639,0.992443057727118,
7.7374242432469));
#40252=CARTESIAN_POINT('Ctrl Pts',(-7.92479322829447,0.496317691455577,
7.75236870894085));
#40253=CARTESIAN_POINT('Ctrl Pts',(-7.92448697665393,0.000136394684465916,
7.76731317463479));
#40254=CARTESIAN_POINT('Origin',(0.,0.,0.));
#40255=CARTESIAN_POINT('',(-7.92566451523509,-3.0530117057781E-5,9.4826868253652));
#40256=CARTESIAN_POINT('',(-7.92567438502354,3.93182477014807E-6,9.2673131746348));
#40257=CARTESIAN_POINT('',(-7.925,-9.70532588324277E-16,0.));
#40258=CARTESIAN_POINT('Ctrl Pts',(-7.92566451523509,-3.0530117057781E-5,
9.4826868253652));
#40259=CARTESIAN_POINT('Ctrl Pts',(-7.92538377707008,1.28515034464984,9.44396192806621));
#40260=CARTESIAN_POINT('Ctrl Pts',(-7.60662215046401,2.57046545380378,9.40523703076722));
#40261=CARTESIAN_POINT('Ctrl Pts',(-7.00560821546851,3.70644963641561,9.36651213346824));
#40262=CARTESIAN_POINT('Ctrl Pts',(-6.39097442121051,4.86817689051166,9.32690967307053));
#40263=CARTESIAN_POINT('Ctrl Pts',(-5.48115086564248,5.8737284137033,9.28730721267282));
#40264=CARTESIAN_POINT('Ctrl Pts',(-4.38649696388181,6.60113321799984,9.24770475227511));
#40265=CARTESIAN_POINT('Ctrl Pts',(-3.29184306212112,7.32853802229639,9.2081022918774));
#40266=CARTESIAN_POINT('Ctrl Pts',(-2.01235881416776,7.77779610769788,9.1684998314797));
#40267=CARTESIAN_POINT('Ctrl Pts',(-0.703242590509952,7.89441354597149,
9.12889737108199));
#40268=CARTESIAN_POINT('Ctrl Pts',(0.60587363314786,8.01103098424511,9.08929491068428));
#40269=CARTESIAN_POINT('Ctrl Pts',(1.94462183251012,7.79500777539085,9.04969245028657));
#40270=CARTESIAN_POINT('Ctrl Pts',(3.15061506192477,7.27254701652028,9.01008998988886));
#40271=CARTESIAN_POINT('Ctrl Pts',(4.35660829133941,6.75008625764971,8.97048752949116));
#40272=CARTESIAN_POINT('Ctrl Pts',(5.42984655080643,5.92118794876284,8.93088506909345));
#40273=CARTESIAN_POINT('Ctrl Pts',(6.24014861356879,4.88639546665032,8.89128260869575));
#40274=CARTESIAN_POINT('Ctrl Pts',(7.05045067633115,3.85160298453779,8.85168014829804));
#40275=CARTESIAN_POINT('Ctrl Pts',(7.59781654238885,2.61091632919961,8.81207768790033));
#40276=CARTESIAN_POINT('Ctrl Pts',(7.81585204502282,1.31482781619415,8.77247522750262));
#40277=CARTESIAN_POINT('Ctrl Pts',(8.03388754765679,0.0187393031886965,
8.73287276710491));
#40278=CARTESIAN_POINT('Ctrl Pts',(7.92259268686704,-1.33275106748403,8.69327030670721));
#40279=CARTESIAN_POINT('Ctrl Pts',(7.49546726233136,-2.57571075535358,8.6536678463095));
#40280=CARTESIAN_POINT('Ctrl Pts',(7.06834183779569,-3.81867044322313,8.6140653859118));
#40281=CARTESIAN_POINT('Ctrl Pts',(6.32538584951409,-4.95309944828949,8.57446292551408));
#40282=CARTESIAN_POINT('Ctrl Pts',(5.35671807691682,-5.84139425311781,8.53486046511638));
#40283=CARTESIAN_POINT('Ctrl Pts',(4.38805030431956,-6.72968905794612,8.49525800471867));
#40284=CARTESIAN_POINT('Ctrl Pts',(3.19367074740664,-7.3718496625364,8.45565554432097));
#40285=CARTESIAN_POINT('Ctrl Pts',(1.91845478176303,-7.68998352574672,8.41605308392326));
#40286=CARTESIAN_POINT('Ctrl Pts',(0.643238816119382,-8.00811738895705,
8.37645062352555));
#40287=CARTESIAN_POINT('Ctrl Pts',(-0.712813558254954,-8.00222451078741,
8.33684816312784));
#40288=CARTESIAN_POINT('Ctrl Pts',(-1.98521644078227,-7.67301968322596,
8.29724570273013));
#40289=CARTESIAN_POINT('Ctrl Pts',(-3.25761932330957,-7.34381485566452,
8.25764324233242));
#40290=CARTESIAN_POINT('Ctrl Pts',(-4.44637271398986,-6.69129807871128,
8.21804078193472));
#40291=CARTESIAN_POINT('Ctrl Pts',(-5.40728367770804,-5.79461807237694,
8.17843832153702));
#40292=CARTESIAN_POINT('Ctrl Pts',(-6.36819464142624,-4.89793806604258,
8.13883586113931));
#40293=CARTESIAN_POINT('Ctrl Pts',(-7.10126317818233,-3.75709483032712,
8.0992334007416));
#40294=CARTESIAN_POINT('Ctrl Pts',(-7.51756983270146,-2.51046991345888,
8.05963094034389));
#40295=CARTESIAN_POINT('Ctrl Pts',(-7.78718563241042,-1.70310887262521,
8.03398290201766));
#40296=CARTESIAN_POINT('Ctrl Pts',(-7.92394062506736,-0.851379363495959,
8.00833486369143));
#40297=CARTESIAN_POINT('Ctrl Pts',(-7.92455486516943,0.000157560269493928,
7.9826868253652));
#40298=CARTESIAN_POINT('Ctrl Pts',(-7.92448697665393,0.000136394684465916,
7.76731317463479));
#40299=CARTESIAN_POINT('Ctrl Pts',(-7.92398166910498,-0.818550337812214,
7.79197116933855));
#40300=CARTESIAN_POINT('Ctrl Pts',(-7.7977523179122,-1.63738933647875,7.81662916404231));
#40301=CARTESIAN_POINT('Ctrl Pts',(-7.54822065908196,-2.41675004340037,
7.84128715874607));
#40302=CARTESIAN_POINT('Ctrl Pts',(-7.1474553999633,-3.6684577309962,7.88088961914378));
#40303=CARTESIAN_POINT('Ctrl Pts',(-6.42863674902783,-4.81833273732931,
7.92049207954149));
#40304=CARTESIAN_POINT('Ctrl Pts',(-5.47895568457806,-5.72689798205777,
7.9600945399392));
#40305=CARTESIAN_POINT('Ctrl Pts',(-4.52927462012827,-6.63546322678623,
7.9996970003369));
#40306=CARTESIAN_POINT('Ctrl Pts',(-3.34873114216419,-7.30271870991004,
8.03929946073461));
#40307=CARTESIAN_POINT('Ctrl Pts',(-2.08052234307956,-7.64772794171015,
8.07890192113232));
#40308=CARTESIAN_POINT('Ctrl Pts',(-0.812313543994936,-7.99273717351026,
8.11850438153002));
#40309=CARTESIAN_POINT('Ctrl Pts',(0.543560576210242,-8.01550015398668,
8.15810684192774));
#40310=CARTESIAN_POINT('Ctrl Pts',(1.82263573876145,-7.71325578820364,8.19770930232545));
#40311=CARTESIAN_POINT('Ctrl Pts',(3.10171090131263,-7.41101142242061,8.23731176272315));
#40312=CARTESIAN_POINT('Ctrl Pts',(4.30398710620981,-6.78375971037817,8.27691422312085));
#40313=CARTESIAN_POINT('Ctrl Pts',(5.28363113340734,-5.90758478031049,8.31651668351856));
#40314=CARTESIAN_POINT('Ctrl Pts',(6.26327516060488,-5.0314098502428,8.35611914391626));
#40315=CARTESIAN_POINT('Ctrl Pts',(7.02028701010276,-3.90631170214984,8.39572160431398));
#40316=CARTESIAN_POINT('Ctrl Pts',(7.46284296021754,-2.66876204289534,8.43532406471169));
#40317=CARTESIAN_POINT('Ctrl Pts',(7.90539891033232,-1.43121238364084,8.4749265251094));
#40318=CARTESIAN_POINT('Ctrl Pts',(8.03349896106404,-0.0812112132247506,
8.51452898550711));
#40319=CARTESIAN_POINT('Ctrl Pts',(7.83160488350145,1.21748956430181,8.55413144590481));
#40320=CARTESIAN_POINT('Ctrl Pts',(7.62971080593885,2.51619034182838,8.59373390630252));
#40321=CARTESIAN_POINT('Ctrl Pts',(7.09782260008196,3.76359072646538,8.63333636670022));
#40322=CARTESIAN_POINT('Ctrl Pts',(6.30045702958997,4.80838404339315,8.67293882709792));
#40323=CARTESIAN_POINT('Ctrl Pts',(5.50309145909799,5.8531773603209,8.71254128749563));
#40324=CARTESIAN_POINT('Ctrl Pts',(4.44024852397089,6.69536360953942,8.75214374789334));
#40325=CARTESIAN_POINT('Ctrl Pts',(3.2408485230561,7.23278761896632,8.79174620829105));
#40326=CARTESIAN_POINT('Ctrl Pts',(2.04144852214128,7.77021162839325,8.83134866868876));
#40327=CARTESIAN_POINT('Ctrl Pts',(0.705491455438782,8.00287339802857,8.87095112908646));
#40328=CARTESIAN_POINT('Ctrl Pts',(-0.604974289096646,7.9025516132449,8.91055358948417));
#40329=CARTESIAN_POINT('Ctrl Pts',(-1.91544003363207,7.80222982846123,8.95015604988188));
#40330=CARTESIAN_POINT('Ctrl Pts',(-3.20041445600039,7.36892448925854,8.98975851027959));
#40331=CARTESIAN_POINT('Ctrl Pts',(-4.30403324072476,6.65519449401772,9.0293609706773));
#40332=CARTESIAN_POINT('Ctrl Pts',(-5.40765202544913,5.94146449877691,9.06896343107501));
#40333=CARTESIAN_POINT('Ctrl Pts',(-6.32991517252957,4.94730984749797,9.10856589147271));
#40334=CARTESIAN_POINT('Ctrl Pts',(-6.95895437423414,3.79331911494341,9.14816835187042));
#40335=CARTESIAN_POINT('Ctrl Pts',(-7.58799357593871,2.63932838238885,9.18777081226812));
#40336=CARTESIAN_POINT('Ctrl Pts',(-7.9238088322674,1.32550156855867,9.22737327266583));
#40337=CARTESIAN_POINT('Ctrl Pts',(-7.92566655806616,0.0112027148127723,
9.26697573306354));
#40338=CARTESIAN_POINT('Ctrl Pts',(-7.92567183445477,0.00746978958662008,
9.26708821358729));
#40339=CARTESIAN_POINT('Ctrl Pts',(-7.92567441681873,0.00373686055253689,
9.26720069411104));
#40340=CARTESIAN_POINT('Ctrl Pts',(-7.92567430608102,3.93136451648719E-6,
9.2673131746348));
#40341=CARTESIAN_POINT('Origin',(0.,0.,0.));
#40342=CARTESIAN_POINT('',(-7.92444197974487,-0.000117952357666096,10.9826868253652));
#40343=CARTESIAN_POINT('',(-7.92450147625162,-0.000141486819805631,10.7673131746348));
#40344=CARTESIAN_POINT('',(-7.925,-9.70532588324277E-16,0.));
#40345=CARTESIAN_POINT('Ctrl Pts',(-7.92444197974487,-0.000117952357666096,
10.9826868253652));
#40346=CARTESIAN_POINT('Ctrl Pts',(-7.92402168439202,0.79317964478778,10.9587939132364));
#40347=CARTESIAN_POINT('Ctrl Pts',(-7.80562445932409,1.58659993568632,10.9349010011076));
#40348=CARTESIAN_POINT('Ctrl Pts',(-7.57110679996587,2.34406851422498,10.9110080889788));
#40349=CARTESIAN_POINT('Ctrl Pts',(-7.18239418648314,3.5995713688952,10.8714056285811));
#40350=CARTESIAN_POINT('Ctrl Pts',(-6.47466384601646,4.75630406628582,10.8318031681834));
#40351=CARTESIAN_POINT('Ctrl Pts',(-5.53376177138355,5.67395770459255,10.7922007077857));
#40352=CARTESIAN_POINT('Ctrl Pts',(-4.59285969675065,6.59161134289928,10.752598247388));
#40353=CARTESIAN_POINT('Ctrl Pts',(-3.41878588795152,7.27018592212212,10.7129957869903));
#40354=CARTESIAN_POINT('Ctrl Pts',(-2.15395268203755,7.62737197332591,10.6733933265926));
#40355=CARTESIAN_POINT('Ctrl Pts',(-0.889119476123588,7.98455802452969,
10.6337908661949));
#40356=CARTESIAN_POINT('Ctrl Pts',(0.46647312690522,8.02035554771443,10.5941884057972));
#40357=CARTESIAN_POINT('Ctrl Pts',(1.74839499563781,7.73042238918058,10.5545859453995));
#40358=CARTESIAN_POINT('Ctrl Pts',(3.0303168643704,7.44048923064672,10.5149834850018));
#40359=CARTESIAN_POINT('Ctrl Pts',(4.23856799880677,6.82482539039427,10.475381024604));
#40360=CARTESIAN_POINT('Ctrl Pts',(5.22659043427609,5.95810941560032,10.4357785642063));
#40361=CARTESIAN_POINT('Ctrl Pts',(6.21461286974541,5.09139344080638,10.3961761038086));
#40362=CARTESIAN_POINT('Ctrl Pts',(6.98240660624767,3.97362533147094,10.3565736434109));
#40363=CARTESIAN_POINT('Ctrl Pts',(7.43684010506711,2.74038767833817,10.3169711830132));
#40364=CARTESIAN_POINT('Ctrl Pts',(7.89127360388654,1.5071500252054,10.2773687226155));
#40365=CARTESIAN_POINT('Ctrl Pts',(8.03234686502314,0.158442828275303,10.2377662622178));
#40366=CARTESIAN_POINT('Ctrl Pts',(7.84294804025856,-1.14213896428184,10.1981638018201));
#40367=CARTESIAN_POINT('Ctrl Pts',(7.65354921549399,-2.442720756839,10.1585613414224));
#40368=CARTESIAN_POINT('Ctrl Pts',(7.13367830482823,-3.69517714502321,10.1189588810247));
#40369=CARTESIAN_POINT('Ctrl Pts',(6.34639440283714,-4.7475881729108,10.079356420627));
#40370=CARTESIAN_POINT('Ctrl Pts',(5.55911050084605,-5.79999920079838,10.0397539602293));
#40371=CARTESIAN_POINT('Ctrl Pts',(4.50441360752963,-6.65236486838934,10.0001514998316));
#40372=CARTESIAN_POINT('Ctrl Pts',(3.31023592640137,-7.20129526456781,9.96054903943384));
#40373=CARTESIAN_POINT('Ctrl Pts',(2.11605824527312,-7.75022566074628,9.92094657903614));
#40374=CARTESIAN_POINT('Ctrl Pts',(0.782399776333046,-7.99572078551226,
9.88134411863843));
#40375=CARTESIAN_POINT('Ctrl Pts',(-0.52896990685943,-7.90800266904119,
9.84174165824072));
#40376=CARTESIAN_POINT('Ctrl Pts',(-1.84033959005191,-7.82028455257012,
9.80213919784301));
#40377=CARTESIAN_POINT('Ctrl Pts',(-3.12942048749678,-7.39935319486198,
9.76253673744531));
#40378=CARTESIAN_POINT('Ctrl Pts',(-4.23985017813971,-6.69626656002088,
9.7229342770476));
#40379=CARTESIAN_POINT('Ctrl Pts',(-5.35027986878263,-5.99317992517977,
9.68333181664989));
#40380=CARTESIAN_POINT('Ctrl Pts',(-6.28205835262362,-5.0079380132057,9.64372935625218));
#40381=CARTESIAN_POINT('Ctrl Pts',(-6.92216313440376,-3.86004830496029,
9.60412689585448));
#40382=CARTESIAN_POINT('Ctrl Pts',(-7.56226791618391,-2.71215859671488,
9.56452443545677));
#40383=CARTESIAN_POINT('Ctrl Pts',(-7.91069899590321,-1.40162109219814,
9.52492197505906));
#40384=CARTESIAN_POINT('Ctrl Pts',(-7.92519251928886,-0.0874008474395132,
9.48531951466136));
#40385=CARTESIAN_POINT('Ctrl Pts',(-7.92551368573069,-0.058278636879719,
9.48444195156264));
#40386=CARTESIAN_POINT('Ctrl Pts',(-7.92567087717459,-0.0291546179659009,
9.48356438846392));
#40387=CARTESIAN_POINT('Ctrl Pts',(-7.92566451523509,-3.0530117057781E-5,
9.4826868253652));
#40388=CARTESIAN_POINT('Ctrl Pts',(-7.92567430608102,3.93136451648719E-6,
9.2673131746348));
#40389=CARTESIAN_POINT('Ctrl Pts',(-7.9256354279719,-1.31056338809906,9.30680315450875));
#40390=CARTESIAN_POINT('Ctrl Pts',(-7.59364712907968,-2.62114968173378,
9.34629313438271));
#40391=CARTESIAN_POINT('Ctrl Pts',(-6.96965005365923,-3.77363141019302,
9.38578311425666));
#40392=CARTESIAN_POINT('Ctrl Pts',(-6.34387562818474,-4.92939578779125,
9.42538557465437));
#40393=CARTESIAN_POINT('Ctrl Pts',(-5.42442658196696,-5.92615364932607,
9.46498803505207));
#40394=CARTESIAN_POINT('Ctrl Pts',(-4.32282987905268,-6.64300065687463,
9.50459049544978));
#40395=CARTESIAN_POINT('Ctrl Pts',(-3.22123317613842,-7.35984766442319,
9.54419295584749));
#40396=CARTESIAN_POINT('Ctrl Pts',(-1.93748881652769,-7.7967838179855,9.5837954162452));
#40397=CARTESIAN_POINT('Ctrl Pts',(-0.627311912035025,-7.90080981010722,
9.6233978766429));
#40398=CARTESIAN_POINT('Ctrl Pts',(0.682864992457676,-8.00483580222894,
9.66300033704061));
#40399=CARTESIAN_POINT('Ctrl Pts',(2.01947444183229,-7.77595163291006,9.70260279743832));
#40400=CARTESIAN_POINT('Ctrl Pts',(3.22038891568058,-7.24192040292001,9.74220525783603));
#40401=CARTESIAN_POINT('Ctrl Pts',(4.42130338952884,-6.70788917292997,9.78180771823373));
#40402=CARTESIAN_POINT('Ctrl Pts',(5.48652288785077,-5.86871088226878,9.82141017863144));
#40403=CARTESIAN_POINT('Ctrl Pts',(6.28683884038356,-4.82617584486022,9.86101263902915));
#40404=CARTESIAN_POINT('Ctrl Pts',(7.08715479291634,-3.78364080745165,9.90061509942685));
#40405=CARTESIAN_POINT('Ctrl Pts',(7.62256719965997,-2.53774902329572,9.94021755982456));
#40406=CARTESIAN_POINT('Ctrl Pts',(7.82813181984032,-1.2396241775921,9.97982002022227));
#40407=CARTESIAN_POINT('Ctrl Pts',(8.03369644002068,0.0585006681115341,
10.01942248062));
#40408=CARTESIAN_POINT('Ctrl Pts',(7.90941327363775,1.40885857536285,10.0590249410177));
#40409=CARTESIAN_POINT('Ctrl Pts',(7.47035757068589,2.64765436878824,10.0986274014154));
#40410=CARTESIAN_POINT('Ctrl Pts',(7.03130186773404,3.8864501622136,10.1382298618131));
#40411=CARTESIAN_POINT('Ctrl Pts',(6.27747362821324,5.01368384181308,10.1778323222108));
#40412=CARTESIAN_POINT('Ctrl Pts',(5.30031040955247,5.89262466587319,10.2174347826085));
#40413=CARTESIAN_POINT('Ctrl Pts',(4.32314719089171,6.77156548993329,10.2570372430062));
#40414=CARTESIAN_POINT('Ctrl Pts',(3.12264899309097,7.40221345845408,10.2966397034039));
#40415=CARTESIAN_POINT('Ctrl Pts',(1.84443336819958,7.70807248543627,10.3362421638016));
#40416=CARTESIAN_POINT('Ctrl Pts',(0.566217743308195,8.01393151241845,10.3758446241993));
#40417=CARTESIAN_POINT('Ctrl Pts',(-0.789715308673824,7.99500159786202,
10.415447084597));
#40418=CARTESIAN_POINT('Ctrl Pts',(-2.05889436068869,7.65357889500015,10.4550495449948));
#40419=CARTESIAN_POINT('Ctrl Pts',(-3.32807341270356,7.31215619213827,10.4946520053925));
#40420=CARTESIAN_POINT('Ctrl Pts',(-4.51049846475127,6.64824070097095,10.5342544657902));
#40421=CARTESIAN_POINT('Ctrl Pts',(-5.4627441940148,5.74236377820361,10.5738569261879));
#40422=CARTESIAN_POINT('Ctrl Pts',(-6.41498992327833,4.83648685543627,10.6134593865856));
#40423=CARTESIAN_POINT('Ctrl Pts',(-7.13705632975766,3.68864850106897,10.6530618469833));
#40424=CARTESIAN_POINT('Ctrl Pts',(-7.54135849019206,2.43807875444513,10.692664307381));
#40425=CARTESIAN_POINT('Ctrl Pts',(-7.79538898898431,1.6523227343239,10.7175472631323));
#40426=CARTESIAN_POINT('Ctrl Pts',(-7.92397123184249,0.826009999126394,
10.7424302188835));
#40427=CARTESIAN_POINT('Ctrl Pts',(-7.92450147625162,-0.000141486819805631,
10.7673131746348));
#40428=CARTESIAN_POINT('Origin',(0.,0.,0.));
#40429=CARTESIAN_POINT('',(-7.92500786703747,0.000202977126703835,12.4826868253652));
#40430=CARTESIAN_POINT('',(-7.92490579193458,0.000202837437923534,12.2673131746348));
#40431=CARTESIAN_POINT('',(-7.925,-9.70532588324277E-16,0.));
#40432=CARTESIAN_POINT('Ctrl Pts',(-7.92500786703747,0.000202977126703835,
12.4826868253652));
#40433=CARTESIAN_POINT('Ctrl Pts',(-7.92531493217766,0.300984151116678,
12.4736258984066));
#40434=CARTESIAN_POINT('Ctrl Pts',(-7.90851822812937,0.601731230547898,
12.464564971448));
#40435=CARTESIAN_POINT('Ctrl Pts',(-7.87435266312157,0.900492052656451,
12.4555040444894));
#40436=CARTESIAN_POINT('Ctrl Pts',(-7.72502572986527,2.20628159052614,12.4159015840917));
#40437=CARTESIAN_POINT('Ctrl Pts',(-7.24390335415058,3.47412787300641,12.376299123694));
#40438=CARTESIAN_POINT('Ctrl Pts',(-6.48934464920618,4.5502440932928,12.3366966632963));
#40439=CARTESIAN_POINT('Ctrl Pts',(-5.73478594426178,5.62636031357918,12.2970942028986));
#40440=CARTESIAN_POINT('Ctrl Pts',(-4.70679091008767,6.51074647167168,12.2574917425009));
#40441=CARTESIAN_POINT('Ctrl Pts',(-3.5300528159044,7.09612869556788,12.2178892821032));
#40442=CARTESIAN_POINT('Ctrl Pts',(-2.35331472172112,7.68151091946408,12.1782868217055));
#40443=CARTESIAN_POINT('Ctrl Pts',(-1.02783356752869,7.96788920916399,12.1386843613077));
#40444=CARTESIAN_POINT('Ctrl Pts',(0.285612929694432,7.92052654057446,12.09908190091));
#40445=CARTESIAN_POINT('Ctrl Pts',(1.59905942691756,7.87316387198493,12.0594794405123));
#40446=CARTESIAN_POINT('Ctrl Pts',(2.90047126717137,7.49206024510598,12.0198769801146));
#40447=CARTESIAN_POINT('Ctrl Pts',(4.03199033200069,6.82344262828845,11.9802745197169));
#40448=CARTESIAN_POINT('Ctrl Pts',(5.16350939683,6.15482501147092,11.9406720593192));
#40449=CARTESIAN_POINT('Ctrl Pts',(6.12513568623482,5.19869340471483,11.9010695989215));
#40450=CARTESIAN_POINT('Ctrl Pts',(6.80022622936098,4.0710242723093,11.8614671385238));
#40451=CARTESIAN_POINT('Ctrl Pts',(7.47531677248716,2.94335513990372,11.8218646781261));
#40452=CARTESIAN_POINT('Ctrl Pts',(7.86387156933467,1.64414848184864,11.7822622177284));
#40453=CARTESIAN_POINT('Ctrl Pts',(7.91875985925233,0.330994952927389,11.7426597573307));
#40454=CARTESIAN_POINT('Ctrl Pts',(7.97364814916999,-0.982158575993826,
11.703057296933));
#40455=CARTESIAN_POINT('Ctrl Pts',(7.69486993215784,-2.30925897578126,11.6634548365353));
#40456=CARTESIAN_POINT('Ctrl Pts',(7.11624033511875,-3.48933215259594,11.6238523761376));
#40457=CARTESIAN_POINT('Ctrl Pts',(6.53761073807967,-4.66940532941062,11.5842499157399));
#40458=CARTESIAN_POINT('Ctrl Pts',(5.65912976101366,-5.70245128325254,11.5446474553421));
#40459=CARTESIAN_POINT('Ctrl Pts',(4.58735504055451,-6.46316401678891,11.5050449949444));
#40460=CARTESIAN_POINT('Ctrl Pts',(3.51558032009535,-7.22387675032529,11.4654425345467));
#40461=CARTESIAN_POINT('Ctrl Pts',(2.25051185624305,-7.71225626355612,11.425840074149));
#40462=CARTESIAN_POINT('Ctrl Pts',(0.945599418880597,-7.86906329331735,
11.3862376137513));
#40463=CARTESIAN_POINT('Ctrl Pts',(-0.35931301848186,-8.02587032307857,
11.3466351533536));
#40464=CARTESIAN_POINT('Ctrl Pts',(-1.70406942935446,-7.85110486937019,
11.3070326929559));
#40465=CARTESIAN_POINT('Ctrl Pts',(-2.92555408614859,-7.36596556233821,
11.2674302325582));
#40466=CARTESIAN_POINT('Ctrl Pts',(-4.14703874294271,-6.88082625530622,
11.2278277721605));
#40467=CARTESIAN_POINT('Ctrl Pts',(-5.24525164565834,-6.08531309495062,
11.1882253117628));
#40468=CARTESIAN_POINT('Ctrl Pts',(-6.08698220336153,-5.07591991973112,
11.1486228513651));
#40469=CARTESIAN_POINT('Ctrl Pts',(-6.92871276106471,-4.06652674451163,
11.1090203909674));
#40470=CARTESIAN_POINT('Ctrl Pts',(-7.51396097375545,-2.84325355442823,
11.0694179305697));
#40471=CARTESIAN_POINT('Ctrl Pts',(-7.77173763685142,-1.55448045341163,
11.029815470172));
#40472=CARTESIAN_POINT('Ctrl Pts',(-7.87399277178087,-1.04324849876091,
11.014105921903));
#40473=CARTESIAN_POINT('Ctrl Pts',(-7.92471832321012,-0.521709746057469,
10.9983963736341));
#40474=CARTESIAN_POINT('Ctrl Pts',(-7.92444197974487,-0.000117952357666096,
10.9826868253652));
#40475=CARTESIAN_POINT('Ctrl Pts',(-7.92450147625162,-0.000141486819805631,
10.7673131746348));
#40476=CARTESIAN_POINT('Ctrl Pts',(-7.92481514216503,-0.488851138422702,
10.7820326792812));
#40477=CARTESIAN_POINT('Ctrl Pts',(-7.88031944032983,-0.977504363908973,
10.7967521839277));
#40478=CARTESIAN_POINT('Ctrl Pts',(-7.7904753919032,-1.45767247988534,10.8114716885741));
#40479=CARTESIAN_POINT('Ctrl Pts',(-7.54875221879049,-2.74955282871158,
10.8510741489718));
#40480=CARTESIAN_POINT('Ctrl Pts',(-6.97876795817564,-3.98001238748372,
10.8906766093695));
#40481=CARTESIAN_POINT('Ctrl Pts',(-6.14966033378676,-4.9997993629268,10.9302790697672));
#40482=CARTESIAN_POINT('Ctrl Pts',(-5.32055270939788,-6.01958633836991,
10.9698815301649));
#40483=CARTESIAN_POINT('Ctrl Pts',(-4.23232172123497,-6.82870073048396,
11.0094839905627));
#40484=CARTESIAN_POINT('Ctrl Pts',(-3.01696717808935,-7.32899890413347,
11.0490864509604));
#40485=CARTESIAN_POINT('Ctrl Pts',(-1.80161263494375,-7.82929707778297,
11.0886889113581));
#40486=CARTESIAN_POINT('Ctrl Pts',(-0.459134536815433,-8.02077903296795,
11.1282913717558));
#40487=CARTESIAN_POINT('Ctrl Pts',(0.847627742874828,-7.88021846778281,
11.1678938321535));
#40488=CARTESIAN_POINT('Ctrl Pts',(2.15439002256511,-7.73965790259767,11.2074962925512));
#40489=CARTESIAN_POINT('Ctrl Pts',(3.42543648381735,-7.26705481704241,11.2470987529489));
#40490=CARTESIAN_POINT('Ctrl Pts',(4.50659223942145,-6.51973483188231,11.2867012133466));
#40491=CARTESIAN_POINT('Ctrl Pts',(5.58774799502555,-5.77241484672221,11.3263036737443));
#40492=CARTESIAN_POINT('Ctrl Pts',(6.47901304498153,-4.75037796195727,11.365906134142));
#40493=CARTESIAN_POINT('Ctrl Pts',(7.07227907641263,-3.57759480038614,11.4055085945397));
#40494=CARTESIAN_POINT('Ctrl Pts',(7.66554510784373,-2.40481163881498,11.4451110549374));
#40495=CARTESIAN_POINT('Ctrl Pts',(7.96081212074994,-1.08128220043768,11.4847135153351));
#40496=CARTESIAN_POINT('Ctrl Pts',(7.92226493460879,0.232452568277466,11.5243159757329));
#40497=CARTESIAN_POINT('Ctrl Pts',(7.88371774846763,1.54618733699257,11.5639184361306));
#40498=CARTESIAN_POINT('Ctrl Pts',(7.5113563632791,2.85012743604553,11.6035208965283));
#40499=CARTESIAN_POINT('Ctrl Pts',(6.85034732205659,3.98610805890958,11.643123356926));
#40500=CARTESIAN_POINT('Ctrl Pts',(6.18933828083405,5.12208868177365,11.6827258173237));
#40501=CARTESIAN_POINT('Ctrl Pts',(5.23968158357755,6.09010982844884,11.7223282777214));
#40502=CARTESIAN_POINT('Ctrl Pts',(4.11656830979056,6.77275285551553,11.7619307381191));
#40503=CARTESIAN_POINT('Ctrl Pts',(2.99345503600359,7.45539588258221,11.8015331985168));
#40504=CARTESIAN_POINT('Ctrl Pts',(1.69688518568615,7.85266079004038,11.8411356589145));
#40505=CARTESIAN_POINT('Ctrl Pts',(0.384129572232522,7.91636029760581,11.8807381193122));
#40506=CARTESIAN_POINT('Ctrl Pts',(-0.928626041221122,7.98005980517125,
11.9203405797099));
#40507=CARTESIAN_POINT('Ctrl Pts',(-2.25756741781097,7.71019391284396,11.9599430401076));
#40508=CARTESIAN_POINT('Ctrl Pts',(-3.44149715658974,7.1394967057732,11.9995455005053));
#40509=CARTESIAN_POINT('Ctrl Pts',(-4.62542689536849,6.56879949870245,12.0391479609031));
#40510=CARTESIAN_POINT('Ctrl Pts',(-5.66434499633619,5.69727097688824,12.0787504213008));
#40511=CARTESIAN_POINT('Ctrl Pts',(-6.43223318442422,4.63062546034554,12.1183528816985));
#40512=CARTESIAN_POINT('Ctrl Pts',(-7.20012137251226,3.56397994380283,12.1579553420962));
#40513=CARTESIAN_POINT('Ctrl Pts',(-7.69697964772063,2.3022174325316,12.1975578024939));
#40514=CARTESIAN_POINT('Ctrl Pts',(-7.86254029535431,0.99838669160568,12.2371602628916));
#40515=CARTESIAN_POINT('Ctrl Pts',(-7.90455902808044,0.667478856887011,
12.2472112334727));
#40516=CARTESIAN_POINT('Ctrl Pts',(-7.92523797810166,0.333861292895049,
12.2572622040537));
#40517=CARTESIAN_POINT('Ctrl Pts',(-7.92490579193458,0.000202837437923534,
12.2673131746348));
#40518=CARTESIAN_POINT('Origin',(0.,0.,0.));
#40519=CARTESIAN_POINT('',(-7.92471172241511,-8.01339879119567E-6,13.9826868253652));
#40520=CARTESIAN_POINT('',(-7.92543898861653,-0.000149382597450273,13.7673131746348));
#40521=CARTESIAN_POINT('',(-7.925,-9.70532588324277E-16,0.));
#40522=CARTESIAN_POINT('Ctrl Pts',(-7.92471172241511,-8.01339879119567E-6,
13.9826868253652));
#40523=CARTESIAN_POINT('Ctrl Pts',(-7.92378999755476,1.12304350898084,13.9488554231791));
#40524=CARTESIAN_POINT('Ctrl Pts',(-7.68313346855731,2.24612491945329,13.915024020993));
#40525=CARTESIAN_POINT('Ctrl Pts',(-7.22018928937337,3.2688662481316,13.8811926188069));
#40526=CARTESIAN_POINT('Ctrl Pts',(-6.67827475619426,4.46606974396276,13.8415901584092));
#40527=CARTESIAN_POINT('Ctrl Pts',(-5.83176739335577,5.52578080862963,13.8019876980115));
#40528=CARTESIAN_POINT('Ctrl Pts',(-4.78383316777566,6.31911976065525,13.7623852376138));
#40529=CARTESIAN_POINT('Ctrl Pts',(-3.73589894219555,7.11245871268087,13.722782777216));
#40530=CARTESIAN_POINT('Ctrl Pts',(-2.48653785387384,7.63942555206525,13.6831803168183));
#40531=CARTESIAN_POINT('Ctrl Pts',(-1.18708642259866,7.83625609708293,13.6435778564206));
#40532=CARTESIAN_POINT('Ctrl Pts',(0.112365008676521,8.03308664210061,13.6039753960229));
#40533=CARTESIAN_POINT('Ctrl Pts',(1.46190678290515,7.89978089275159,13.5643729356252));
#40534=CARTESIAN_POINT('Ctrl Pts',(2.69774006309914,7.45243063459268,13.5247704752275));
#40535=CARTESIAN_POINT('Ctrl Pts',(3.93357334329316,7.00508037643375,13.4851680148298));
#40536=CARTESIAN_POINT('Ctrl Pts',(5.05569812945251,6.2436856094649,13.4455655544321));
#40537=CARTESIAN_POINT('Ctrl Pts',(5.92805547631356,5.26064132126167,13.4059630940344));
#40538=CARTESIAN_POINT('Ctrl Pts',(6.80041282317456,4.27759703305851,13.3663606336367));
#40539=CARTESIAN_POINT('Ctrl Pts',(7.42300273073732,3.07290322362089,13.326758173239));
#40540=CARTESIAN_POINT('Ctrl Pts',(7.72027995804387,1.79266613693959,13.2871557128413));
#40541=CARTESIAN_POINT('Ctrl Pts',(8.01755718535043,0.512429050258223,13.2475532524436));
#40542=CARTESIAN_POINT('Ctrl Pts',(7.98952173240083,-0.843351313666888,
13.2079507920459));
#40543=CARTESIAN_POINT('Ctrl Pts',(7.63958780389822,-2.11021171993848,13.1683483316481));
#40544=CARTESIAN_POINT('Ctrl Pts',(7.2896538753956,-3.3770721262101,13.1287458712504));
#40545=CARTESIAN_POINT('Ctrl Pts',(6.61782147133996,-4.55501257482813,13.0891434108527));
#40546=CARTESIAN_POINT('Ctrl Pts',(5.70557531991554,-5.50115698955477,13.049540950455));
#40547=CARTESIAN_POINT('Ctrl Pts',(4.79332916849116,-6.44730140428135,13.0099384900573));
#40548=CARTESIAN_POINT('Ctrl Pts',(3.64066926969804,-7.16164978511656,12.9703360296596));
#40549=CARTESIAN_POINT('Ctrl Pts',(2.38741404450885,-7.55755069275904,12.9307335692619));
#40550=CARTESIAN_POINT('Ctrl Pts',(1.13415881931962,-7.95345160040152,12.8911311088642));
#40551=CARTESIAN_POINT('Ctrl Pts',(-0.219691732265668,-8.03090503485126,
12.8515286484665));
#40552=CARTESIAN_POINT('Ctrl Pts',(-1.50992059338783,-7.78051745619478,
12.8119261880688));
#40553=CARTESIAN_POINT('Ctrl Pts',(-2.80014945451003,-7.5301298775383,12.7723237276711));
#40554=CARTESIAN_POINT('Ctrl Pts',(-4.0267566251691,-6.95190128577559,12.7327212672734));
#40555=CARTESIAN_POINT('Ctrl Pts',(-5.04095667418956,-6.11596871951397,
12.6931188068757));
#40556=CARTESIAN_POINT('Ctrl Pts',(-6.05515672321,-5.28003615325238,12.653516346478));
#40557=CARTESIAN_POINT('Ctrl Pts',(-6.85694965059184,-4.18639961249191,
12.6139138860802));
#40558=CARTESIAN_POINT('Ctrl Pts',(-7.34908036888381,-2.96771494548212,
12.5743114256825));
#40559=CARTESIAN_POINT('Ctrl Pts',(-7.72861302009243,-2.02786176122485,
12.5437698922434));
#40560=CARTESIAN_POINT('Ctrl Pts',(-7.92397284707874,-1.01363570905215,
12.5132283588043));
#40561=CARTESIAN_POINT('Ctrl Pts',(-7.92500786703747,0.000202977126703835,
12.4826868253652));
#40562=CARTESIAN_POINT('Ctrl Pts',(-7.92490579193458,0.000202837437923534,
12.2673131746348));
#40563=CARTESIAN_POINT('Ctrl Pts',(-7.92392911052309,-0.980807341544247,
12.2968646644514));
#40564=CARTESIAN_POINT('Ctrl Pts',(-7.74132045846664,-1.96217100913998,
12.3264161542681));
#40565=CARTESIAN_POINT('Ctrl Pts',(-7.38543284899398,-2.87605590061804,
12.3559676440847));
#40566=CARTESIAN_POINT('Ctrl Pts',(-6.908501734941,-4.10076878133526,12.3955701044824));
#40567=CARTESIAN_POINT('Ctrl Pts',(-6.12037648677604,-5.20429557218911,
12.4351725648801));
#40568=CARTESIAN_POINT('Ctrl Pts',(-5.11665481600748,-6.05278112504653,
12.4747750252778));
#40569=CARTESIAN_POINT('Ctrl Pts',(-4.11293314523893,-6.90126667790396,
12.5143774856755));
#40570=CARTESIAN_POINT('Ctrl Pts',(-2.89361505186678,-7.49471099276496,
12.5539799460733));
#40571=CARTESIAN_POINT('Ctrl Pts',(-1.60660087812754,-7.76113068811402,
12.593582406471));
#40572=CARTESIAN_POINT('Ctrl Pts',(-0.319586704388297,-8.02755038346307,
12.6331848668687));
#40573=CARTESIAN_POINT('Ctrl Pts',(1.03512354971804,-7.96694545930018,12.6727873272664));
#40574=CARTESIAN_POINT('Ctrl Pts',(2.29320674430343,-7.58666716612938,12.7123897876641));
#40575=CARTESIAN_POINT('Ctrl Pts',(3.55128993888883,-7.20638887295857,12.7519922480618));
#40576=CARTESIAN_POINT('Ctrl Pts',(4.71274607395329,-6.50643721077984,12.7915947084595));
#40577=CARTESIAN_POINT('Ctrl Pts',(5.63669337513792,-5.5717146010451,12.8311971688572));
#40578=CARTESIAN_POINT('Ctrl Pts',(6.56064067632253,-4.6369919913104,12.8707996292549));
#40579=CARTESIAN_POINT('Ctrl Pts',(7.24707914362734,-3.46749843401971,12.9104020896526));
#40580=CARTESIAN_POINT('Ctrl Pts',(7.61274530193707,-2.20509076394141,12.9500045500503));
#40581=CARTESIAN_POINT('Ctrl Pts',(7.97841146024682,-0.942683093863061,
12.989607010448));
#40582=CARTESIAN_POINT('Ctrl Pts',(8.02330530956146,0.412638689002901,13.0292094708457));
#40583=CARTESIAN_POINT('Ctrl Pts',(7.74198159896325,1.69647744267076,13.0688119312434));
#40584=CARTESIAN_POINT('Ctrl Pts',(7.46065788836505,2.98031619633858,13.1084143916412));
#40585=CARTESIAN_POINT('Ctrl Pts',(6.85311661785402,4.1926719208083,13.1480168520389));
#40586=CARTESIAN_POINT('Ctrl Pts',(5.99305056654226,5.18648850098789,13.1876193124366));
#40587=CARTESIAN_POINT('Ctrl Pts',(5.13298451523049,6.18030508116749,13.2272217728343));
#40588=CARTESIAN_POINT('Ctrl Pts',(4.02039368311798,6.95558251705697,13.266824233232));
#40589=CARTESIAN_POINT('Ctrl Pts',(2.79023368812278,7.41828205099748,13.3064266936297));
#40590=CARTESIAN_POINT('Ctrl Pts',(1.56007369312757,7.88098158493798,13.3460291540274));
#40591=CARTESIAN_POINT('Ctrl Pts',(0.212344535249671,8.03110321692952,13.3856316144251));
#40592=CARTESIAN_POINT('Ctrl Pts',(-1.08947946657793,7.85043650322858,13.4252340748228));
#40593=CARTESIAN_POINT('Ctrl Pts',(-2.39130346840553,7.66976978952763,13.4648365352205));
#40594=CARTESIAN_POINT('Ctrl Pts',(-3.64722231418283,7.15831473013422,13.5044389956182));
#40595=CARTESIAN_POINT('Ctrl Pts',(-4.70489215064052,6.37811165393581,13.5440414560159));
#40596=CARTESIAN_POINT('Ctrl Pts',(-5.7625619870982,5.59790857773741,13.5836439164136));
#40597=CARTESIAN_POINT('Ctrl Pts',(-6.62198281423625,4.54895748473401,13.6232463768114));
#40598=CARTESIAN_POINT('Ctrl Pts',(-7.17891660675418,3.35848959671542,13.6628488372091));
#40599=CARTESIAN_POINT('Ctrl Pts',(-7.66861446088681,2.31174117166319,13.6976702830176));
#40600=CARTESIAN_POINT('Ctrl Pts',(-7.92445227138459,1.15558268908939,13.7324917288262));
#40601=CARTESIAN_POINT('Ctrl Pts',(-7.92543898861653,-0.000149382597450273,
13.7673131746348));
#40602=CARTESIAN_POINT('Origin',(0.,0.,-2.77281266907387));
#40603=CARTESIAN_POINT('',(-7.06850701680182,0.000181040229527252,12.9771873309261));
#40604=CARTESIAN_POINT('',(-7.06889154461022,-0.000133237967543387,13.2728126690739));
#40605=CARTESIAN_POINT('',(-7.0685,-3.68825033525048E-13,-2.77281266907387));
#40606=CARTESIAN_POINT('',(2.93403320825987,6.43108807842,14.));
#40607=CARTESIAN_POINT('Ctrl Pts',(-7.06850701680181,0.000181040229526898,
12.9771873309261));
#40608=CARTESIAN_POINT('Ctrl Pts',(-7.06758385735974,-0.904086310338917,
13.0077288643652));
#40609=CARTESIAN_POINT('Ctrl Pts',(-6.66739692335297,-2.98168855062559,
13.077872858202));
#40610=CARTESIAN_POINT('Ctrl Pts',(-4.68560277486572,-5.6848334937073,13.1876193124366));
#40611=CARTESIAN_POINT('Ctrl Pts',(-1.40348058465622,-7.23204187258727,
13.3064266936297));
#40612=CARTESIAN_POINT('Ctrl Pts',(2.21911599220716,-7.02479407394702,13.4252340748228));
#40613=CARTESIAN_POINT('Ctrl Pts',(5.30337207849841,-5.11336005630641,13.5440414560159));
#40614=CARTESIAN_POINT('Ctrl Pts',(7.10104299890235,-1.96145896063838,13.6628488372091));
#40615=CARTESIAN_POINT('Ctrl Pts',(7.1760595033216,1.66630135572941,13.7816562184022));
#40616=CARTESIAN_POINT('Ctrl Pts',(5.60022245538124,4.71550133998197,13.8940399393325));
#40617=CARTESIAN_POINT('Ctrl Pts',(3.82727142929074,6.0224930120962,13.9668211998651));
#40618=CARTESIAN_POINT('Ctrl Pts',(2.93403320825987,6.43108807842,14.));
#40619=CARTESIAN_POINT('',(7.03625248964568,-0.674420604634066,14.));
#40620=CARTESIAN_POINT('Origin',(0.,0.,14.));
#40621=CARTESIAN_POINT('Ctrl Pts',(-7.06889154461022,-0.000133237967543647,
13.2728126690739));
#40622=CARTESIAN_POINT('Ctrl Pts',(-7.06901237995171,-0.141666470630141,
13.277593683663));
#40623=CARTESIAN_POINT('Ctrl Pts',(-7.03035435797223,-1.4554918851001,13.3219771586498));
#40624=CARTESIAN_POINT('Ctrl Pts',(-6.25050664162124,-3.89909682044781,
13.4059630940344));
#40625=CARTESIAN_POINT('Ctrl Pts',(-3.63108720070629,-6.40999851148318,
13.5247704752275));
#40626=CARTESIAN_POINT('Ctrl Pts',(-0.130578947762305,-7.3657578324409,
13.6435778564207));
#40627=CARTESIAN_POINT('Ctrl Pts',(3.40120320632095,-6.5348310696329,13.7623852376137));
#40628=CARTESIAN_POINT('Ctrl Pts',(6.10869718244117,-4.11816204547854,13.8811926188069));
#40629=CARTESIAN_POINT('Ctrl Pts',(6.9243752846715,-1.84163918696265,13.9603975396023));
#40630=CARTESIAN_POINT('Ctrl Pts',(7.03625248964568,-0.674420604634066,
14.));
#40631=CARTESIAN_POINT('Origin',(0.,0.,-2.77281266907387));
#40632=CARTESIAN_POINT('',(-7.06800228818001,-0.000105204573031335,11.4771873309261));
#40633=CARTESIAN_POINT('',(-7.06841597353811,0.000180915637408435,11.7728126690739));
#40634=CARTESIAN_POINT('',(-7.0685,-3.68825033525048E-13,-2.77281266907387));
#40635=CARTESIAN_POINT('Ctrl Pts',(-7.06800228818001,-0.000105204573031432,
11.4771873309261));
#40636=CARTESIAN_POINT('Ctrl Pts',(-7.06824876562911,-0.465325594953699,
11.492896879195));
#40637=CARTESIAN_POINT('Ctrl Pts',(-6.90895070021522,-2.10316120251506,
11.5482088878617));
#40638=CARTESIAN_POINT('Ctrl Pts',(-5.65789011484937,-4.71810105207384,
11.643123356926));
#40639=CARTESIAN_POINT('Ctrl Pts',(-2.71932182355139,-6.84671358480829,
11.7619307381191));
#40640=CARTESIAN_POINT('Ctrl Pts',(0.878940898310958,-7.31434624457016,
11.8807381193122));
#40641=CARTESIAN_POINT('Ctrl Pts',(4.26397677341757,-6.00755359247974,11.9995455005054));
#40642=CARTESIAN_POINT('Ctrl Pts',(6.61459233924385,-3.24335725504188,12.1183528816985));
#40643=CARTESIAN_POINT('Ctrl Pts',(7.36053952925658,0.307661991354685,12.2371602628916));
#40644=CARTESIAN_POINT('Ctrl Pts',(6.32085514508631,3.78404392036229,12.3559676440847));
#40645=CARTESIAN_POINT('Ctrl Pts',(3.74776160818102,6.3424349345032,12.4747750252778));
#40646=CARTESIAN_POINT('Ctrl Pts',(0.265479112470959,7.36218168021696,12.593582406471));
#40647=CARTESIAN_POINT('Ctrl Pts',(-3.28120740049152,6.59589842189123,12.7123897876641));
#40648=CARTESIAN_POINT('Ctrl Pts',(-6.03188862411031,4.22948193287789,12.8311971688572));
#40649=CARTESIAN_POINT('Ctrl Pts',(-6.98832057332378,1.70910717488751,12.9194630166112));
#40650=CARTESIAN_POINT('Ctrl Pts',(-7.06878089565903,0.268455075352352,
12.9681264039675));
#40651=CARTESIAN_POINT('Ctrl Pts',(-7.06850701680181,0.000181040229526898,
12.9771873309261));
#40652=CARTESIAN_POINT('Ctrl Pts',(-7.06841597353811,0.000180915637408539,
11.7728126690739));
#40653=CARTESIAN_POINT('Ctrl Pts',(-7.06754484766335,-0.874805891950531,
11.8023641588905));
#40654=CARTESIAN_POINT('Ctrl Pts',(-6.68640271942718,-2.92311539223316,
11.8715181091049));
#40655=CARTESIAN_POINT('Ctrl Pts',(-4.75596440127724,-5.62609998399613,
11.9802745197169));
#40656=CARTESIAN_POINT('Ctrl Pts',(-1.49334612632416,-7.21402218195007,
12.09908190091));
#40657=CARTESIAN_POINT('Ctrl Pts',(2.13155081922184,-7.05185717004641,12.2178892821032));
#40658=CARTESIAN_POINT('Ctrl Pts',(5.23934363589174,-5.17894550161347,12.3366966632963));
#40659=CARTESIAN_POINT('Ctrl Pts',(7.07609706408506,-2.04964636860042,12.4555040444894));
#40660=CARTESIAN_POINT('Ctrl Pts',(7.19622280814078,1.5768868890101,12.5743114256825));
#40661=CARTESIAN_POINT('Ctrl Pts',(5.57058035869953,4.82087544613853,12.6931188068757));
#40662=CARTESIAN_POINT('Ctrl Pts',(2.5935399939851,6.89534177632834,12.8119261880688));
#40663=CARTESIAN_POINT('Ctrl Pts',(-1.01267712366536,7.29703316651084,12.9307335692619));
#40664=CARTESIAN_POINT('Ctrl Pts',(-4.37323069894997,5.92849559402285,13.049540950455));
#40665=CARTESIAN_POINT('Ctrl Pts',(-6.58030514877926,3.23468938944454,13.163567317059));
#40666=CARTESIAN_POINT('Ctrl Pts',(-7.06801146754352,1.03069226975728,13.2379912232653));
#40667=CARTESIAN_POINT('Ctrl Pts',(-7.06889154461022,-0.000133237967543647,
13.2728126690739));
#40668=CARTESIAN_POINT('Origin',(0.,0.,-2.77281266907387));
#40669=CARTESIAN_POINT('',(-7.0690926972794,-2.72305532282471E-5,9.97718733092612));
#40670=CARTESIAN_POINT('',(-7.06805535455957,-0.000126195531622297,10.2728126690739));
#40671=CARTESIAN_POINT('',(-7.0685,-3.68825033525048E-13,-2.77281266907387));
#40672=CARTESIAN_POINT('Ctrl Pts',(-7.0690926972794,-2.72305532283707E-5,
9.97718733092612));
#40673=CARTESIAN_POINT('Ctrl Pts',(-7.06909837164777,-0.0260037119360697,
9.97806489402483));
#40674=CARTESIAN_POINT('Ctrl Pts',(-7.0626311268876,-1.22423787807622,10.0185449175213));
#40675=CARTESIAN_POINT('Ctrl Pts',(-6.43419630013248,-3.58794036486512,
10.0986274014154));
#40676=CARTESIAN_POINT('Ctrl Pts',(-3.94096871160376,-6.22422394396494,
10.2174347826085));
#40677=CARTESIAN_POINT('Ctrl Pts',(-0.491681018131546,-7.35054065133146,
10.3362421638016));
#40678=CARTESIAN_POINT('Ctrl Pts',(3.07688613178757,-6.69365145660272,10.4550495449948));
#40679=CARTESIAN_POINT('Ctrl Pts',(5.8990154656956,-4.41291452737873,10.5738569261879));
#40680=CARTESIAN_POINT('Ctrl Pts',(7.2900719447016,-1.06162570218753,10.692664307381));
#40681=CARTESIAN_POINT('Ctrl Pts',(6.91259193977638,2.54720842582524,10.8114716885741));
#40682=CARTESIAN_POINT('Ctrl Pts',(4.85815028937904,5.53810200847668,10.9302790697673));
#40683=CARTESIAN_POINT('Ctrl Pts',(1.62514468290704,7.18547860967203,11.0490864509604));
#40684=CARTESIAN_POINT('Ctrl Pts',(-2.00211322794815,7.08969256829738,11.1678938321535));
#40685=CARTESIAN_POINT('Ctrl Pts',(-5.14366807368819,5.27398111849169,11.2867012133466));
#40686=CARTESIAN_POINT('Ctrl Pts',(-6.78699198309204,2.58809019405032,11.3897990462708));
#40687=CARTESIAN_POINT('Ctrl Pts',(-7.06762741654575,0.707456191694836,
11.4532944187973));
#40688=CARTESIAN_POINT('Ctrl Pts',(-7.06800228818001,-0.000105204573031432,
11.4771873309261));
#40689=CARTESIAN_POINT('Ctrl Pts',(-7.06805535455957,-0.00012619553162195,
10.2728126690739));
#40690=CARTESIAN_POINT('Ctrl Pts',(-7.06833512080673,-0.436018204661516,
10.2875321737203));
#40691=CARTESIAN_POINT('Ctrl Pts',(-6.92187198456732,-2.0444810670586,10.3418541387645));
#40692=CARTESIAN_POINT('Ctrl Pts',(-5.71614985062563,-4.64734649237981,
10.4357785642063));
#40693=CARTESIAN_POINT('Ctrl Pts',(-2.8042908954851,-6.81235283206109,10.5545859453995));
#40694=CARTESIAN_POINT('Ctrl Pts',(0.78787557894517,-7.32471505296642,10.6733933265926));
#40695=CARTESIAN_POINT('Ctrl Pts',(4.18890721731539,-6.0601365380463,10.7922007077857));
#40696=CARTESIAN_POINT('Ctrl Pts',(6.57373005855721,-3.32539796897586,10.9110080889788));
#40697=CARTESIAN_POINT('Ctrl Pts',(7.36379752129319,0.216066195757339,11.0298154701719));
#40698=CARTESIAN_POINT('Ctrl Pts',(6.36744302872343,3.70511373777206,11.1486228513651));
#40699=CARTESIAN_POINT('Ctrl Pts',(3.82637740176148,6.29531846027314,11.2674302325582));
#40700=CARTESIAN_POINT('Ctrl Pts',(0.357050971363174,7.3583091221159,11.3862376137513));
#40701=CARTESIAN_POINT('Ctrl Pts',(-3.1988943108167,6.63620928870937,11.5050449949444));
#40702=CARTESIAN_POINT('Ctrl Pts',(-5.97880318022623,4.30419691403035,11.6238523761376));
#40703=CARTESIAN_POINT('Ctrl Pts',(-6.97759561010622,1.76778178833764,11.7131082675141));
#40704=CARTESIAN_POINT('Ctrl Pts',(-7.06871225844943,0.297778996697315,
11.7627616984928));
#40705=CARTESIAN_POINT('Ctrl Pts',(-7.06841597353811,0.000180915637408539,
11.7728126690739));
#40706=CARTESIAN_POINT('Origin',(0.,0.,-2.77281266907387));
#40707=CARTESIAN_POINT('',(-7.06810297343219,0.000140531831294521,8.47718733092612));
#40708=CARTESIAN_POINT('',(-7.06910150038349,3.50688967443413E-6,8.77281266907389));
#40709=CARTESIAN_POINT('',(-7.0685,-3.68825033525048E-13,-2.77281266907387));
#40710=CARTESIAN_POINT('Ctrl Pts',(-7.06810297343219,0.000140531831294526,
8.47718733092612));
#40711=CARTESIAN_POINT('Ctrl Pts',(-7.0675551177651,-0.759365934494961,
8.50283536925235));
#40712=CARTESIAN_POINT('Ctrl Pts',(-6.75724147934998,-2.69204332921662,
8.56808586797629));
#40713=CARTESIAN_POINT('Ctrl Pts',(-5.02610585121275,-5.3861357263693,8.67293882709792));
#40714=CARTESIAN_POINT('Ctrl Pts',(-1.84527177852238,-7.1321224157929,8.79174620829105));
#40715=CARTESIAN_POINT('Ctrl Pts',(1.78321637602583,-7.14789041932932,8.91055358948417));
#40716=CARTESIAN_POINT('Ctrl Pts',(4.97910479168735,-5.42961449495844,9.02936097067729));
#40717=CARTESIAN_POINT('Ctrl Pts',(6.96708626922742,-2.39414013950925,9.14816835187041));
#40718=CARTESIAN_POINT('Ctrl Pts',(7.26488603837279,1.2221411292984,9.26697573306353));
#40719=CARTESIAN_POINT('Ctrl Pts',(5.80025930364893,4.54193682264524,9.38578311425666));
#40720=CARTESIAN_POINT('Ctrl Pts',(2.92851748521003,6.75988043010273,9.50459049544978));
#40721=CARTESIAN_POINT('Ctrl Pts',(-0.653668627291716,7.33790947178836,
9.6233978766429));
#40722=CARTESIAN_POINT('Ctrl Pts',(-4.07727786640525,6.1357968749453,9.74220525783602));
#40723=CARTESIAN_POINT('Ctrl Pts',(-6.49377691438734,3.46504353643401,9.86013507593044));
#40724=CARTESIAN_POINT('Ctrl Pts',(-7.06884230009088,1.14625680897868,9.93846243362713));
#40725=CARTESIAN_POINT('Ctrl Pts',(-7.0690926972794,-2.72305532283707E-5,
9.97718733092612));
#40726=CARTESIAN_POINT('Ctrl Pts',(-7.0691014299727,3.50647916297852E-6,
8.77281266907389));
#40727=CARTESIAN_POINT('Ctrl Pts',(-7.06906675364277,-1.16892331971989,
8.81230264894784));
#40728=CARTESIAN_POINT('Ctrl Pts',(-6.47600648320203,-3.51014035758656,
8.8913950892195));
#40729=CARTESIAN_POINT('Ctrl Pts',(-4.01809889103379,-6.17471293558617,
9.01008998988887));
#40730=CARTESIAN_POINT('Ctrl Pts',(-0.583090560721348,-7.34385484149978,
9.12889737108199));
#40731=CARTESIAN_POINT('Ctrl Pts',(2.99337274258629,-6.73141279071218,9.24770475227512));
#40732=CARTESIAN_POINT('Ctrl Pts',(5.84365817749679,-4.48596228691204,9.36651213346823));
#40733=CARTESIAN_POINT('Ctrl Pts',(7.27630017007747,-1.15223885108631,9.48531951466136));
#40734=CARTESIAN_POINT('Ctrl Pts',(6.94374664518998,2.46101220282127,9.60412689585448));
#40735=CARTESIAN_POINT('Ctrl Pts',(4.92667349274102,5.47723350159046,9.72293427704761));
#40736=CARTESIAN_POINT('Ctrl Pts',(1.71441298378659,7.16470422669678,9.84174165824072));
#40737=CARTESIAN_POINT('Ctrl Pts',(-1.91375589114147,7.11405207488272,9.96054903943386));
#40738=CARTESIAN_POINT('Ctrl Pts',(-5.07765676700238,5.33756501520463,10.079356420627));
#40739=CARTESIAN_POINT('Ctrl Pts',(-6.77036891949848,2.646732268931,10.1834442971737));
#40740=CARTESIAN_POINT('Ctrl Pts',(-7.06758241669134,0.736738382185901,
10.2479297133226));
#40741=CARTESIAN_POINT('Ctrl Pts',(-7.06805535455957,-0.00012619553162195,
10.2728126690739));
#40742=CARTESIAN_POINT('Origin',(0.,0.,-2.77281266907387));
#40743=CARTESIAN_POINT('',(-7.06834762154544,-0.000177849683210104,6.97718733092612));
#40744=CARTESIAN_POINT('',(-7.06804242201619,0.000121653731739724,7.27281266907389));
#40745=CARTESIAN_POINT('',(-7.0685,-3.68825033525048E-13,-2.77281266907387));
#40746=CARTESIAN_POINT('Ctrl Pts',(-7.06834762154545,-0.000177849683210204,
6.97718733092612));
#40747=CARTESIAN_POINT('Ctrl Pts',(-7.06865582645895,-0.320438072175684,
6.98800338408215));
#40748=CARTESIAN_POINT('Ctrl Pts',(-6.96904742463227,-1.8131255237446,7.03842189763588));
#40749=CARTESIAN_POINT('Ctrl Pts',(-5.93714558070924,-4.36147915780088,
7.12844287158734));
#40750=CARTESIAN_POINT('Ctrl Pts',(-3.13494485649586,-6.66665724611644,
7.24725025278046));
#40751=CARTESIAN_POINT('Ctrl Pts',(0.427778451839743,-7.35453626591155,
7.36605763397357));
#40752=CARTESIAN_POINT('Ctrl Pts',(3.88672475977586,-6.25824006668105,7.48486501516671));
#40753=CARTESIAN_POINT('Ctrl Pts',(6.40277028527823,-3.64372484751866,7.60367239635982));
#40754=CARTESIAN_POINT('Ctrl Pts',(7.36553445311621,-0.145259458986194,
7.72247977755295));
#40755=CARTESIAN_POINT('Ctrl Pts',(6.54145529447003,3.38844517749906,7.84128715874606));
#40756=CARTESIAN_POINT('Ctrl Pts',(4.13045046018973,6.10012926800615,7.9600945399392));
#40757=CARTESIAN_POINT('Ctrl Pts',(0.71741815768671,7.33195125989582,8.0789019211323));
#40758=CARTESIAN_POINT('Ctrl Pts',(-2.86965634847726,6.78507704688097,8.19770930232544));
#40759=CARTESIAN_POINT('Ctrl Pts',(-5.76056598999791,4.59217568972987,8.31651668351855));
#40760=CARTESIAN_POINT('Ctrl Pts',(-6.93159083568589,1.99913423513499,8.40967602638545));
#40761=CARTESIAN_POINT('Ctrl Pts',(-7.06840104726987,0.413367994389237,
8.46323290885464));
#40762=CARTESIAN_POINT('Ctrl Pts',(-7.06810297343219,0.000140531831294526,
8.47718733092612));
#40763=CARTESIAN_POINT('Ctrl Pts',(-7.06804242201619,0.000121653731739516,
7.27281266907389));
#40764=CARTESIAN_POINT('Ctrl Pts',(-7.06759172593921,-0.730084929063449,
7.29747066377764));
#40765=CARTESIAN_POINT('Ctrl Pts',(-6.77418208262749,-2.63340817566325,
7.36173111887911));
#40766=CARTESIAN_POINT('Ctrl Pts',(-5.09272545443097,-5.32318945565654,
7.46559403437827));
#40767=CARTESIAN_POINT('Ctrl Pts',(-1.9338592434572,-7.10861357519998,7.58440141557141));
#40768=CARTESIAN_POINT('Ctrl Pts',(1.69415194342111,-7.16952214081417,7.70320879676452));
#40769=CARTESIAN_POINT('Ctrl Pts',(4.91116999552812,-5.49113902665435,7.82201617795765));
#40770=CARTESIAN_POINT('Ctrl Pts',(6.93676176518449,-2.48063192515472,7.94082355915077));
#40771=CARTESIAN_POINT('Ctrl Pts',(7.27952840566287,1.13166458200723,8.0596309403439));
#40772=CARTESIAN_POINT('Ctrl Pts',(5.85631637420563,4.46942469007289,8.178438321537));
#40773=CARTESIAN_POINT('Ctrl Pts',(3.01239008261732,6.72292380777671,8.29724570273014));
#40774=CARTESIAN_POINT('Ctrl Pts',(-0.562327592835126,7.34547385900723,
8.41605308392325));
#40775=CARTESIAN_POINT('Ctrl Pts',(-4.00062729170338,6.18604718765547,8.53486046511639));
#40776=CARTESIAN_POINT('Ctrl Pts',(-6.46839400027299,3.52591514252037,8.6536678463095));
#40777=CARTESIAN_POINT('Ctrl Pts',(-7.06828828255705,1.17891875484952,8.73298524762867));
#40778=CARTESIAN_POINT('Ctrl Pts',(-7.06910152874236,0.00333299669573309,
8.77270018855014));
#40779=CARTESIAN_POINT('Ctrl Pts',(-7.0691014299727,3.50647916297852E-6,
8.77281266907389));
#40780=CARTESIAN_POINT('Origin',(0.,0.,-2.77281266907387));
#40781=CARTESIAN_POINT('',(-7.06894407494582,0.000114272372526485,5.47718733092612));
#40782=CARTESIAN_POINT('',(-7.06843645704685,-0.000181328847439488,5.77281266907388));
#40783=CARTESIAN_POINT('',(-7.0685,-3.68825033525048E-13,-2.77281266907387));
#40784=CARTESIAN_POINT('Ctrl Pts',(-7.06894407494582,0.000114272372526512,
5.47718733092612));
#40785=CARTESIAN_POINT('Ctrl Pts',(-7.06813276101183,-1.05333618941605,
5.51277385930966));
#40786=CARTESIAN_POINT('Ctrl Pts',(-6.5638901837095,-3.27986943935765,5.5879628480909));
#40787=CARTESIAN_POINT('Ctrl Pts',(-4.3160277462564,-5.97026821709139,5.70275429726988));
#40788=CARTESIAN_POINT('Ctrl Pts',(-0.942477130941647,-7.30643106777301,
5.82156167846298));
#40789=CARTESIAN_POINT('Ctrl Pts',(2.659713915357,-6.87008878974086,5.94036905965612));
#40790=CARTESIAN_POINT('Ctrl Pts',(5.61667112421129,-4.76709592654876,6.05917644084923));
#40791=CARTESIAN_POINT('Ctrl Pts',(7.21105086102525,-1.50762845892934,6.17798382204236));
#40792=CARTESIAN_POINT('Ctrl Pts',(7.05606424975171,2.11758244086091,6.29679120323547));
#40793=CARTESIAN_POINT('Ctrl Pts',(5.18931029882807,5.22907799836104,6.41559858442861));
#40794=CARTESIAN_POINT('Ctrl Pts',(2.06365456208858,7.0720243169009,6.53440596562172));
#40795=CARTESIAN_POINT('Ctrl Pts',(-1.56263387223831,7.19933146005934,6.65321334681485));
#40796=CARTESIAN_POINT('Ctrl Pts',(-4.80983482498188,5.58011532558766,6.77202072800796));
#40797=CARTESIAN_POINT('Ctrl Pts',(-6.70080011169465,2.87784082925081,6.88001205604507));
#40798=CARTESIAN_POINT('Ctrl Pts',(-7.06752734893528,0.852179387747461,
6.94840092368444));
#40799=CARTESIAN_POINT('Ctrl Pts',(-7.06834762154545,-0.000177849683210204,
6.97718733092612));
#40800=CARTESIAN_POINT('Ctrl Pts',(-7.06843645704685,-0.000181328847439211,
5.77281266907388));
#40801=CARTESIAN_POINT('Ctrl Pts',(-7.0687283062341,-0.291116138498873,
5.78263867860744));
#40802=CARTESIAN_POINT('Ctrl Pts',(-6.98006586361788,-1.7544493646656,5.83206714853871));
#40803=CARTESIAN_POINT('Ctrl Pts',(-5.9909469960723,-4.28727799719992,5.9210980788677));
#40804=CARTESIAN_POINT('Ctrl Pts',(-3.21764169554554,-6.62713968874273,
6.0399054600608));
#40805=CARTESIAN_POINT('Ctrl Pts',(0.336248045567207,-7.35928908162156,
6.15871284125395));
#40806=CARTESIAN_POINT('Ctrl Pts',(3.80856562377858,-6.30611024518239,6.27752022244705));
#40807=CARTESIAN_POINT('Ctrl Pts',(6.35694345102643,-3.72309931313607,6.39632760364018));
#40808=CARTESIAN_POINT('Ctrl Pts',(7.36315729077195,-0.236882347113499,
6.5151349848333));
#40809=CARTESIAN_POINT('Ctrl Pts',(6.58310449221504,3.30680114001436,6.63394236602642));
#40810=CARTESIAN_POINT('Ctrl Pts',(4.20602212243871,6.04827053301837,6.75274974721955));
#40811=CARTESIAN_POINT('Ctrl Pts',(0.808578961688855,7.3224585077511,6.87155712841267));
#40812=CARTESIAN_POINT('Ctrl Pts',(-2.78502157648225,6.8202531737136,6.99036450960579));
#40813=CARTESIAN_POINT('Ctrl Pts',(-5.70298923971021,4.66348713590718,7.10917189079892));
#40814=CARTESIAN_POINT('Ctrl Pts',(-6.91897017189403,2.05781460754039,7.20332127728827));
#40815=CARTESIAN_POINT('Ctrl Pts',(-7.06831557529332,0.442677804675292,
7.25786820337994));
#40816=CARTESIAN_POINT('Ctrl Pts',(-7.06804242201619,0.000121653731739516,
7.27281266907389));
#40817=CARTESIAN_POINT('Origin',(0.,0.,-2.77281266907387));
#40818=CARTESIAN_POINT('',(-7.06790662938871,2.60008083700674E-5,3.97718733092612));
#40819=CARTESIAN_POINT('',(-7.0688699538086,0.000135730005232301,4.27281266907388));
#40820=CARTESIAN_POINT('',(-7.0685,-3.68825033525048E-13,-2.77281266907387));
#40821=CARTESIAN_POINT('Ctrl Pts',(-7.06790662938871,2.60008083700913E-5,
3.97718733092612));
#40822=CARTESIAN_POINT('Ctrl Pts',(-7.06782750266918,-0.614619981437727,
3.99794187413946));
#40823=CARTESIAN_POINT('Ctrl Pts',(-6.83699561128725,-2.40215150421776,
4.05829887775052));
#40824=CARTESIAN_POINT('Ctrl Pts',(-5.34760935712609,-5.06707728913272,
4.15825834175928));
#40825=CARTESIAN_POINT('Ctrl Pts',(-2.28008659912764,-7.00524112296964,
4.2770657229524));
#40826=CARTESIAN_POINT('Ctrl Pts',(1.34057423043783,-7.24396706391966,4.39587310414552));
#40827=CARTESIAN_POINT('Ctrl Pts',(4.63601818231957,-5.72534134385619,4.51468048533865));
#40828=CARTESIAN_POINT('Ctrl Pts',(6.80678636175523,-2.81777527774835,4.63348786653177));
#40829=CARTESIAN_POINT('Ctrl Pts',(7.32626082140389,0.773369554113066,4.75229524772489));
#40830=CARTESIAN_POINT('Ctrl Pts',(6.06841954922959,4.17689864193457,4.87110262891801));
#40831=CARTESIAN_POINT('Ctrl Pts',(3.33840880410428,6.56713215545002,4.98991001011114));
#40832=CARTESIAN_POINT('Ctrl Pts',(-0.201483902833845,7.36421091002734,
5.10871739130425));
#40833=CARTESIAN_POINT('Ctrl Pts',(-3.69249758144563,6.37476742332494,5.22752477249739));
#40834=CARTESIAN_POINT('Ctrl Pts',(-6.28772905939532,3.83883593894067,5.34633215369049));
#40835=CARTESIAN_POINT('Ctrl Pts',(-7.03713150959426,1.41016055953885,5.42955300650008));
#40836=CARTESIAN_POINT('Ctrl Pts',(-7.06903563154741,0.118995928634036,
5.47317139891195));
#40837=CARTESIAN_POINT('Ctrl Pts',(-7.06894407494582,0.000114272372526512,
5.47718733092612));
#40838=CARTESIAN_POINT('Ctrl Pts',(-7.0688699538086,0.000135730005232423,
4.27281266907388));
#40839=CARTESIAN_POINT('Ctrl Pts',(-7.06797279848001,-1.02403807532536,
4.30740915383496));
#40840=CARTESIAN_POINT('Ctrl Pts',(-6.58508986586626,-3.22139801692903,
4.38160809899374));
#40841=CARTESIAN_POINT('Ctrl Pts',(-4.38996945438879,-5.91611077690027,
4.49540950455022));
#40842=CARTESIAN_POINT('Ctrl Pts',(-1.03330302320227,-7.29414034669358,
4.61421688574334));
#40843=CARTESIAN_POINT('Ctrl Pts',(2.57403776474647,-6.90264645774946,4.73302426693647));
#40844=CARTESIAN_POINT('Ctrl Pts',(5.5569293384078,-4.83660364956287,4.85183164812959));
#40845=CARTESIAN_POINT('Ctrl Pts',(7.19173651068846,-1.59722399676838,4.97063902932272));
#40846=CARTESIAN_POINT('Ctrl Pts',(7.08186290362403,2.02963453589456,5.08944641051583));
#40847=CARTESIAN_POINT('Ctrl Pts',(5.25396332723401,5.16411346613359,5.20825379170895));
#40848=CARTESIAN_POINT('Ctrl Pts',(2.15147745047193,7.04580324130137,5.32706117290208));
#40849=CARTESIAN_POINT('Ctrl Pts',(-1.47294653532043,7.21821494824792,5.4458685540952));
#40850=CARTESIAN_POINT('Ctrl Pts',(-4.74004075724321,5.63952233391227,5.56467593528832));
#40851=CARTESIAN_POINT('Ctrl Pts',(-6.68212139988246,2.9364259970353,5.67365730694789));
#40852=CARTESIAN_POINT('Ctrl Pts',(-7.06755204583654,0.881458978407337,
5.74303621820974));
#40853=CARTESIAN_POINT('Ctrl Pts',(-7.06843645704685,-0.000181328847439211,
5.77281266907388));
#40854=CARTESIAN_POINT('Origin',(0.,0.,-2.77281266907387));
#40855=CARTESIAN_POINT('',(-7.06879387608848,-0.000152214530812696,2.47718733092612));
#40856=CARTESIAN_POINT('',(-7.06790105247164,-1.00512679984677E-6,2.77281266907389));
#40857=CARTESIAN_POINT('',(-7.0685,-3.68825033525048E-13,-2.77281266907387));
#40858=CARTESIAN_POINT('Ctrl Pts',(-7.06879387608848,-0.000152214530812871,
2.47718733092612));
#40859=CARTESIAN_POINT('Ctrl Pts',(-7.06896001159515,-0.175485562544569,
2.48310988896927));
#40860=CARTESIAN_POINT('Ctrl Pts',(-7.0198256726627,-1.52313020894557,2.52863490741013));
#40861=CARTESIAN_POINT('Ctrl Pts',(-6.19395711760227,-3.9883697563648,2.61376238624869));
#40862=CARTESIAN_POINT('Ctrl Pts',(-3.53871699613534,-6.46139923806788,
2.73256976744181));
#40863=CARTESIAN_POINT('Ctrl Pts',(-0.0250011063573954,-7.36692425873726,
2.85137714863493));
#40864=CARTESIAN_POINT('Ctrl Pts',(3.49477993190855,-6.48526879308302,2.97018452982806));
#40865=CARTESIAN_POINT('Ctrl Pts',(6.16674412284828,-4.03031822733696,3.08899191102118));
#40866=CARTESIAN_POINT('Ctrl Pts',(7.34268577093533,-0.597631792820449,
3.2077992922143));
#40867=CARTESIAN_POINT('Ctrl Pts',(6.73732707323029,2.98003724789039,3.32660667340742));
#40868=CARTESIAN_POINT('Ctrl Pts',(4.4975251459451,5.83476354722511,3.44541405460054));
#40869=CARTESIAN_POINT('Ctrl Pts',(1.16664519249845,7.27400419887887,3.56422143579367));
#40870=CARTESIAN_POINT('Ctrl Pts',(-2.44725728835037,6.94860632465767,3.68302881698679));
#40871=CARTESIAN_POINT('Ctrl Pts',(-5.46746689033045,4.93750988795068,3.80183619817991));
#40872=CARTESIAN_POINT('Ctrl Pts',(-6.86539920913079,2.28916439736259,3.89988903615969));
#40873=CARTESIAN_POINT('Ctrl Pts',(-7.06797848709435,0.558207236212538,
3.95833941374176));
#40874=CARTESIAN_POINT('Ctrl Pts',(-7.06790662938871,2.60008083700913E-5,
3.97718733092612));
#40875=CARTESIAN_POINT('Ctrl Pts',(-7.06790105247164,-1.00512680008963E-6,
2.77281266907389));
#40876=CARTESIAN_POINT('Ctrl Pts',(-7.06790396260581,-0.585328167239678,
2.79257716866476));
#40877=CARTESIAN_POINT('Ctrl Pts',(-6.8519294853734,-2.34348310332654,2.85194412865334));
#40878=CARTESIAN_POINT('Ctrl Pts',(-5.41023469503032,-5.0001559055375,2.95091354903963));
#40879=CARTESIAN_POINT('Ctrl Pts',(-2.36706189309541,-6.97633259881565,
3.06972093023276));
#40880=CARTESIAN_POINT('Ctrl Pts',(1.25034876951077,-7.26008446848898,3.18852831142588));
#40881=CARTESIAN_POINT('Ctrl Pts',(4.56443081844987,-5.78257467211716,3.307335692619));
#40882=CARTESIAN_POINT('Ctrl Pts',(6.7712038460194,-2.90223999880672,3.42614307381212));
#40883=CARTESIAN_POINT('Ctrl Pts',(7.33531530143303,0.682164176415201,3.54495045500525));
#40884=CARTESIAN_POINT('Ctrl Pts',(6.11991445160226,4.10107859472268,3.66375783619837));
#40885=CARTESIAN_POINT('Ctrl Pts',(3.41985171252147,6.5250910184752,3.78256521739149));
#40886=CARTESIAN_POINT('Ctrl Pts',(-0.109850647279407,7.36614766145199,
3.90137259858461));
#40887=CARTESIAN_POINT('Ctrl Pts',(-3.61290376699451,6.42021221654385,4.02017997977773));
#40888=CARTESIAN_POINT('Ctrl Pts',(-6.2394837636286,3.91676408511378,4.13898736097086));
#40889=CARTESIAN_POINT('Ctrl Pts',(-7.02831730228861,1.46882013834326,4.2231982574029));
#40890=CARTESIAN_POINT('Ctrl Pts',(-7.06899976866546,0.148329662208865,
4.26780669343725));
#40891=CARTESIAN_POINT('Ctrl Pts',(-7.0688699538086,0.000135730005232423,
4.27281266907388));
#40892=CARTESIAN_POINT('Origin',(0.,0.,-2.77281266907387));
#40893=CARTESIAN_POINT('',(-7.0685211611855,0.000181853424906659,0.977187330926116));
#40894=CARTESIAN_POINT('',(-7.06887577069393,-0.000134259091651989,1.27281266907389));
#40895=CARTESIAN_POINT('',(-7.0685,-3.68825033525048E-13,-2.77281266907387));
#40896=CARTESIAN_POINT('Ctrl Pts',(-7.06852116118549,0.000181853424906647,
0.977187330926117));
#40897=CARTESIAN_POINT('Ctrl Pts',(-7.06759165261753,-0.908565991214031,
1.00788036419678));
#40898=CARTESIAN_POINT('Ctrl Pts',(-6.66445125668807,-2.9906520072978,1.07817585786515));
#40899=CARTESIAN_POINT('Ctrl Pts',(-4.67477113205871,-5.69374237749066,
1.18807381193122));
#40900=CARTESIAN_POINT('Ctrl Pts',(-1.38971041869972,-7.23470180222814,
1.30688119312434));
#40901=CARTESIAN_POINT('Ctrl Pts',(2.23248728958399,-7.02055517652312,1.42568857431747));
#40902=CARTESIAN_POINT('Ctrl Pts',(5.31309433455675,-5.10325661323295,1.54449595551059));
#40903=CARTESIAN_POINT('Ctrl Pts',(7.10477015790912,-1.94793192835274,1.66330333670371));
#40904=CARTESIAN_POINT('Ctrl Pts',(7.17286283343114,1.67995141886001,1.78211071789683));
#40905=CARTESIAN_POINT('Ctrl Pts',(5.50085338730159,4.90028675314958,1.90091809908995));
#40906=CARTESIAN_POINT('Ctrl Pts',(2.49436329953803,6.93183595449864,2.01972548028308));
#40907=CARTESIAN_POINT('Ctrl Pts',(-1.1172473609771,7.28175504193768,2.1385328614762));
#40908=CARTESIAN_POINT('Ctrl Pts',(-4.45781917027722,5.86515526715037,2.25734024266932));
#40909=CARTESIAN_POINT('Ctrl Pts',(-6.60432779697333,3.16724420624364,2.37022506581929));
#40910=CARTESIAN_POINT('Ctrl Pts',(-7.06784911073517,0.99691864532032,2.44350742857156));
#40911=CARTESIAN_POINT('Ctrl Pts',(-7.06879387608848,-0.000152214530812871,
2.47718733092612));
#40912=CARTESIAN_POINT('Ctrl Pts',(-7.06887577069393,-0.000134259091651625,
1.27281266907389));
#40913=CARTESIAN_POINT('Ctrl Pts',(-7.06900268511687,-0.146153139652322,
1.27774518349456));
#40914=CARTESIAN_POINT('Ctrl Pts',(-7.02898406704184,-1.46446746156119,
1.32228015831295));
#40915=CARTESIAN_POINT('Ctrl Pts',(-6.24309683168348,-3.91100251149225,
1.40641759352904));
#40916=CARTESIAN_POINT('Ctrl Pts',(-3.61882898585832,-6.41687425365725,
1.52522497472216));
#40917=CARTESIAN_POINT('Ctrl Pts',(-0.116650592004996,-7.36604311957603,
1.64403235591529));
#40918=CARTESIAN_POINT('Ctrl Pts',(3.41382667831815,-6.5282452403422,1.76283973710841));
#40919=CARTESIAN_POINT('Ctrl Pts',(6.11612597108606,-4.10672639074461,1.88164711830153));
#40920=CARTESIAN_POINT('Ctrl Pts',(7.33468244243266,-0.688935413517191,
2.00045449949465));
#40921=CARTESIAN_POINT('Ctrl Pts',(6.77388013677175,2.89598798778839,2.11926188068778));
#40922=CARTESIAN_POINT('Ctrl Pts',(4.56976700382019,5.77835859632846,2.2380692618809));
#40923=CARTESIAN_POINT('Ctrl Pts',(1.25705031644168,7.25892712704843,2.35687664307402));
#40924=CARTESIAN_POINT('Ctrl Pts',(-2.36062074769956,6.97851475753138,2.47568402426714));
#40925=CARTESIAN_POINT('Ctrl Pts',(-5.40561654216747,5.00514818301045,2.59449140546027));
#40926=CARTESIAN_POINT('Ctrl Pts',(-6.85083513592755,2.34783644208199,2.69353428706251));
#40927=CARTESIAN_POINT('Ctrl Pts',(-7.06789813152101,0.587501716496959,
2.75297470826705));
#40928=CARTESIAN_POINT('Ctrl Pts',(-7.06790105247164,-1.00512680008963E-6,
2.77281266907389));
#40929=CARTESIAN_POINT('Ctrl Pts',(-3.08141029750819,6.36149375763354,-0.494500505560914));
#40930=CARTESIAN_POINT('Ctrl Pts',(-4.13669558412972,5.85032970200549,-0.454898045163206));
#40931=CARTESIAN_POINT('Ctrl Pts',(-5.98693791583793,4.29325218121263,-0.375693124367791));
#40932=CARTESIAN_POINT('Ctrl Pts',(-7.31006311005933,0.913880564558005,
-0.25688574317467));
#40933=CARTESIAN_POINT('Ctrl Pts',(-6.85969295893001,-2.68627098725521,
-0.138078361981547));
#40934=CARTESIAN_POINT('Ctrl Pts',(-4.74525181548372,-5.63519834469009,
-0.0192709807884249));
#40935=CARTESIAN_POINT('Ctrl Pts',(-1.47960575920872,-7.21682451563664,
0.0995364004046977));
#40936=CARTESIAN_POINT('Ctrl Pts',(2.14497044005655,-7.04780045183455,0.21834378159782));
#40937=CARTESIAN_POINT('Ctrl Pts',(5.24919481691,-5.16895421862038,0.337151162790942));
#40938=CARTESIAN_POINT('Ctrl Pts',(7.07998577213964,-2.03617489938541,0.455958543984065));
#40939=CARTESIAN_POINT('Ctrl Pts',(7.19320815162393,1.59058620557498,0.574765925177186));
#40940=CARTESIAN_POINT('Ctrl Pts',(5.56139171256912,4.83147080423204,0.693573306370309));
#40941=CARTESIAN_POINT('Ctrl Pts',(2.5804088453257,6.9002678057359,0.812380687563431));
#40942=CARTESIAN_POINT('Ctrl Pts',(-1.02656909712053,7.29509087359264,0.931188068756555));
#40943=CARTESIAN_POINT('Ctrl Pts',(-4.3845061645243,5.92016094290675,1.04999544994967));
#40944=CARTESIAN_POINT('Ctrl Pts',(-6.67878313815982,3.10902782828873,1.1688028311428));
#40945=CARTESIAN_POINT('Ctrl Pts',(-7.35281932448621,-0.456340249290331,
1.28761021233592));
#40946=CARTESIAN_POINT('Ctrl Pts',(-6.24309683168348,-3.91100251149225,
1.40641759352904));
#40947=CARTESIAN_POINT('Ctrl Pts',(-3.61882898585832,-6.41687425365725,
1.52522497472216));
#40948=CARTESIAN_POINT('Ctrl Pts',(-0.116650592004996,-7.36604311957603,
1.64403235591529));
#40949=CARTESIAN_POINT('Ctrl Pts',(3.41382667831815,-6.5282452403422,1.76283973710841));
#40950=CARTESIAN_POINT('Ctrl Pts',(6.11612597108606,-4.10672639074461,1.88164711830153));
#40951=CARTESIAN_POINT('Ctrl Pts',(7.33468244243266,-0.688935413517191,
2.00045449949465));
#40952=CARTESIAN_POINT('Ctrl Pts',(6.77388013677175,2.89598798778839,2.11926188068778));
#40953=CARTESIAN_POINT('Ctrl Pts',(4.56976700382019,5.77835859632846,2.2380692618809));
#40954=CARTESIAN_POINT('Ctrl Pts',(1.25705031644168,7.25892712704843,2.35687664307402));
#40955=CARTESIAN_POINT('Ctrl Pts',(-2.36062074769956,6.97851475753138,2.47568402426714));
#40956=CARTESIAN_POINT('Ctrl Pts',(-5.40561654216747,5.00514818301045,2.59449140546027));
#40957=CARTESIAN_POINT('Ctrl Pts',(-7.13923569377689,1.81755666864683,2.71329878665339));
#40958=CARTESIAN_POINT('Ctrl Pts',(-7.14091051238772,-1.81096537490967,
2.83210616784651));
#40959=CARTESIAN_POINT('Ctrl Pts',(-5.41023469503032,-5.0001559055375,2.95091354903963));
#40960=CARTESIAN_POINT('Ctrl Pts',(-2.36706189309541,-6.97633259881565,
3.06972093023276));
#40961=CARTESIAN_POINT('Ctrl Pts',(1.25034876951077,-7.26008446848898,3.18852831142588));
#40962=CARTESIAN_POINT('Ctrl Pts',(4.56443081844987,-5.78257467211716,3.307335692619));
#40963=CARTESIAN_POINT('Ctrl Pts',(6.7712038460194,-2.90223999880672,3.42614307381212));
#40964=CARTESIAN_POINT('Ctrl Pts',(7.33531530143303,0.682164176415201,3.54495045500525));
#40965=CARTESIAN_POINT('Ctrl Pts',(6.11991445160226,4.10107859472268,3.66375783619837));
#40966=CARTESIAN_POINT('Ctrl Pts',(3.41985171252147,6.5250910184752,3.78256521739149));
#40967=CARTESIAN_POINT('Ctrl Pts',(-0.109850647279407,7.36614766145199,
3.90137259858461));
#40968=CARTESIAN_POINT('Ctrl Pts',(-3.61290376699451,6.42021221654385,4.02017997977773));
#40969=CARTESIAN_POINT('Ctrl Pts',(-6.2394837636286,3.91676408511378,4.13898736097086));
#40970=CARTESIAN_POINT('Ctrl Pts',(-7.35239492947897,0.463127775019019,
4.25779474216397));
#40971=CARTESIAN_POINT('Ctrl Pts',(-6.68165035425043,-3.10286111171082,
4.3766021233571));
#40972=CARTESIAN_POINT('Ctrl Pts',(-4.38996945438879,-5.91611077690027,
4.49540950455022));
#40973=CARTESIAN_POINT('Ctrl Pts',(-1.03330302320227,-7.29414034669358,
4.61421688574334));
#40974=CARTESIAN_POINT('Ctrl Pts',(2.57403776474647,-6.90264645774946,4.73302426693647));
#40975=CARTESIAN_POINT('Ctrl Pts',(5.5569293384078,-4.83660364956287,4.85183164812959));
#40976=CARTESIAN_POINT('Ctrl Pts',(7.19173651068846,-1.59722399676838,4.97063902932272));
#40977=CARTESIAN_POINT('Ctrl Pts',(7.08186290362403,2.02963453589456,5.08944641051583));
#40978=CARTESIAN_POINT('Ctrl Pts',(5.25396332723401,5.16411346613359,5.20825379170895));
#40979=CARTESIAN_POINT('Ctrl Pts',(2.15147745047193,7.04580324130137,5.32706117290208));
#40980=CARTESIAN_POINT('Ctrl Pts',(-1.47294653532043,7.21821494824792,5.4458685540952));
#40981=CARTESIAN_POINT('Ctrl Pts',(-4.74004075724321,5.63952233391227,5.56467593528832));
#40982=CARTESIAN_POINT('Ctrl Pts',(-6.85722382903087,2.69270865367817,5.68348331648145));
#40983=CARTESIAN_POINT('Ctrl Pts',(-7.31087729341474,-0.907343229244046,
5.80229069767456));
#40984=CARTESIAN_POINT('Ctrl Pts',(-5.9909469960723,-4.28727799719992,5.9210980788677));
#40985=CARTESIAN_POINT('Ctrl Pts',(-3.21764169554554,-6.62713968874273,
6.0399054600608));
#40986=CARTESIAN_POINT('Ctrl Pts',(0.336248045567207,-7.35928908162156,
6.15871284125395));
#40987=CARTESIAN_POINT('Ctrl Pts',(3.80856562377858,-6.30611024518239,6.27752022244705));
#40988=CARTESIAN_POINT('Ctrl Pts',(6.35694345102643,-3.72309931313607,6.39632760364018));
#40989=CARTESIAN_POINT('Ctrl Pts',(7.36315729077195,-0.236882347113499,
6.5151349848333));
#40990=CARTESIAN_POINT('Ctrl Pts',(6.58310449221504,3.30680114001436,6.63394236602642));
#40991=CARTESIAN_POINT('Ctrl Pts',(4.20602212243871,6.04827053301837,6.75274974721955));
#40992=CARTESIAN_POINT('Ctrl Pts',(0.808578961688855,7.3224585077511,6.87155712841267));
#40993=CARTESIAN_POINT('Ctrl Pts',(-2.78502157648225,6.8202531737136,6.99036450960579));
#40994=CARTESIAN_POINT('Ctrl Pts',(-5.70298923971021,4.66348713590718,7.10917189079892));
#40995=CARTESIAN_POINT('Ctrl Pts',(-7.23743907013845,1.37538148928055,7.22797927199203));
#40996=CARTESIAN_POINT('Ctrl Pts',(-7.01612089953035,-2.24638510905758,
7.34678665318516));
#40997=CARTESIAN_POINT('Ctrl Pts',(-5.09272545443097,-5.32318945565654,
7.46559403437827));
#40998=CARTESIAN_POINT('Ctrl Pts',(-1.9338592434572,-7.10861357519998,7.58440141557141));
#40999=CARTESIAN_POINT('Ctrl Pts',(1.69415194342111,-7.16952214081417,7.70320879676452));
#41000=CARTESIAN_POINT('Ctrl Pts',(4.91116999552812,-5.49113902665435,7.82201617795765));
#41001=CARTESIAN_POINT('Ctrl Pts',(6.93676176518449,-2.48063192515472,7.94082355915077));
#41002=CARTESIAN_POINT('Ctrl Pts',(7.27952840566287,1.13166458200723,8.0596309403439));
#41003=CARTESIAN_POINT('Ctrl Pts',(5.85631637420563,4.46942469007289,8.178438321537));
#41004=CARTESIAN_POINT('Ctrl Pts',(3.01239008261732,6.72292380777671,8.29724570273014));
#41005=CARTESIAN_POINT('Ctrl Pts',(-0.562327592835126,7.34547385900723,
8.41605308392325));
#41006=CARTESIAN_POINT('Ctrl Pts',(-4.00062729170338,6.18604718765547,8.53486046511639));
#41007=CARTESIAN_POINT('Ctrl Pts',(-6.46839400027299,3.52591514252037,8.6536678463095));
#41008=CARTESIAN_POINT('Ctrl Pts',(-7.36695935271188,0.0104129973246502,
8.77247522750263));
#41009=CARTESIAN_POINT('Ctrl Pts',(-6.47833570485983,-3.50761529107176,
8.89128260869574));
#41010=CARTESIAN_POINT('Ctrl Pts',(-4.01809889103379,-6.17471293558617,
9.01008998988887));
#41011=CARTESIAN_POINT('Ctrl Pts',(-0.583090560721348,-7.34385484149978,
9.12889737108199));
#41012=CARTESIAN_POINT('Ctrl Pts',(2.99337274258629,-6.73141279071218,9.24770475227512));
#41013=CARTESIAN_POINT('Ctrl Pts',(5.84365817749679,-4.48596228691204,9.36651213346823));
#41014=CARTESIAN_POINT('Ctrl Pts',(7.27630017007747,-1.15223885108631,9.48531951466136));
#41015=CARTESIAN_POINT('Ctrl Pts',(6.94374664518998,2.46101220282127,9.60412689585448));
#41016=CARTESIAN_POINT('Ctrl Pts',(4.92667349274102,5.47723350159046,9.72293427704761));
#41017=CARTESIAN_POINT('Ctrl Pts',(1.71441298378659,7.16470422669678,9.84174165824072));
#41018=CARTESIAN_POINT('Ctrl Pts',(-1.91375589114147,7.11405207488272,9.96054903943386));
#41019=CARTESIAN_POINT('Ctrl Pts',(-5.07765676700238,5.33756501520463,10.079356420627));
#41020=CARTESIAN_POINT('Ctrl Pts',(-7.00974246827655,2.26621028668262,10.1981638018201));
#41021=CARTESIAN_POINT('Ctrl Pts',(-7.24129827188348,-1.35491618657003,
10.3169711830132));
#41022=CARTESIAN_POINT('Ctrl Pts',(-5.71614985062563,-4.64734649237981,
10.4357785642063));
#41023=CARTESIAN_POINT('Ctrl Pts',(-2.8042908954851,-6.81235283206109,10.5545859453995));
#41024=CARTESIAN_POINT('Ctrl Pts',(0.78787557894517,-7.32471505296642,10.6733933265926));
#41025=CARTESIAN_POINT('Ctrl Pts',(4.18890721731539,-6.0601365380463,10.7922007077857));
#41026=CARTESIAN_POINT('Ctrl Pts',(6.57373005855721,-3.32539796897586,10.9110080889788));
#41027=CARTESIAN_POINT('Ctrl Pts',(7.36379752129319,0.216066195757339,11.0298154701719));
#41028=CARTESIAN_POINT('Ctrl Pts',(6.36744302872343,3.70511373777206,11.1486228513651));
#41029=CARTESIAN_POINT('Ctrl Pts',(3.82637740176148,6.29531846027314,11.2674302325582));
#41030=CARTESIAN_POINT('Ctrl Pts',(0.357050971363174,7.3583091221159,11.3862376137513));
#41031=CARTESIAN_POINT('Ctrl Pts',(-3.1988943108167,6.63620928870937,11.5050449949444));
#41032=CARTESIAN_POINT('Ctrl Pts',(-5.97880318022623,4.30419691403035,11.6238523761376));
#41033=CARTESIAN_POINT('Ctrl Pts',(-7.30828307359288,0.928007017151897,
11.7426597573307));
#41034=CARTESIAN_POINT('Ctrl Pts',(-6.86480855900118,-2.67331293498022,
11.8614671385238));
#41035=CARTESIAN_POINT('Ctrl Pts',(-4.75596440127724,-5.62609998399613,
11.9802745197169));
#41036=CARTESIAN_POINT('Ctrl Pts',(-1.49334612632416,-7.21402218195007,
12.09908190091));
#41037=CARTESIAN_POINT('Ctrl Pts',(2.13155081922184,-7.05185717004641,12.2178892821032));
#41038=CARTESIAN_POINT('Ctrl Pts',(5.23934363589174,-5.17894550161347,12.3366966632963));
#41039=CARTESIAN_POINT('Ctrl Pts',(7.07609706408506,-2.04964636860042,12.4555040444894));
#41040=CARTESIAN_POINT('Ctrl Pts',(7.19622280814078,1.5768868890101,12.5743114256825));
#41041=CARTESIAN_POINT('Ctrl Pts',(5.57058035869953,4.82087544613853,12.6931188068757));
#41042=CARTESIAN_POINT('Ctrl Pts',(2.5935399939851,6.89534177632834,12.8119261880688));
#41043=CARTESIAN_POINT('Ctrl Pts',(-1.01267712366536,7.29703316651084,12.9307335692619));
#41044=CARTESIAN_POINT('Ctrl Pts',(-4.37323069894997,5.92849559402285,13.049540950455));
#41045=CARTESIAN_POINT('Ctrl Pts',(-6.67284563268825,3.12174071671263,13.1683483316481));
#41046=CARTESIAN_POINT('Ctrl Pts',(-7.3536873644992,-0.442347762287138,
13.2871557128413));
#41047=CARTESIAN_POINT('Ctrl Pts',(-6.25050664162124,-3.89909682044781,
13.4059630940344));
#41048=CARTESIAN_POINT('Ctrl Pts',(-3.63108720070629,-6.40999851148318,
13.5247704752275));
#41049=CARTESIAN_POINT('Ctrl Pts',(-0.130578947762305,-7.3657578324409,
13.6435778564207));
#41050=CARTESIAN_POINT('Ctrl Pts',(3.40120320632095,-6.5348310696329,13.7623852376137));
#41051=CARTESIAN_POINT('Ctrl Pts',(6.10869718244117,-4.11816204547854,13.8811926188069));
#41052=CARTESIAN_POINT('Ctrl Pts',(6.9243752846715,-1.84163918696265,13.9603975396023));
#41053=CARTESIAN_POINT('Ctrl Pts',(7.03625248964568,-0.674420604634066,
14.));
#41054=CARTESIAN_POINT('Ctrl Pts',(-3.20586989147275,6.61843744693175,-0.329667003707276));
#41055=CARTESIAN_POINT('Ctrl Pts',(-4.30377864125201,6.08662723753957,-0.290064543309568));
#41056=CARTESIAN_POINT('Ctrl Pts',(-6.22875312061569,4.46665863204891,-0.210859622514153));
#41057=CARTESIAN_POINT('Ctrl Pts',(-7.60531995633817,0.950792625275473,
-0.0920522413210315));
#41058=CARTESIAN_POINT('Ctrl Pts',(-7.13675914550065,-2.79477072084242,
0.0267551398720911));
#41059=CARTESIAN_POINT('Ctrl Pts',(-4.93691474160959,-5.86280662472249,
0.145562521065213));
#41060=CARTESIAN_POINT('Ctrl Pts',(-1.53936772345208,-7.50831541175523,
0.264369902258336));
#41061=CARTESIAN_POINT('Ctrl Pts',(2.23160679297952,-7.33246438746429,0.383177283451458));
#41062=CARTESIAN_POINT('Ctrl Pts',(5.46121223506488,-5.37773068171951,0.50198466464458));
#41063=CARTESIAN_POINT('Ctrl Pts',(7.36594968781422,-2.11841694985929,0.620792045837702));
#41064=CARTESIAN_POINT('Ctrl Pts',(7.48374517182464,1.65483072162386,0.739599427030824));
#41065=CARTESIAN_POINT('Ctrl Pts',(5.78601890842942,5.02661615538266,0.858406808223948));
#41066=CARTESIAN_POINT('Ctrl Pts',(2.68463275780226,7.17897282922568,0.977214189417068));
#41067=CARTESIAN_POINT('Ctrl Pts',(-1.0680327000388,7.58974298428242,1.09602157061019));
#41068=CARTESIAN_POINT('Ctrl Pts',(-4.56159840615571,6.15927899471405,1.21482895180331));
#41069=CARTESIAN_POINT('Ctrl Pts',(-6.94854229299388,3.23460290715646,1.33363633299644));
#41070=CARTESIAN_POINT('Ctrl Pts',(-7.64980311413618,-0.474772044037771,
1.45244371418956));
#41071=CARTESIAN_POINT('Ctrl Pts',(-6.49525841411903,-4.06896972052259,
1.57125109538268));
#41072=CARTESIAN_POINT('Ctrl Pts',(-3.76499517040421,-6.67605478692726,
1.6900584765758));
#41073=CARTESIAN_POINT('Ctrl Pts',(-0.121362163628049,-7.66356102445527,
1.80886585776892));
#41074=CARTESIAN_POINT('Ctrl Pts',(3.55171272439013,-6.79192409952275,1.92767323896205));
#41075=CARTESIAN_POINT('Ctrl Pts',(6.36315914145388,-4.27259897821829,2.04648062015517));
#41076=CARTESIAN_POINT('Ctrl Pts',(7.63093367498759,-0.716761835043583,
2.16528800134829));
#41077=CARTESIAN_POINT('Ctrl Pts',(7.04748030357494,3.0129582884906,2.28409538254141));
#41078=CARTESIAN_POINT('Ctrl Pts',(4.75434201684852,6.01174918545651,2.40290276373454));
#41079=CARTESIAN_POINT('Ctrl Pts',(1.30782316292173,7.55211856720863,2.52171014492766));
#41080=CARTESIAN_POINT('Ctrl Pts',(-2.45596731676912,7.26038021176852,2.64051752612078));
#41081=CARTESIAN_POINT('Ctrl Pts',(-5.6239519065006,5.20730844420442,2.7593249073139));
#41082=CARTESIAN_POINT('Ctrl Pts',(-7.4275927413221,1.89096862718099,2.87813228850702));
#41083=CARTESIAN_POINT('Ctrl Pts',(-7.42933520663497,-1.88411110802654,
2.99693966970015));
#41084=CARTESIAN_POINT('Ctrl Pts',(-5.62875658870384,-5.20211452632421,
3.11574705089327));
#41085=CARTESIAN_POINT('Ctrl Pts',(-2.46266862302097,-7.25810991464812,
3.2345544320864));
#41086=CARTESIAN_POINT('Ctrl Pts',(1.30085093739578,-7.55332265420782,3.35336181327951));
#41087=CARTESIAN_POINT('Ctrl Pts',(4.74879030047114,-6.01613555050572,3.47216919447264));
#41088=CARTESIAN_POINT('Ctrl Pts',(7.04469591619532,-3.01946282113952,3.59097657566576));
#41089=CARTESIAN_POINT('Ctrl Pts',(7.6315920954571,0.709717104528156,3.70978395685888));
#41090=CARTESIAN_POINT('Ctrl Pts',(6.3671006404588,4.26672306509026,3.82859133805201));
#41091=CARTESIAN_POINT('Ctrl Pts',(3.55798111252501,6.78864247716865,3.94739871924512));
#41092=CARTESIAN_POINT('Ctrl Pts',(-0.114287565974772,7.66366978882619,
4.06620610043825));
#41093=CARTESIAN_POINT('Ctrl Pts',(-3.75883062919679,6.67952757168615,4.18501348163137));
#41094=CARTESIAN_POINT('Ctrl Pts',(-6.49149941256627,4.07496400678033,4.30382086282449));
#41095=CARTESIAN_POINT('Ctrl Pts',(-7.64936157761737,0.481833721085094,
4.42262824401762));
#41096=CARTESIAN_POINT('Ctrl Pts',(-6.95152531727491,-3.22818711403002,
4.54143562521074));
#41097=CARTESIAN_POINT('Ctrl Pts',(-4.56728236083685,-6.15506524062029,
4.66024300640386));
#41098=CARTESIAN_POINT('Ctrl Pts',(-1.07503861252453,-7.58875406516016,
4.77905038759698));
#41099=CARTESIAN_POINT('Ctrl Pts',(2.67800434631753,-7.18144755609954,4.8978577687901));
#41100=CARTESIAN_POINT('Ctrl Pts',(5.78137629690187,-5.03195631872185,5.01666514998322));
#41101=CARTESIAN_POINT('Ctrl Pts',(7.48221409062784,-1.66173661628843,5.13547253117636));
#41102=CARTESIAN_POINT('Ctrl Pts',(7.36790263751166,2.11161241804746,5.25427991236947));
#41103=CARTESIAN_POINT('Ctrl Pts',(5.466173347737,5.37269440899007,5.3730872935626));
#41104=CARTESIAN_POINT('Ctrl Pts',(2.23837662456966,7.33038650866949,5.49189467475571));
#41105=CARTESIAN_POINT('Ctrl Pts',(-1.53243953041611,7.50976200458587,5.61070205594885));
#41106=CARTESIAN_POINT('Ctrl Pts',(-4.93149320630494,5.86730526187889,5.72950943714195));
#41107=CARTESIAN_POINT('Ctrl Pts',(-7.13419028629737,2.80146840760407,5.84831681833509));
#41108=CARTESIAN_POINT('Ctrl Pts',(-7.60616702493768,-0.943991243950004,
5.9671241995282));
#41109=CARTESIAN_POINT('Ctrl Pts',(-6.23292412946393,-4.46044314796747,
6.08593158072133));
#41110=CARTESIAN_POINT('Ctrl Pts',(-3.34760373898875,-6.89481294065417,
6.20473896191445));
#41111=CARTESIAN_POINT('Ctrl Pts',(0.349829260394867,-7.65653418776898,
6.32354634310758));
#41112=CARTESIAN_POINT('Ctrl Pts',(3.96239535930786,-6.56081696867387,6.44235372430069));
#41113=CARTESIAN_POINT('Ctrl Pts',(6.61370335132607,-3.8734770246591,6.56116110549382));
#41114=CARTESIAN_POINT('Ctrl Pts',(7.66055863568464,-0.246450135201629,
6.67996848668693));
#41115=CARTESIAN_POINT('Ctrl Pts',(6.84899914207391,3.44036437485541,6.79877586788007));
#41116=CARTESIAN_POINT('Ctrl Pts',(4.375905310662,6.29256299070766,6.91758324907318));
#41117=CARTESIAN_POINT('Ctrl Pts',(0.841237841728794,7.6182160099033,7.03639063026631));
#41118=CARTESIAN_POINT('Ctrl Pts',(-2.8975098922615,7.0957263690302,7.15519801145942));
#41119=CARTESIAN_POINT('Ctrl Pts',(-5.93333562549746,4.85184754862579,7.27400539265256));
#41120=CARTESIAN_POINT('Ctrl Pts',(-7.52976259769374,1.43093378682455,7.39281277384567));
#41121=CARTESIAN_POINT('Ctrl Pts',(-7.29950528331981,-2.33711764759276,
7.5116201550388));
#41122=CARTESIAN_POINT('Ctrl Pts',(-5.2984230023181,-5.5381955516585,7.63042753623192));
#41123=CARTESIAN_POINT('Ctrl Pts',(-2.01196871703817,-7.3957337811446,7.74923491742504));
#41124=CARTESIAN_POINT('Ctrl Pts',(1.76257952775252,-7.45910247203048,7.86804229861817));
#41125=CARTESIAN_POINT('Ctrl Pts',(5.10953443405443,-5.71292868388146,7.98684967981128));
#41126=CARTESIAN_POINT('Ctrl Pts',(7.21694079665652,-2.58082580145546,8.10565706100442));
#41127=CARTESIAN_POINT('Ctrl Pts',(7.5735519410405,1.17737304040193,8.22446444219752));
#41128=CARTESIAN_POINT('Ctrl Pts',(6.0928557142121,4.64994683041607,8.34327182339065));
#41129=CARTESIAN_POINT('Ctrl Pts',(3.13406191802616,6.99446582477044,8.46207920458377));
#41130=CARTESIAN_POINT('Ctrl Pts',(-0.585040265644679,7.64216096189278,
8.58088658577689));
#41131=CARTESIAN_POINT('Ctrl Pts',(-4.16221448725848,6.43590450845561,8.69969396697002));
#41132=CARTESIAN_POINT('Ctrl Pts',(-6.729655440052,3.66832849375325,8.81850134816314));
#41133=CARTESIAN_POINT('Ctrl Pts',(-7.66451426467329,0.0108335831259308,
8.93730872935627));
#41134=CARTESIAN_POINT('Ctrl Pts',(-6.73999869470739,-3.64928950279998,
9.05611611054938));
#41135=CARTESIAN_POINT('Ctrl Pts',(-4.18039177260559,-6.42411246067774,
9.17492349174251));
#41136=CARTESIAN_POINT('Ctrl Pts',(-0.606641859453193,-7.6404765515158,
9.29373087293563));
#41137=CARTESIAN_POINT('Ctrl Pts',(3.11427645879316,-7.00329768167184,9.41253825412875));
#41138=CARTESIAN_POINT('Ctrl Pts',(6.07968624705544,-4.66715238847722,9.53134563532187));
#41139=CARTESIAN_POINT('Ctrl Pts',(7.57019331551951,-1.19877831377079,9.650153016515));
#41140=CARTESIAN_POINT('Ctrl Pts',(7.2242077992116,2.5604136294189,9.76896039770811));
#41141=CARTESIAN_POINT('Ctrl Pts',(5.12566412472484,5.6984615081978,9.88776777890124));
#41142=CARTESIAN_POINT('Ctrl Pts',(1.78365892095447,7.4540899601228,10.0065751600944));
#41143=CARTESIAN_POINT('Ctrl Pts',(-1.9910533809796,7.40139194435702,10.1253825412875));
#41144=CARTESIAN_POINT('Ctrl Pts',(-5.28274568360125,5.55315174673762,10.2441899224806));
#41145=CARTESIAN_POINT('Ctrl Pts',(-7.29286922426337,2.35774357335561,10.3629973036737));
#41146=CARTESIAN_POINT('Ctrl Pts',(-7.53377767439077,-1.40964188102651,
10.4818046848669));
#41147=CARTESIAN_POINT('Ctrl Pts',(-5.94702779960401,-4.83505497700517,
10.60061206606));
#41148=CARTESIAN_POINT('Ctrl Pts',(-2.91755750801408,-7.08750692890673,
10.7194194472531));
#41149=CARTESIAN_POINT('Ctrl Pts',(0.819698239734408,-7.62056369802859,
10.8382268284462));
#41150=CARTESIAN_POINT('Ctrl Pts',(4.35809912656678,-6.30490826919325,10.9570342096394));
#41151=CARTESIAN_POINT('Ctrl Pts',(6.83924607068397,-3.45971233838136,11.0758415908324));
#41152=CARTESIAN_POINT('Ctrl Pts',(7.66122472541418,0.224793209818121,11.1946489720256));
#41153=CARTESIAN_POINT('Ctrl Pts',(6.62462701184582,3.85476500354751,11.3134563532187));
#41154=CARTESIAN_POINT('Ctrl Pts',(3.98092656328132,6.54958929855679,11.4322637344118));
#41155=CARTESIAN_POINT('Ctrl Pts',(0.37147242603168,7.65551464724345,11.5510711156049));
#41156=CARTESIAN_POINT('Ctrl Pts',(-3.32809913867807,6.90424886597847,11.6698784967981));
#41157=CARTESIAN_POINT('Ctrl Pts',(-6.22028981925211,4.47804542771158,11.7886858779912));
#41158=CARTESIAN_POINT('Ctrl Pts',(-7.60346802337159,0.965489651854728,
11.9074932591843));
#41159=CARTESIAN_POINT('Ctrl Pts',(-7.1420813670361,-2.78128928681395,12.0263006403774));
#41160=CARTESIAN_POINT('Ctrl Pts',(-4.94806001372185,-5.85334077701174,
12.1451080215706));
#41161=CARTESIAN_POINT('Ctrl Pts',(-1.55366307038099,-7.50539989050869,
12.2639154027637));
#41162=CARTESIAN_POINT('Ctrl Pts',(2.21764514742269,-7.33668495841004,12.3827227839568));
#41163=CARTESIAN_POINT('Ctrl Pts',(5.45096316026706,-5.38812551727601,12.5015301651499));
#41164=CARTESIAN_POINT('Ctrl Pts',(7.3619039130341,-2.13243253797661,12.6203375463431));
#41165=CARTESIAN_POINT('Ctrl Pts',(7.48688159171922,1.64057808329635,12.7391449275362));
#41166=CARTESIAN_POINT('Ctrl Pts',(5.79557868824736,5.01559284585168,12.8579523087293));
#41167=CARTESIAN_POINT('Ctrl Pts',(2.69829427965856,7.17384783520105,12.9767596899224));
#41168=CARTESIAN_POINT('Ctrl Pts',(-1.05357962331965,7.59176372731423,13.0955670711155));
#41169=CARTESIAN_POINT('Ctrl Pts',(-4.54986751928669,6.16795028626218,13.2143744523087));
#41170=CARTESIAN_POINT('Ctrl Pts',(-6.94236496891693,3.24782927505195,13.3331818335018));
#41171=CARTESIAN_POINT('Ctrl Pts',(-7.65070621468871,-0.460214393981673,
13.4519892146949));
#41172=CARTESIAN_POINT('Ctrl Pts',(-6.5029675097238,-4.05658315308385,13.570796595888));
#41173=CARTESIAN_POINT('Ctrl Pts',(-3.77774850024675,-6.66890133033136,
13.6896039770811));
#41174=CARTESIAN_POINT('Ctrl Pts',(-0.135853092147427,-7.66326421444017,
13.8084113582743));
#41175=CARTESIAN_POINT('Ctrl Pts',(3.53857938449235,-6.79877593351919,13.9272187394674));
#41176=CARTESIAN_POINT('Ctrl Pts',(6.3554303005832,-4.2844965243615,14.0460261206605));
#41177=CARTESIAN_POINT('Ctrl Pts',(7.20405402043916,-1.91602384960365,14.1252310414559));
#41178=CARTESIAN_POINT('Ctrl Pts',(7.32044999771583,-0.701660766284081,
14.1648335018536));
#41179=CARTESIAN_POINT('Ctrl Pts',(-3.33032948543731,6.87538113622997,-0.164833501853638));
#41180=CARTESIAN_POINT('Ctrl Pts',(-4.47086169837431,6.32292477307365,-0.12523104145593));
#41181=CARTESIAN_POINT('Ctrl Pts',(-6.47056832539346,4.6400650828852,-0.0460261206605157));
#41182=CARTESIAN_POINT('Ctrl Pts',(-7.900576802617,0.98770468599294,0.0727812605326066));
#41183=CARTESIAN_POINT('Ctrl Pts',(-7.41382533207128,-2.90327045442965,
0.191588641725729));
#41184=CARTESIAN_POINT('Ctrl Pts',(-5.12857766773546,-6.09041490475487,
0.310396022918851));
#41185=CARTESIAN_POINT('Ctrl Pts',(-1.59912968769544,-7.79980630787381,
0.429203404111974));
#41186=CARTESIAN_POINT('Ctrl Pts',(2.31824314590249,-7.61712832309403,0.548010785305095));
#41187=CARTESIAN_POINT('Ctrl Pts',(5.67322965321975,-5.58650714481864,0.666818166498218));
#41188=CARTESIAN_POINT('Ctrl Pts',(7.65191360348882,-2.20065900033317,0.78562554769134));
#41189=CARTESIAN_POINT('Ctrl Pts',(7.77428219202533,1.71907523767275,0.904432928884463));
#41190=CARTESIAN_POINT('Ctrl Pts',(6.01064610428973,5.22176150653328,1.02324031007758));
#41191=CARTESIAN_POINT('Ctrl Pts',(2.78885667027882,7.45767785271547,1.14204769127071));
#41192=CARTESIAN_POINT('Ctrl Pts',(-1.10949630295707,7.8843950949722,1.26085507246383));
#41193=CARTESIAN_POINT('Ctrl Pts',(-4.73869064778711,6.39839704652136,1.37966245365695));
#41194=CARTESIAN_POINT('Ctrl Pts',(-7.21830144782795,3.36017798602418,1.49846983485007));
#41195=CARTESIAN_POINT('Ctrl Pts',(-7.94678690378614,-0.493203838785206,
1.61727721604319));
#41196=CARTESIAN_POINT('Ctrl Pts',(-6.74741999655458,-4.22693692955293,
1.73608459723632));
#41197=CARTESIAN_POINT('Ctrl Pts',(-3.91116135495011,-6.93523532019726,
1.85489197842944));
#41198=CARTESIAN_POINT('Ctrl Pts',(-0.126073735251096,-7.96107892933453,
1.97369935962256));
#41199=CARTESIAN_POINT('Ctrl Pts',(3.6895987704621,-7.0556029587033,2.09250674081569));
#41200=CARTESIAN_POINT('Ctrl Pts',(6.61019231182172,-4.43847156569197,2.21131412200881));
#41201=CARTESIAN_POINT('Ctrl Pts',(7.92718490754252,-0.744588256569963,
2.33012150320193));
#41202=CARTESIAN_POINT('Ctrl Pts',(7.32108047037813,3.12992858919279,2.44892888439505));
#41203=CARTESIAN_POINT('Ctrl Pts',(4.93891702987685,6.24513977458459,2.56773626558817));
#41204=CARTESIAN_POINT('Ctrl Pts',(1.35859600940177,7.84531000736881,2.6865436467813));
#41205=CARTESIAN_POINT('Ctrl Pts',(-2.55131388583866,7.54224566600566,2.80535102797442));
#41206=CARTESIAN_POINT('Ctrl Pts',(-5.84228727083374,5.40946870539838,2.92415840916754));
#41207=CARTESIAN_POINT('Ctrl Pts',(-7.71594978886729,1.96438058571516,3.04296579036067));
#41208=CARTESIAN_POINT('Ctrl Pts',(-7.71775990088224,-1.95725684114341,
3.16177317155378));
#41209=CARTESIAN_POINT('Ctrl Pts',(-5.84727848237734,-5.40407314711093,
3.28058055274691));
#41210=CARTESIAN_POINT('Ctrl Pts',(-2.55827535294654,-7.53988723048059,
3.39938793394003));
#41211=CARTESIAN_POINT('Ctrl Pts',(1.3513531052808,-7.84656083992666,3.51819531513315));
#41212=CARTESIAN_POINT('Ctrl Pts',(4.93314978249241,-6.24969642889428,3.63700269632627));
#41213=CARTESIAN_POINT('Ctrl Pts',(7.31818798637123,-3.13668564347232,3.7558100775194));
#41214=CARTESIAN_POINT('Ctrl Pts',(7.92786888948117,0.737270032641113,3.87461745871252));
#41215=CARTESIAN_POINT('Ctrl Pts',(6.61428682931535,4.43236753545784,3.99342483990565));
#41216=CARTESIAN_POINT('Ctrl Pts',(3.69611051252854,7.05219393586209,4.11223222109876));
#41217=CARTESIAN_POINT('Ctrl Pts',(-0.118724484670133,7.9611919162004,4.23103960229189));
#41218=CARTESIAN_POINT('Ctrl Pts',(-3.90475749139907,6.93884292682844,4.349846983485));
#41219=CARTESIAN_POINT('Ctrl Pts',(-6.74351506150395,4.2331639284469,4.46865436467813));
#41220=CARTESIAN_POINT('Ctrl Pts',(-7.94632822575575,0.500539667151168,
4.58746174587125));
#41221=CARTESIAN_POINT('Ctrl Pts',(-7.22140028029939,-3.35351311634923,
4.70626912706438));
#41222=CARTESIAN_POINT('Ctrl Pts',(-4.7445952672849,-6.39401970434032,4.82507650825749));
#41223=CARTESIAN_POINT('Ctrl Pts',(-1.11677420184678,-7.88336778362672,
4.94388388945062));
#41224=CARTESIAN_POINT('Ctrl Pts',(2.78197092788859,-7.46024865444962,5.06269127064373));
#41225=CARTESIAN_POINT('Ctrl Pts',(6.00582325539593,-5.22730898788083,5.18149865183687));
#41226=CARTESIAN_POINT('Ctrl Pts',(7.77269167056723,-1.72624923580848,5.30030603302998));
#41227=CARTESIAN_POINT('Ctrl Pts',(7.65394237139929,2.19359030020036,5.41911341422311));
#41228=CARTESIAN_POINT('Ctrl Pts',(5.67838336823999,5.58127535184656,5.53792079541623));
#41229=CARTESIAN_POINT('Ctrl Pts',(2.32527579866739,7.6149697760376,5.65672817660936));
#41230=CARTESIAN_POINT('Ctrl Pts',(-1.5919325255118,7.80130906092382,5.77553555780247));
#41231=CARTESIAN_POINT('Ctrl Pts',(-5.12294565536668,6.0950881898455,5.8943429389956));
#41232=CARTESIAN_POINT('Ctrl Pts',(-7.41115674356387,2.91022816152997,6.01315032018872));
#41233=CARTESIAN_POINT('Ctrl Pts',(-7.90145675646063,-0.980639258655962,
6.13195770138184));
#41234=CARTESIAN_POINT('Ctrl Pts',(-6.47490126285554,-4.63360829873503,
6.25076508257496));
#41235=CARTESIAN_POINT('Ctrl Pts',(-3.47756578243197,-7.1624861925656,6.36957246376809));
#41236=CARTESIAN_POINT('Ctrl Pts',(0.363410475222534,-7.95377929391638,
6.48837984496121));
#41237=CARTESIAN_POINT('Ctrl Pts',(4.11622509483713,-6.81552369216537,6.60718722615433));
#41238=CARTESIAN_POINT('Ctrl Pts',(6.87046325162571,-4.02385473618211,6.72599460734745));
#41239=CARTESIAN_POINT('Ctrl Pts',(7.95795998059733,-0.256017923289772,
6.84480198854058));
#41240=CARTESIAN_POINT('Ctrl Pts',(7.11489379193279,3.57392760969647,6.96360936973369));
#41241=CARTESIAN_POINT('Ctrl Pts',(4.54578849888529,6.53685544839694,7.08241675092683));
#41242=CARTESIAN_POINT('Ctrl Pts',(0.873896721768728,7.91397351205552,7.20122413211994));
#41243=CARTESIAN_POINT('Ctrl Pts',(-3.00999820804074,7.37119956434678,7.32003151331307));
#41244=CARTESIAN_POINT('Ctrl Pts',(-6.16368201128471,5.04020796134442,7.43883889450619));
#41245=CARTESIAN_POINT('Ctrl Pts',(-7.82208612524901,1.48648608436854,7.5576462756993));
#41246=CARTESIAN_POINT('Ctrl Pts',(-7.5828896671093,-2.42785018612792,7.67645365689243));
#41247=CARTESIAN_POINT('Ctrl Pts',(-5.50412055020522,-5.75320164766046,
7.79526103808555));
#41248=CARTESIAN_POINT('Ctrl Pts',(-2.09007819061915,-7.68285398708923,
7.91406841927868));
#41249=CARTESIAN_POINT('Ctrl Pts',(1.83100711208394,-7.74868280324678,8.0328758004718));
#41250=CARTESIAN_POINT('Ctrl Pts',(5.30789887258074,-5.93471834110859,8.15168318166492));
#41251=CARTESIAN_POINT('Ctrl Pts',(7.49711982812857,-2.6810196777562,8.27049056285805));
#41252=CARTESIAN_POINT('Ctrl Pts',(7.86757547641812,1.22308149879663,8.38929794405116));
#41253=CARTESIAN_POINT('Ctrl Pts',(6.32939505421858,4.83046897075924,8.5081053252443));
#41254=CARTESIAN_POINT('Ctrl Pts',(3.25573375343499,7.26600784176417,8.6269127064374));
#41255=CARTESIAN_POINT('Ctrl Pts',(-0.607752938454231,7.93884806477834,
8.74572008763054));
#41256=CARTESIAN_POINT('Ctrl Pts',(-4.32380168281358,6.68576182925573,8.86452746882365));
#41257=CARTESIAN_POINT('Ctrl Pts',(-6.99091687983101,3.81074184498614,8.98333485001678));
#41258=CARTESIAN_POINT('Ctrl Pts',(-7.96206917663469,0.0112541689272012,
9.10214223120989));
#41259=CARTESIAN_POINT('Ctrl Pts',(-7.00166168455497,-3.79096371452819,
9.22094961240303));
#41260=CARTESIAN_POINT('Ctrl Pts',(-4.34268465417737,-6.67351198576931,
9.33975699359614));
#41261=CARTESIAN_POINT('Ctrl Pts',(-0.63019315818504,-7.93709826153181,
9.45856437478927));
#41262=CARTESIAN_POINT('Ctrl Pts',(3.23518017500003,-7.2751825726315,9.57737175598238));
#41263=CARTESIAN_POINT('Ctrl Pts',(6.31571431661408,-4.8483424900424,9.69617913717552));
#41264=CARTESIAN_POINT('Ctrl Pts',(7.86408646096156,-1.24531777645527,9.81498651836863));
#41265=CARTESIAN_POINT('Ctrl Pts',(7.50466895323321,2.65981505601654,9.93379389956176));
#41266=CARTESIAN_POINT('Ctrl Pts',(5.32465475670866,5.91968951480514,10.0526012807549));
#41267=CARTESIAN_POINT('Ctrl Pts',(1.85290485812236,7.74347569354884,10.171408661948));
#41268=CARTESIAN_POINT('Ctrl Pts',(-2.06835087081773,7.6887318138313,10.2902160431411));
#41269=CARTESIAN_POINT('Ctrl Pts',(-5.48783460020011,5.76873847827063,10.4090234243343));
#41270=CARTESIAN_POINT('Ctrl Pts',(-7.57599598025021,2.44927686002859,10.5278308055273));
#41271=CARTESIAN_POINT('Ctrl Pts',(-7.82625707689805,-1.46436757548299,
10.6466381867205));
#41272=CARTESIAN_POINT('Ctrl Pts',(-6.17790574858239,-5.02276346163052,
10.7654455679136));
#41273=CARTESIAN_POINT('Ctrl Pts',(-3.03082412054307,-7.36266102575237,
10.8842529491067));
#41274=CARTESIAN_POINT('Ctrl Pts',(0.851520900523648,-7.91641234309075,
11.0030603302998));
#41275=CARTESIAN_POINT('Ctrl Pts',(4.52729103581818,-6.54968000034022,11.121867711493));
#41276=CARTESIAN_POINT('Ctrl Pts',(7.10476208281073,-3.59402670778684,11.2406750926861));
#41277=CARTESIAN_POINT('Ctrl Pts',(7.95865192953517,0.233520223878897,11.3594824738792));
#41278=CARTESIAN_POINT('Ctrl Pts',(6.88181099496819,4.00441626932297,11.4782898550723));
#41279=CARTESIAN_POINT('Ctrl Pts',(4.13547572480117,6.80386013684043,11.5970972362655));
#41280=CARTESIAN_POINT('Ctrl Pts',(0.385893880700171,7.952720172371,11.7159046174586));
#41281=CARTESIAN_POINT('Ctrl Pts',(-3.45730396653943,7.17228844324756,11.8347119986517));
#41282=CARTESIAN_POINT('Ctrl Pts',(-6.46177645827802,4.6518939413928,11.9535193798448));
#41283=CARTESIAN_POINT('Ctrl Pts',(-7.89865297315028,1.00297228655756,12.072326761038));
#41284=CARTESIAN_POINT('Ctrl Pts',(-7.41935417507103,-2.88926563864769,
12.1911341422311));
#41285=CARTESIAN_POINT('Ctrl Pts',(-5.14015562616646,-6.08058157002734,
12.3099415234242));
#41286=CARTESIAN_POINT('Ctrl Pts',(-1.61398001443781,-7.79677759906733,
12.4287489046173));
#41287=CARTESIAN_POINT('Ctrl Pts',(2.30373947562354,-7.62151274677366,12.5475562858105));
#41288=CARTESIAN_POINT('Ctrl Pts',(5.6625826846424,-5.59730553293856,12.6663636670036));
#41289=CARTESIAN_POINT('Ctrl Pts',(7.64771076198313,-2.21521870735279,12.7851710481967));
#41290=CARTESIAN_POINT('Ctrl Pts',(7.77754037529766,1.70426927758259,12.9039784293898));
#41291=CARTESIAN_POINT('Ctrl Pts',(6.02057701779519,5.21031024556484,13.022785810583));
#41292=CARTESIAN_POINT('Ctrl Pts',(2.80304856533202,7.45235389407376,13.141593191776));
#41293=CARTESIAN_POINT('Ctrl Pts',(-1.09448212297394,7.88649428811764,13.2604005729692));
#41294=CARTESIAN_POINT('Ctrl Pts',(-4.72650433962341,6.40740497850149,13.3792079541623));
#41295=CARTESIAN_POINT('Ctrl Pts',(-7.21188430514562,3.37391783339129,13.4980153353554));
#41296=CARTESIAN_POINT('Ctrl Pts',(-7.94772506487821,-0.47808102567622,
13.6168227165485));
#41297=CARTESIAN_POINT('Ctrl Pts',(-6.75542837782637,-4.21406948571987,
13.7356300977417));
#41298=CARTESIAN_POINT('Ctrl Pts',(-3.9244097997872,-6.92780414917955,13.8544374789348));
#41299=CARTESIAN_POINT('Ctrl Pts',(-0.141127236532553,-7.96077059643944,
13.9732448601279));
#41300=CARTESIAN_POINT('Ctrl Pts',(3.67595556266374,-7.06272079740548,14.092052241321));
#41301=CARTESIAN_POINT('Ctrl Pts',(6.60216341872522,-4.45083100324446,14.2108596225142));
#41302=CARTESIAN_POINT('Ctrl Pts',(7.48373275620681,-1.99040851224466,14.2900645433096));
#41303=CARTESIAN_POINT('Ctrl Pts',(7.60464750578597,-0.728900927934096,
14.3296670037073));
#41304=CARTESIAN_POINT('Ctrl Pts',(-3.45478907940187,7.13232482552818,0.));
#41305=CARTESIAN_POINT('Ctrl Pts',(-4.6379447554966,6.55922230860773,0.0396024603977074));
#41306=CARTESIAN_POINT('Ctrl Pts',(-6.71238353017122,4.81347153372149,0.118807381193122));
#41307=CARTESIAN_POINT('Ctrl Pts',(-8.19583364889584,1.02461674671041,0.237614762386245));
#41308=CARTESIAN_POINT('Ctrl Pts',(-7.69089151864192,-3.01177018801687,
0.356422143579367));
#41309=CARTESIAN_POINT('Ctrl Pts',(-5.32024059386133,-6.31802318478726,
0.475229524772489));
#41310=CARTESIAN_POINT('Ctrl Pts',(-1.65889165193879,-8.0912972039924,0.594036905965612));
#41311=CARTESIAN_POINT('Ctrl Pts',(2.40487949882547,-7.90179225872376,0.712844287158733));
#41312=CARTESIAN_POINT('Ctrl Pts',(5.88524707137462,-5.79528360791777,0.831651668351856));
#41313=CARTESIAN_POINT('Ctrl Pts',(7.93787751916342,-2.28290105080705,0.950459049544978));
#41314=CARTESIAN_POINT('Ctrl Pts',(8.06481921222603,1.78331975372163,1.0692664307381));
#41315=CARTESIAN_POINT('Ctrl Pts',(6.23527330015003,5.41690685768391,1.18807381193122));
#41316=CARTESIAN_POINT('Ctrl Pts',(2.89308058275538,7.73638287620525,1.30688119312434));
#41317=CARTESIAN_POINT('Ctrl Pts',(-1.15095990587534,8.17904720566199,1.42568857431747));
#41318=CARTESIAN_POINT('Ctrl Pts',(-4.91578288941853,6.63751509832866,1.54449595551059));
#41319=CARTESIAN_POINT('Ctrl Pts',(-7.488060602662,3.48575306489192,1.66330333670371));
#41320=CARTESIAN_POINT('Ctrl Pts',(-8.24377069343612,-0.511635633532653,
1.78211071789683));
#41321=CARTESIAN_POINT('Ctrl Pts',(-6.99958157899013,-4.38490413858326,
1.90091809908996));
#41322=CARTESIAN_POINT('Ctrl Pts',(-4.057327539496,-7.1944158534673,2.01972548028308));
#41323=CARTESIAN_POINT('Ctrl Pts',(-0.130785306874149,-8.25859683421376,
2.1385328614762));
#41324=CARTESIAN_POINT('Ctrl Pts',(3.82748481653407,-7.31928181788386,2.25734024266932));
#41325=CARTESIAN_POINT('Ctrl Pts',(6.85722548218955,-4.60434415316564,2.37614762386244));
#41326=CARTESIAN_POINT('Ctrl Pts',(8.22343614009745,-0.772414678096356,
2.49495500505557));
#41327=CARTESIAN_POINT('Ctrl Pts',(7.59468063718132,3.24689888989499,2.61376238624869));
#41328=CARTESIAN_POINT('Ctrl Pts',(5.12349204290518,6.47853036371263,2.73256976744181));
#41329=CARTESIAN_POINT('Ctrl Pts',(1.40936885588182,8.13850144752901,2.85137714863493));
#41330=CARTESIAN_POINT('Ctrl Pts',(-2.64666045490822,7.8241111202428,2.97018452982806));
#41331=CARTESIAN_POINT('Ctrl Pts',(-6.06062263516686,5.61162896659236,3.08899191102118));
#41332=CARTESIAN_POINT('Ctrl Pts',(-8.00430683641251,2.03779254424933,3.2077992922143));
#41333=CARTESIAN_POINT('Ctrl Pts',(-8.00618459512947,-2.03040257426028,
3.32660667340743));
#41334=CARTESIAN_POINT('Ctrl Pts',(-6.06580037605087,-5.60603176789764,
3.44541405460054));
#41335=CARTESIAN_POINT('Ctrl Pts',(-2.65388208287209,-7.82166454631306,
3.56422143579367));
#41336=CARTESIAN_POINT('Ctrl Pts',(1.40185527316581,-8.13979902564551,3.68302881698679));
#41337=CARTESIAN_POINT('Ctrl Pts',(5.11750926451368,-6.48325730728283,3.80183619817991));
#41338=CARTESIAN_POINT('Ctrl Pts',(7.59168005654716,-3.25390846580513,3.92064357937303));
#41339=CARTESIAN_POINT('Ctrl Pts',(8.22414568350524,0.764822960754067,4.03945096056616));
#41340=CARTESIAN_POINT('Ctrl Pts',(6.86147301817189,4.59801200582542,4.15825834175928));
#41341=CARTESIAN_POINT('Ctrl Pts',(3.83423991253207,7.31574539455554,4.27706572295241));
#41342=CARTESIAN_POINT('Ctrl Pts',(-0.123161403365499,8.25871404357459,
4.39587310414552));
#41343=CARTESIAN_POINT('Ctrl Pts',(-4.05068435360135,7.19815828197074,4.51468048533865));
#41344=CARTESIAN_POINT('Ctrl Pts',(-6.99553071044162,4.39136385011345,4.63348786653177));
#41345=CARTESIAN_POINT('Ctrl Pts',(-8.24329487389415,0.519245613217243,
4.75229524772489));
#41346=CARTESIAN_POINT('Ctrl Pts',(-7.49127524332387,-3.47883911866845,
4.87110262891801));
#41347=CARTESIAN_POINT('Ctrl Pts',(-4.92190817373296,-6.63297416806032,
4.98991001011114));
#41348=CARTESIAN_POINT('Ctrl Pts',(-1.15850979116904,-8.17798150209332,
5.10871739130425));
#41349=CARTESIAN_POINT('Ctrl Pts',(2.88593750945964,-7.73904975279968,5.22752477249739));
#41350=CARTESIAN_POINT('Ctrl Pts',(6.23027021389002,-5.42266165703982,5.34633215369049));
#41351=CARTESIAN_POINT('Ctrl Pts',(8.06316925050661,-1.79076185532853,5.46513953488364));
#41352=CARTESIAN_POINT('Ctrl Pts',(7.93998210528692,2.27556818235326,5.58394691607674));
#41353=CARTESIAN_POINT('Ctrl Pts',(5.89059338874298,5.78985629470304,5.70275429726988));
#41354=CARTESIAN_POINT('Ctrl Pts',(2.41217497276513,7.89955304340571,5.82156167846299));
#41355=CARTESIAN_POINT('Ctrl Pts',(-1.65142552060749,8.09285611726176,5.94036905965612));
#41356=CARTESIAN_POINT('Ctrl Pts',(-5.31439810442841,6.32287111781213,6.05917644084924));
#41357=CARTESIAN_POINT('Ctrl Pts',(-7.68812320083037,3.01898791545586,6.17798382204235));
#41358=CARTESIAN_POINT('Ctrl Pts',(-8.19674648798357,-1.01728727336192,
6.29679120323548));
#41359=CARTESIAN_POINT('Ctrl Pts',(-6.71687839624717,-4.8067734495026,6.4155985844286));
#41360=CARTESIAN_POINT('Ctrl Pts',(-3.60752782587519,-7.43015944447703,
6.53440596562173));
#41361=CARTESIAN_POINT('Ctrl Pts',(0.376991690050199,-8.25102440006379,
6.65321334681485));
#41362=CARTESIAN_POINT('Ctrl Pts',(4.2700548303664,-7.07023041565686,6.77202072800797));
#41363=CARTESIAN_POINT('Ctrl Pts',(7.12722315192535,-4.17423244770513,6.89082810920109));
#41364=CARTESIAN_POINT('Ctrl Pts',(8.25536132551003,-0.265585711377908,
7.00963549039422));
#41365=CARTESIAN_POINT('Ctrl Pts',(7.38078844179166,3.70749084453752,7.12844287158733));
#41366=CARTESIAN_POINT('Ctrl Pts',(4.71567168710858,6.78114790608622,7.24725025278046));
#41367=CARTESIAN_POINT('Ctrl Pts',(0.90655560180866,8.20973101420773,7.36605763397358));
#41368=CARTESIAN_POINT('Ctrl Pts',(-3.12248652381999,7.64667275966336,7.4848650151667));
#41369=CARTESIAN_POINT('Ctrl Pts',(-6.39402839707196,5.22856837406304,7.60367239635983));
#41370=CARTESIAN_POINT('Ctrl Pts',(-8.1144096528043,1.54203838191253,7.72247977755296));
#41371=CARTESIAN_POINT('Ctrl Pts',(-7.86627405089878,-2.51858272466308,
7.84128715874606));
#41372=CARTESIAN_POINT('Ctrl Pts',(-5.70981809809234,-5.96820774366244,
7.9600945399392));
#41373=CARTESIAN_POINT('Ctrl Pts',(-2.16818766420013,-7.96997419303383,
8.07890192113231));
#41374=CARTESIAN_POINT('Ctrl Pts',(1.89943469641536,-8.03826313446309,8.19770930232545));
#41375=CARTESIAN_POINT('Ctrl Pts',(5.50626331110705,-6.1565079983357,8.31651668351855));
#41376=CARTESIAN_POINT('Ctrl Pts',(7.7772988596006,-2.78121355405694,8.43532406471168));
#41377=CARTESIAN_POINT('Ctrl Pts',(8.16159901179575,1.26878995719133,8.55413144590481));
#41378=CARTESIAN_POINT('Ctrl Pts',(6.56593439422505,5.01099111110242,8.67293882709792));
#41379=CARTESIAN_POINT('Ctrl Pts',(3.37740558884383,7.53754985875791,8.79174620829106));
#41380=CARTESIAN_POINT('Ctrl Pts',(-0.630465611263786,8.2355351676639,8.91055358948416));
#41381=CARTESIAN_POINT('Ctrl Pts',(-4.48538887836867,6.93561915005586,9.0293609706773));
#41382=CARTESIAN_POINT('Ctrl Pts',(-7.25217831961001,3.95315519621903,9.14816835187041));
#41383=CARTESIAN_POINT('Ctrl Pts',(-8.25962408859611,0.0116747547284766,
9.26697573306354));
#41384=CARTESIAN_POINT('Ctrl Pts',(-7.26332467440254,-3.93263792625641,
9.38578311425666));
#41385=CARTESIAN_POINT('Ctrl Pts',(-4.50497753574917,-6.92291151086089,
9.50459049544978));
#41386=CARTESIAN_POINT('Ctrl Pts',(-0.653744456916887,-8.23371997154782,
9.62339787664291));
#41387=CARTESIAN_POINT('Ctrl Pts',(3.35608389120691,-7.54706746359117,9.74220525783602));
#41388=CARTESIAN_POINT('Ctrl Pts',(6.55174238617272,-5.02953259160757,9.86101263902915));
#41389=CARTESIAN_POINT('Ctrl Pts',(8.15797960640361,-1.29185723913975,9.97982002022227));
#41390=CARTESIAN_POINT('Ctrl Pts',(7.78513010725481,2.75921648261417,10.0986274014154));
#41391=CARTESIAN_POINT('Ctrl Pts',(5.52364538869249,6.14091752141248,10.2174347826085));
#41392=CARTESIAN_POINT('Ctrl Pts',(1.92215079529024,8.03286142697488,10.3362421638016));
#41393=CARTESIAN_POINT('Ctrl Pts',(-2.14564836065585,7.9760716833056,10.4550495449947));
#41394=CARTESIAN_POINT('Ctrl Pts',(-5.69292351679898,5.98432520980362,10.5738569261879));
#41395=CARTESIAN_POINT('Ctrl Pts',(-7.85912273623703,2.54081014670158,10.692664307381));
#41396=CARTESIAN_POINT('Ctrl Pts',(-8.11873647940535,-1.51909326993947,
10.8114716885741));
#41397=CARTESIAN_POINT('Ctrl Pts',(-6.40878369756076,-5.21047194625588,
10.9302790697672));
#41398=CARTESIAN_POINT('Ctrl Pts',(-3.14409073307205,-7.637815122598,11.0490864509604));
#41399=CARTESIAN_POINT('Ctrl Pts',(0.883343561312894,-8.21226098815292,
11.1678938321535));
#41400=CARTESIAN_POINT('Ctrl Pts',(4.69648294506956,-6.79445173148717,11.2867012133466));
#41401=CARTESIAN_POINT('Ctrl Pts',(7.37027809493751,-3.72834107719234,11.4055085945397));
#41402=CARTESIAN_POINT('Ctrl Pts',(8.25607913365615,0.242247237939676,11.5243159757329));
#41403=CARTESIAN_POINT('Ctrl Pts',(7.13899497809059,4.15406753509843,11.643123356926));
#41404=CARTESIAN_POINT('Ctrl Pts',(4.290024886321,7.05813097512407,11.7619307381191));
#41405=CARTESIAN_POINT('Ctrl Pts',(0.400315335368676,8.24992569749855,11.8807381193122));
#41406=CARTESIAN_POINT('Ctrl Pts',(-3.5865087944008,7.44032802051665,11.9995455005053));
#41407=CARTESIAN_POINT('Ctrl Pts',(-6.7032630973039,4.82574245507403,12.1183528816985));
#41408=CARTESIAN_POINT('Ctrl Pts',(-8.19383792292899,1.04045492126039,12.2371602628916));
#41409=CARTESIAN_POINT('Ctrl Pts',(-7.69662698310595,-2.99724199048142,
12.3559676440847));
#41410=CARTESIAN_POINT('Ctrl Pts',(-5.33225123861107,-6.30782236304295,
12.4747750252778));
#41411=CARTESIAN_POINT('Ctrl Pts',(-1.67429695849463,-8.08815530762596,
12.593582406471));
#41412=CARTESIAN_POINT('Ctrl Pts',(2.38983380382439,-7.90634053513729,12.7123897876641));
#41413=CARTESIAN_POINT('Ctrl Pts',(5.87420220901772,-5.80648554860111,12.8311971688572));
#41414=CARTESIAN_POINT('Ctrl Pts',(7.93351761093217,-2.29800487672896,12.9500045500503));
#41415=CARTESIAN_POINT('Ctrl Pts',(8.06819915887609,1.76796047186882,13.0688119312434));
#41416=CARTESIAN_POINT('Ctrl Pts',(6.24557534734301,5.40502764527801,13.1876193124366));
#41417=CARTESIAN_POINT('Ctrl Pts',(2.90780285100547,7.73085995294645,13.3064266936297));
#41418=CARTESIAN_POINT('Ctrl Pts',(-1.13538462262823,8.18122484892105,13.4252340748228));
#41419=CARTESIAN_POINT('Ctrl Pts',(-4.90314115996014,6.6468596707408,13.5440414560159));
#41420=CARTESIAN_POINT('Ctrl Pts',(-7.48140364137431,3.50000639173062,13.6628488372091));
#41421=CARTESIAN_POINT('Ctrl Pts',(-8.24474391506772,-0.495947657370763,
13.7816562184022));
#41422=CARTESIAN_POINT('Ctrl Pts',(-7.00788924592892,-4.3715558183559,13.9004635995953));
#41423=CARTESIAN_POINT('Ctrl Pts',(-4.07107109932766,-7.18670696802772,
14.0192709807884));
#41424=CARTESIAN_POINT('Ctrl Pts',(-0.146401380917679,-8.25827697843872,
14.1380783619815));
#41425=CARTESIAN_POINT('Ctrl Pts',(3.81333174083514,-7.32666566129177,14.2568857431747));
#41426=CARTESIAN_POINT('Ctrl Pts',(6.84889653686724,-4.61716548212742,14.3756931243678));
#41427=CARTESIAN_POINT('Ctrl Pts',(7.76341149197447,-2.06479317488566,14.4548980451632));
#41428=CARTESIAN_POINT('Ctrl Pts',(7.88884501385612,-0.756141089584111,
14.4945005055609));
#41429=CARTESIAN_POINT('',(-4.44937994724887,-6.55809752024317,14.));
#41430=CARTESIAN_POINT('Ctrl Pts',(-4.44940638321902,-6.5584391708898,14.));
#41431=CARTESIAN_POINT('Ctrl Pts',(-4.26689467651366,-6.66907515586647,
14.));
#41432=CARTESIAN_POINT('Ctrl Pts',(-4.08028782328584,-6.77205836122323,
14.));
#41433=CARTESIAN_POINT('Ctrl Pts',(-3.88997616949827,-6.86706524648209,
14.));
#41434=CARTESIAN_POINT('Ctrl Pts',(-3.70514829807453,-6.95933453227472,
14.));
#41435=CARTESIAN_POINT('Ctrl Pts',(-3.51682535429916,-7.04408071741637,
14.));
#41436=CARTESIAN_POINT('Ctrl Pts',(-3.32549660258128,-7.12123542969775,
14.));
#41437=CARTESIAN_POINT('Ctrl Pts',(-3.13345808093299,-7.19867636187171,
14.));
#41438=CARTESIAN_POINT('Ctrl Pts',(-2.93839070791496,-7.26846953339858,
14.));
#41439=CARTESIAN_POINT('Ctrl Pts',(-2.7407745157787,-7.33049546272157,14.));
#41440=CARTESIAN_POINT('Ctrl Pts',(-2.54412235497741,-7.39221881087042,
14.));
#41441=CARTESIAN_POINT('Ctrl Pts',(-2.34494548635082,-7.44625059009398,
14.));
#41442=CARTESIAN_POINT('Ctrl Pts',(-2.1437128994453,-7.49242178207046,14.));
#41443=CARTESIAN_POINT('Ctrl Pts',(-1.97939455606432,-7.53012329897767,
14.));
#41444=CARTESIAN_POINT('Ctrl Pts',(-1.81370528628452,-7.56258270331728,
14.));
#41445=CARTESIAN_POINT('Ctrl Pts',(-1.64690325240232,-7.58968182048372,
14.));
#41446=CARTESIAN_POINT('Ctrl Pts',(-1.61532958921609,-7.59481136463941,
14.));
#41447=CARTESIAN_POINT('Ctrl Pts',(-1.58371164972916,-7.59974937840371,
14.));
#41448=CARTESIAN_POINT('Ctrl Pts',(-1.55207992279835,-7.60449085285328,
14.));
#41449=CARTESIAN_POINT('Ctrl Pts',(-1.34986154646332,-7.63480261125719,
14.));
#41450=CARTESIAN_POINT('Ctrl Pts',(-1.14687126288046,-7.65712242315947,
14.));
#41451=CARTESIAN_POINT('Ctrl Pts',(-0.943573958042012,-7.67137342384431,
14.));
#41452=CARTESIAN_POINT('Ctrl Pts',(-0.741135905208625,-7.68556419155694,
14.));
#41453=CARTESIAN_POINT('Ctrl Pts',(-0.538392736482371,-7.69175426249507,
14.));
#41454=CARTESIAN_POINT('Ctrl Pts',(-0.335799622499727,-7.68981648545354,
14.));
#41455=CARTESIAN_POINT('Ctrl Pts',(-0.269283413955203,-7.689180266486,14.));
#41456=CARTESIAN_POINT('Ctrl Pts',(-0.202783393657834,-7.68766747636142,
14.));
#41457=CARTESIAN_POINT('Ctrl Pts',(-0.136315770622695,-7.68527238702149,
14.));
#41458=CARTESIAN_POINT('Ctrl Pts',(0.0672666969070029,-7.67793651166577,
14.));
#41459=CARTESIAN_POINT('Ctrl Pts',(0.270546320464125,-7.66232728574139,
14.));
#41460=CARTESIAN_POINT('Ctrl Pts',(0.473045266450486,-7.63856454842076,
14.));
#41461=CARTESIAN_POINT('Ctrl Pts',(0.674485516628634,-7.61492604636601,
14.));
#41462=CARTESIAN_POINT('Ctrl Pts',(0.875153886334405,-7.58321879930691,
14.));
#41463=CARTESIAN_POINT('Ctrl Pts',(1.07456032484331,-7.5435134068963,14.));
#41464=CARTESIAN_POINT('Ctrl Pts',(1.13439659455426,-7.53159893418906,14.));
#41465=CARTESIAN_POINT('Ctrl Pts',(1.19411906441983,-7.51896397318094,14.));
#41466=CARTESIAN_POINT('Ctrl Pts',(1.2537140095434,-7.50560964743804,14.));
#41467=CARTESIAN_POINT('Ctrl Pts',(1.28943769992771,-7.49760450879513,14.));
#41468=CARTESIAN_POINT('Ctrl Pts',(1.32511556208652,-7.48934087383794,14.));
#41469=CARTESIAN_POINT('Ctrl Pts',(1.3607445945539,-7.48081892436368,14.));
#41470=CARTESIAN_POINT('Ctrl Pts',(1.38465203572509,-7.47510061006742,14.));
#41471=CARTESIAN_POINT('Ctrl Pts',(1.40852886519995,-7.46926803693634,14.));
#41472=CARTESIAN_POINT('Ctrl Pts',(1.43237022598248,-7.46332253618824,14.));
#41473=CARTESIAN_POINT('Ctrl Pts',(1.62769405447016,-7.41461315340646,14.));
#41474=CARTESIAN_POINT('Ctrl Pts',(1.82072584398294,-7.35830742188736,14.));
#41475=CARTESIAN_POINT('Ctrl Pts',(2.01102139547125,-7.29457501043332,14.));
#41476=CARTESIAN_POINT('Ctrl Pts',(2.20118757483255,-7.23088592735752,14.));
#41477=CARTESIAN_POINT('Ctrl Pts',(2.38862189549973,-7.15977999794911,14.));
#41478=CARTESIAN_POINT('Ctrl Pts',(2.5728645161657,-7.08137730080356,14.));
#41479=CARTESIAN_POINT('Ctrl Pts',(2.75481210731953,-7.00395123166693,14.));
#41480=CARTESIAN_POINT('Ctrl Pts',(2.93364759189136,-6.91940872604078,14.));
#41481=CARTESIAN_POINT('Ctrl Pts',(3.10890286121801,-6.8278218581436,14.));
#41482=CARTESIAN_POINT('Ctrl Pts',(3.22552198713502,-6.76687772493333,14.));
#41483=CARTESIAN_POINT('Ctrl Pts',(3.34055530131138,-6.70281353757012,14.));
#41484=CARTESIAN_POINT('Ctrl Pts',(3.4538566828235,-6.63564064344417,14.));
#41485=CARTESIAN_POINT('Ctrl Pts',(3.58559135870223,-6.55753921769436,14.));
#41486=CARTESIAN_POINT('Ctrl Pts',(3.7149850616138,-6.4752353085306,14.));
#41487=CARTESIAN_POINT('Ctrl Pts',(3.84185984001097,-6.38886310040951,14.));
#41488=CARTESIAN_POINT('Ctrl Pts',(3.8806004845034,-6.36248973407842,14.));
#41489=CARTESIAN_POINT('Ctrl Pts',(3.9191061724772,-6.33573698326292,14.));
#41490=CARTESIAN_POINT('Ctrl Pts',(3.95737155880359,-6.30860848485213,14.));
#41491=CARTESIAN_POINT('Ctrl Pts',(3.97728091824068,-6.29449361296134,14.));
#41492=CARTESIAN_POINT('Ctrl Pts',(3.99712719655925,-6.28027559103114,14.));
#41493=CARTESIAN_POINT('Ctrl Pts',(4.01690323841346,-6.26595955416571,14.));
#41494=CARTESIAN_POINT('Ctrl Pts',(4.17634630198718,-6.1505374291072,14.));
#41495=CARTESIAN_POINT('Ctrl Pts',(4.33089390508824,-6.028990302188,14.));
#41496=CARTESIAN_POINT('Ctrl Pts',(4.48025060970871,-5.90169460830379,14.));
#41497=CARTESIAN_POINT('Ctrl Pts',(4.63343708131297,-5.77113483031398,14.));
#41498=CARTESIAN_POINT('Ctrl Pts',(4.78116368530107,-5.63452748859809,14.));
#41499=CARTESIAN_POINT('Ctrl Pts',(4.92307572794479,-5.49223569146564,14.));
#41500=CARTESIAN_POINT('Ctrl Pts',(5.06165950670547,-5.35328106460028,14.));
#41501=CARTESIAN_POINT('Ctrl Pts',(5.19469858019819,-5.2089048176019,14.));
#41502=CARTESIAN_POINT('Ctrl Pts',(5.32182205546165,-5.05941318879982,14.));
#41503=CARTESIAN_POINT('Ctrl Pts',(5.45352507612924,-4.9045362155504,14.));
#41504=CARTESIAN_POINT('Ctrl Pts',(5.57887944752641,-4.74416823716401,14.));
#41505=CARTESIAN_POINT('Ctrl Pts',(5.69741932593274,-4.57862308077917,14.));
#41506=CARTESIAN_POINT('Ctrl Pts',(5.75668926513591,-4.49585050258675,14.));
#41507=CARTESIAN_POINT('Ctrl Pts',(5.81425468118815,-4.41178326119413,14.));
#41508=CARTESIAN_POINT('Ctrl Pts',(5.87005158672204,-4.32645875741048,14.));
#41509=CARTESIAN_POINT('Ctrl Pts',(5.89510682009737,-4.2881443502856,14.));
#41510=CARTESIAN_POINT('Ctrl Pts',(5.91980539685357,-4.24957641531242,14.));
#41511=CARTESIAN_POINT('Ctrl Pts',(5.94414125164539,-4.21075828020098,14.));
#41512=CARTESIAN_POINT('Ctrl Pts',(5.95731830661959,-4.18973955270054,14.));
#41513=CARTESIAN_POINT('Ctrl Pts',(5.97038804733471,-4.168648934416,14.));
#41514=CARTESIAN_POINT('Ctrl Pts',(5.98334356622436,-4.14749695834229,14.));
#41515=CARTESIAN_POINT('Ctrl Pts',(5.99974507579593,-4.12071884617363,14.));
#41516=CARTESIAN_POINT('Ctrl Pts',(6.01596626965895,-4.09383803111747,14.));
#41517=CARTESIAN_POINT('Ctrl Pts',(6.03200571335301,-4.06685583684996,14.));
#41518=CARTESIAN_POINT('Ctrl Pts',(6.13148189978188,-3.89951301384362,14.));
#41519=CARTESIAN_POINT('Ctrl Pts',(6.22397103273323,-3.72827256414755,14.));
#41520=CARTESIAN_POINT('Ctrl Pts',(6.30936757032185,-3.5536058398909,14.));
#41521=CARTESIAN_POINT('Ctrl Pts',(6.39501944450721,-3.37841686018694,14.));
#41522=CARTESIAN_POINT('Ctrl Pts',(6.47353642951823,-3.19978038055714,14.));
#41523=CARTESIAN_POINT('Ctrl Pts',(6.54476252176001,-3.01815506875983,14.));
#41524=CARTESIAN_POINT('Ctrl Pts',(6.58134872441318,-2.92486088041935,14.));
#41525=CARTESIAN_POINT('Ctrl Pts',(6.61601041067235,-2.83077788216511,14.));
#41526=CARTESIAN_POINT('Ctrl Pts',(6.64872113712823,-2.73596743377932,14.));
#41527=CARTESIAN_POINT('Ctrl Pts',(6.6641565496469,-2.69122864193718,14.));
#41528=CARTESIAN_POINT('Ctrl Pts',(6.67915749473869,-2.64632786691611,14.));
#41529=CARTESIAN_POINT('Ctrl Pts',(6.6937209078782,-2.60127154668905,14.));
#41530=CARTESIAN_POINT('Ctrl Pts',(6.70351950304729,-2.57095663098317,14.));
#41531=CARTESIAN_POINT('Ctrl Pts',(6.71312002789513,-2.54057130140322,14.));
#41532=CARTESIAN_POINT('Ctrl Pts',(6.72252150160785,-2.51011752011723,14.));
#41533=CARTESIAN_POINT('Ctrl Pts',(6.72982180473667,-2.48646996850992,14.));
#41534=CARTESIAN_POINT('Ctrl Pts',(6.73700164922378,-2.46278244924519,14.));
#41535=CARTESIAN_POINT('Ctrl Pts',(6.74405795301005,-2.43906513842396,14.));
#41536=CARTESIAN_POINT('Ctrl Pts',(6.79911253488915,-2.25401831077738,14.));
#41537=CARTESIAN_POINT('Ctrl Pts',(6.84669881313537,-2.06700471360453,14.));
#41538=CARTESIAN_POINT('Ctrl Pts',(6.88668373523586,-1.87847518436181,14.));
#41539=CARTESIAN_POINT('Ctrl Pts',(6.92645168310919,-1.69096869197288,14.));
#41540=CARTESIAN_POINT('Ctrl Pts',(6.95870064560547,-1.50196198674046,14.));
#41541=CARTESIAN_POINT('Ctrl Pts',(6.98324861503862,-1.31189363116468,14.));
#41542=CARTESIAN_POINT('Ctrl Pts',(7.00741036693461,-1.12481565458474,14.));
#41543=CARTESIAN_POINT('Ctrl Pts',(7.02411155235519,-0.936708550057791,
14.));
#41544=CARTESIAN_POINT('Ctrl Pts',(7.03312830125131,-0.747995340106631,
14.));
#41545=CARTESIAN_POINT('Ctrl Pts',(7.03429963262975,-0.723480328444643,
14.));
#41546=CARTESIAN_POINT('Ctrl Pts',(7.03534121362652,-0.698955102669467,
14.));
#41547=CARTESIAN_POINT('Ctrl Pts',(7.03625248964568,-0.674420604634066,
14.));
#41548=CARTESIAN_POINT('Ctrl Pts',(-7.92543898861653,-0.000149382597450273,
13.7673131746348));
#41549=CARTESIAN_POINT('Ctrl Pts',(-7.92557446574483,-0.15883239438947,
13.7720941892239));
#41550=CARTESIAN_POINT('Ctrl Pts',(-7.92090561055472,-0.317507367685049,
13.776875203813));
#41551=CARTESIAN_POINT('Ctrl Pts',(-7.91137809126235,-0.475890009351388,
13.7816562184022));
#41552=CARTESIAN_POINT('Ctrl Pts',(-7.83245902535478,-1.7878170443658,13.8212586787999));
#41553=CARTESIAN_POINT('Ctrl Pts',(-7.42017413564185,-3.07968643136085,
13.8608611391976));
#41554=CARTESIAN_POINT('Ctrl Pts',(-6.72456199968518,-4.19481298313701,
13.9004635995953));
#41555=CARTESIAN_POINT('Ctrl Pts',(-6.14178063209989,-5.12906203268961,
13.9336423997302));
#41556=CARTESIAN_POINT('Ctrl Pts',(-5.36013105826123,-5.93925477959532,
13.9668211998651));
#41557=CARTESIAN_POINT('Ctrl Pts',(-4.44940638321884,-6.55843917088993,
14.));
#41558=CARTESIAN_POINT('',(-4.10246908460462,-5.75649127412218,-9.32299418528667E-16));
#41559=CARTESIAN_POINT('Ctrl Pts',(-4.10246908460462,-5.75649127412218,
-4.85722573273506E-16));
#41560=CARTESIAN_POINT('Ctrl Pts',(-4.26444805314231,-5.65499654616439,
-4.4106029540016E-16));
#41561=CARTESIAN_POINT('Ctrl Pts',(-4.42206063548502,-5.5470406348928,-4.66377136522777E-16));
#41562=CARTESIAN_POINT('Ctrl Pts',(-4.57488596535248,-5.43284881268837,
-3.64291929955129E-16));
#41563=CARTESIAN_POINT('Ctrl Pts',(-4.7279374413068,-5.31848801303912,-2.54051805889774E-16));
#41564=CARTESIAN_POINT('Ctrl Pts',(-4.87618830111391,-5.19787277182883,
-1.22736874955051E-16));
#41565=CARTESIAN_POINT('Ctrl Pts',(-5.01939433701872,-5.07141828023167,
-1.11022302462516E-16));
#41566=CARTESIAN_POINT('Ctrl Pts',(-5.11357307205341,-4.98825611473475,
-1.033182723087E-16));
#41567=CARTESIAN_POINT('Ctrl Pts',(-5.20556947047894,-4.90256748118548,
2.24781300563221E-16));
#41568=CARTESIAN_POINT('Ctrl Pts',(-5.29530739400484,-4.81446023940099,
2.28983498828939E-16));
#41569=CARTESIAN_POINT('Ctrl Pts',(-5.35325244632467,-4.75756814145219,
2.31696917958756E-16));
#41570=CARTESIAN_POINT('Ctrl Pts',(-5.410255722498,-4.69966745324811,-9.24391999260675E-17));
#41571=CARTESIAN_POINT('Ctrl Pts',(-5.46629534973171,-4.64078562778477,
-4.85722573273506E-17));
#41572=CARTESIAN_POINT('Ctrl Pts',(-5.48682578374535,-4.61921393839368,
-3.25013550951246E-17));
#41573=CARTESIAN_POINT('Ctrl Pts',(-5.50722813752232,-4.59750918490477,
-9.10536588563158E-17));
#41574=CARTESIAN_POINT('Ctrl Pts',(-5.52749729586896,-4.57567699269403,
-8.32667268468867E-17));
#41575=CARTESIAN_POINT('Ctrl Pts',(-5.65993255342473,-4.43302913583735,
-3.23882281642257E-17));
#41576=CARTESIAN_POINT('Ctrl Pts',(-5.78644919432292,-4.28519877405637,
-5.70912284577127E-17));
#41577=CARTESIAN_POINT('Ctrl Pts',(-5.90680145533567,-4.13262192737494,
-9.71445146547012E-17));
#41578=CARTESIAN_POINT('Ctrl Pts',(-6.0276504790816,-3.97941530863324,-1.37363123711073E-16));
#41579=CARTESIAN_POINT('Ctrl Pts',(-6.14228463266651,-3.82142243224172,
-4.75715598069395E-16));
#41580=CARTESIAN_POINT('Ctrl Pts',(-6.25042286356285,-3.65904284819727,
-3.19189119579733E-16));
#41581=CARTESIAN_POINT('Ctrl Pts',(-6.35563422902385,-3.50105822408518,
-1.66899181079758E-16));
#41582=CARTESIAN_POINT('Ctrl Pts',(-6.45469683435067,-3.33892050695521,
-5.21246859396646E-16));
#41583=CARTESIAN_POINT('Ctrl Pts',(-6.54731588099908,-3.17296682181485,
-6.66133814775094E-16));
#41584=CARTESIAN_POINT('Ctrl Pts',(-6.56727385003151,-3.13720637481497,
-6.97354708028551E-16));
#41585=CARTESIAN_POINT('Ctrl Pts',(-6.58693247668688,-3.1012686417294,1.04004692438599E-16));
#41586=CARTESIAN_POINT('Ctrl Pts',(-6.60628856479337,-3.06515684386158,
8.32667268468867E-17));
#41587=CARTESIAN_POINT('Ctrl Pts',(-6.6188568578988,-3.04170873504589,6.98011531972333E-17));
#41588=CARTESIAN_POINT('Ctrl Pts',(-6.6312938824366,-3.01819411604075,-7.91234734162241E-17));
#41589=CARTESIAN_POINT('Ctrl Pts',(-6.6435963695148,-2.99461910387611,-8.32667268468867E-17));
#41590=CARTESIAN_POINT('Ctrl Pts',(-6.70027332772065,-2.88601017214828,
-1.02354493412573E-16));
#41591=CARTESIAN_POINT('Ctrl Pts',(-6.75411340828003,-2.77608610999039,
-1.33518598772074E-16));
#41592=CARTESIAN_POINT('Ctrl Pts',(-6.80505784431399,-2.66494979480104,
-1.11022302462516E-16));
#41593=CARTESIAN_POINT('Ctrl Pts',(-6.8859011242357,-2.48858854835737,-7.74867130424257E-17));
#41594=CARTESIAN_POINT('Ctrl Pts',(-6.95945491899237,-2.30917619159457,
3.04971634102744E-16));
#41595=CARTESIAN_POINT('Ctrl Pts',(-7.02573737023362,-2.12720445243301,
2.4980018054066E-16));
#41596=CARTESIAN_POINT('Ctrl Pts',(-7.09286231827722,-1.94291972385284,
1.93927458809757E-16));
#41597=CARTESIAN_POINT('Ctrl Pts',(-7.15253014845298,-1.75600954554244,
2.61861991801936E-16));
#41598=CARTESIAN_POINT('Ctrl Pts',(-7.20471497950316,-1.56695488902645,
4.16333634234434E-16));
#41599=CARTESIAN_POINT('Ctrl Pts',(-7.25719534398338,-1.37682957711156,
5.71680081345093E-16));
#41600=CARTESIAN_POINT('Ctrl Pts',(-7.30210793162369,-1.18453476783516,
-2.26663475651839E-16));
#41601=CARTESIAN_POINT('Ctrl Pts',(-7.33937802283127,-0.990539282908711,
-2.4980018054066E-16));
#41602=CARTESIAN_POINT('Ctrl Pts',(-7.36972363521549,-0.832586576083263,
-2.68638274456075E-16));
#41603=CARTESIAN_POINT('Ctrl Pts',(-7.3950019111505,-0.673505889728574,
2.62252831393826E-16));
#41604=CARTESIAN_POINT('Ctrl Pts',(-7.41514750937589,-0.513545051200431,
3.05311331771918E-16));
#41605=CARTESIAN_POINT('Ctrl Pts',(-7.41978506017856,-0.476721795479128,
3.1522347142427E-16));
#41606=CARTESIAN_POINT('Ctrl Pts',(-7.4241505193075,-0.439851888410535,
-2.15849517642311E-16));
#41607=CARTESIAN_POINT('Ctrl Pts',(-7.4282429147508,-0.402938341593615,
-2.22044604925031E-16));
#41608=CARTESIAN_POINT('Ctrl Pts',(-7.43102427808838,-0.377850349194206,
-2.26255045699889E-16));
#41609=CARTESIAN_POINT('Ctrl Pts',(-7.43367975165298,-0.35273976384182,
6.84940450236123E-16));
#41610=CARTESIAN_POINT('Ctrl Pts',(-7.43620823019086,-0.327615359508083,
6.66133814775094E-16));
#41611=CARTESIAN_POINT('Ctrl Pts',(-7.45623500882372,-0.12861786898675,
5.17176123592382E-16));
#41612=CARTESIAN_POINT('Ctrl Pts',(-7.46825515329086,0.0707954497941199,
5.08633511213826E-16));
#41613=CARTESIAN_POINT('Ctrl Pts',(-7.47226868254779,0.270127329357898,
3.88578058618805E-16));
#41614=CARTESIAN_POINT('Ctrl Pts',(-7.47631137746368,0.470907721003539,
2.6765018273676E-16));
#41615=CARTESIAN_POINT('Ctrl Pts',(-7.47223087939926,0.671606167152592,
-2.90044233826028E-16));
#41616=CARTESIAN_POINT('Ctrl Pts',(-7.45997809674896,0.871732927784226,
-3.88578058618805E-16));
#41617=CARTESIAN_POINT('Ctrl Pts',(-7.45874178840682,0.891925759952658,
-3.98520142229585E-16));
#41618=CARTESIAN_POINT('Ctrl Pts',(-7.45742223668918,0.912112782108578,
-5.92394325853002E-17));
#41619=CARTESIAN_POINT('Ctrl Pts',(-7.45601936233051,0.932293497244242,
-5.55111512312578E-17));
#41620=CARTESIAN_POINT('Ctrl Pts',(-7.44220469443973,1.13102111363738,-1.87972656354744E-17));
#41621=CARTESIAN_POINT('Ctrl Pts',(-7.42031449996691,1.32913694415759,-2.12031727035272E-16));
#41622=CARTESIAN_POINT('Ctrl Pts',(-7.39055416059426,1.52620370719721,-2.22044604925031E-16));
#41623=CARTESIAN_POINT('Ctrl Pts',(-7.36063263652316,1.72433780170694,-2.32111713469992E-16));
#41624=CARTESIAN_POINT('Ctrl Pts',(-7.32275536562233,1.92141211023425,5.3721443045487E-16));
#41625=CARTESIAN_POINT('Ctrl Pts',(-7.27707851263434,2.11697850450149,5.55111512312578E-16));
#41626=CARTESIAN_POINT('Ctrl Pts',(-7.25245833225854,2.22239031786722,5.64758179162703E-16));
#41627=CARTESIAN_POINT('Ctrl Pts',(-7.22557125362165,2.3273639139264,-6.15445996968898E-16));
#41628=CARTESIAN_POINT('Ctrl Pts',(-7.1964356368219,2.43182760644158,-6.10622663543836E-16));
#41629=CARTESIAN_POINT('Ctrl Pts',(-7.18741574955678,2.46416777401931,-6.09129442238959E-16));
#41630=CARTESIAN_POINT('Ctrl Pts',(-7.17818032873551,2.49645906127832,2.62623543107519E-16));
#41631=CARTESIAN_POINT('Ctrl Pts',(-7.1687298384034,2.52869931099089,2.77555756156289E-16));
#41632=CARTESIAN_POINT('Ctrl Pts',(-7.16155733462016,2.55316823322769,2.88888644802346E-16));
#41633=CARTESIAN_POINT('Ctrl Pts',(-7.15426051935625,2.57760900340121,6.20963924433363E-16));
#41634=CARTESIAN_POINT('Ctrl Pts',(-7.14684494823062,2.60200349713766,6.10622663543836E-16));
#41635=CARTESIAN_POINT('Ctrl Pts',(-7.08779443525734,2.7962579037715,5.28274756690613E-16));
#41636=CARTESIAN_POINT('Ctrl Pts',(-7.02114659736257,2.98782550259838,-1.80070095916221E-16));
#41637=CARTESIAN_POINT('Ctrl Pts',(-6.94715442945099,3.17626378280464,-1.66533453693773E-16));
#41638=CARTESIAN_POINT('Ctrl Pts',(-6.87263508283784,3.36604464629625,-1.52900365730218E-16));
#41639=CARTESIAN_POINT('Ctrl Pts',(-6.79066624250823,3.55265212440146,7.72926337156281E-16));
#41640=CARTESIAN_POINT('Ctrl Pts',(-6.70145334111822,3.73563167634114,6.66133814775094E-16));
#41641=CARTESIAN_POINT('Ctrl Pts',(-6.6123241367756,3.91843956198602,5.59441482149727E-16));
#41642=CARTESIAN_POINT('Ctrl Pts',(-6.51596425805218,4.09762701399909,3.57827323897638E-16));
#41643=CARTESIAN_POINT('Ctrl Pts',(-6.41252847447672,4.27272797583501,4.44089209850063E-16));
#41644=CARTESIAN_POINT('Ctrl Pts',(-6.36760697881687,4.34877319756825,4.81552192209496E-16));
#41645=CARTESIAN_POINT('Ctrl Pts',(-6.32135026893501,4.42404743802936,-4.14513171145246E-16));
#41646=CARTESIAN_POINT('Ctrl Pts',(-6.27376821910516,4.49851126261938,-4.44089209850063E-16));
#41647=CARTESIAN_POINT('Ctrl Pts',(-6.18645080840074,4.63515918715393,-4.99268523196803E-16));
#41648=CARTESIAN_POINT('Ctrl Pts',(-6.09467122636726,4.76907872895868,-1.98525553334617E-16));
#41649=CARTESIAN_POINT('Ctrl Pts',(-5.99860552186345,4.90011413024603,-2.22044604925031E-16));
#41650=CARTESIAN_POINT('Ctrl Pts',(-5.95657677614303,4.95744211830925,-2.32334189995837E-16));
#41651=CARTESIAN_POINT('Ctrl Pts',(-5.91372741630838,5.01421790698281,4.04725268970026E-17));
#41652=CARTESIAN_POINT('Ctrl Pts',(-5.8700711905739,5.07042766638301,5.55111512312578E-17));
#41653=CARTESIAN_POINT('Ctrl Pts',(-5.84847106648942,5.09823899815474,6.2951926200114E-17));
#41654=CARTESIAN_POINT('Ctrl Pts',(-5.82667340878159,5.12591175532134,1.17875647828567E-16));
#41655=CARTESIAN_POINT('Ctrl Pts',(-5.80467983186185,5.1534442149457,1.11022302462516E-16));
#41656=CARTESIAN_POINT('Ctrl Pts',(-5.78581483932773,5.17706018460606,1.05143844873007E-16));
#41657=CARTESIAN_POINT('Ctrl Pts',(-5.76680349838768,5.20057552886117,2.33129696379534E-16));
#41658=CARTESIAN_POINT('Ctrl Pts',(-5.74766328194096,5.22396929474179,2.22044604925031E-16));
#41659=CARTESIAN_POINT('Ctrl Pts',(-5.61867202042286,5.38162641324933,1.47339079272257E-16));
#41660=CARTESIAN_POINT('Ctrl Pts',(-5.48369056578089,5.53394270109696,-8.06489650850003E-16));
#41661=CARTESIAN_POINT('Ctrl Pts',(-5.34315344687823,5.68067077831208,-6.66133814775094E-16));
#41662=CARTESIAN_POINT('Ctrl Pts',(-5.20008363720417,5.83004311670153,-5.23248554918668E-16));
#41663=CARTESIAN_POINT('Ctrl Pts',(-5.05125577950163,5.97362456003765,2.85421131474252E-16));
#41664=CARTESIAN_POINT('Ctrl Pts',(-4.8970796282879,6.11113067320816,2.22044604925031E-16));
#41665=CARTESIAN_POINT('Ctrl Pts',(-4.74253899229358,6.248961861853,1.5851825118664E-16));
#41666=CARTESIAN_POINT('Ctrl Pts',(-4.58262427189498,6.38068947566403,-3.93198157072506E-16));
#41667=CARTESIAN_POINT('Ctrl Pts',(-4.41770596513535,6.50599578022417,-3.88578058618805E-16));
#41668=CARTESIAN_POINT('Ctrl Pts',(-4.2543231982024,6.63013536882073,-3.84000977494824E-16));
#41669=CARTESIAN_POINT('Ctrl Pts',(-4.08602906082971,6.74797310968672,-4.57848538427986E-16));
#41670=CARTESIAN_POINT('Ctrl Pts',(-3.91315002787191,6.85916237355816,-5.55111512312578E-16));
#41671=CARTESIAN_POINT('Ctrl Pts',(-3.76372415357097,6.95526745167325,-6.39179572280059E-16));
#41672=CARTESIAN_POINT('Ctrl Pts',(-3.61087228998677,7.04640519188708,2.86820439889053E-17));
#41673=CARTESIAN_POINT('Ctrl Pts',(-3.45478907940187,7.13232482552818,0.));
#41674=CARTESIAN_POINT('Ctrl Pts',(-4.10246908460462,-5.75649127412218,
-4.82469966756049E-16));
#41675=CARTESIAN_POINT('Ctrl Pts',(-3.30199626649145,-6.32576073711656,
0.0331788001348988));
#41676=CARTESIAN_POINT('Ctrl Pts',(-1.28363269872274,-7.20768574705846,
0.105960060667506));
#41677=CARTESIAN_POINT('Ctrl Pts',(2.14497044005655,-7.04780045183455,0.21834378159782));
#41678=CARTESIAN_POINT('Ctrl Pts',(5.24919481691,-5.16895421862038,0.337151162790942));
#41679=CARTESIAN_POINT('Ctrl Pts',(7.07998577213964,-2.03617489938541,0.455958543984065));
#41680=CARTESIAN_POINT('Ctrl Pts',(7.19320815162393,1.59058620557498,0.574765925177186));
#41681=CARTESIAN_POINT('Ctrl Pts',(5.56139171256912,4.83147080423204,0.693573306370309));
#41682=CARTESIAN_POINT('Ctrl Pts',(2.5804088453257,6.9002678057359,0.812380687563431));
#41683=CARTESIAN_POINT('Ctrl Pts',(-1.02656909712053,7.29509087359264,0.931188068756555));
#41684=CARTESIAN_POINT('Ctrl Pts',(-4.3845061645243,5.92016094290675,1.04999544994967));
#41685=CARTESIAN_POINT('Ctrl Pts',(-6.58353186552137,3.22573736676226,1.16387031672212));
#41686=CARTESIAN_POINT('Ctrl Pts',(-7.0679837071718,1.02621179261826,1.23814272309686));
#41687=CARTESIAN_POINT('Ctrl Pts',(-7.06887577069393,-0.000134259091651625,
1.27281266907389));
#41688=CARTESIAN_POINT('Origin',(0.,0.,-2.77281266907387));
#41689=CARTESIAN_POINT('',(4.10219162127161,-5.75636310115763,0.));
#41690=CARTESIAN_POINT('Origin',(0.,0.,0.));
#41691=CARTESIAN_POINT('Ctrl Pts',(4.1021916212716,-5.75636310115763,-1.66533453693773E-15));
#41692=CARTESIAN_POINT('Ctrl Pts',(5.05709396285032,-5.0758653083813,0.0396024603977058));
#41693=CARTESIAN_POINT('Ctrl Pts',(6.62078237616492,-3.2312072264826,0.11880738119312));
#41694=CARTESIAN_POINT('Ctrl Pts',(7.35993086199691,0.321887848378951,0.237614762386243));
#41695=CARTESIAN_POINT('Ctrl Pts',(6.31364411820374,3.79596318205578,0.356422143579365));
#41696=CARTESIAN_POINT('Ctrl Pts',(3.73567782192208,6.34961322753113,0.475229524772488));
#41697=CARTESIAN_POINT('Ctrl Pts',(0.25146363409415,7.3626457790994,0.594036905965609));
#41698=CARTESIAN_POINT('Ctrl Pts',(-3.29375929907944,6.58965400328772,0.712844287158733));
#41699=CARTESIAN_POINT('Ctrl Pts',(-6.03992954092638,4.21798341238717,0.831651668351853));
#41700=CARTESIAN_POINT('Ctrl Pts',(-6.9899282991103,1.70012972441635,0.919766016274316));
#41701=CARTESIAN_POINT('Ctrl Pts',(-7.06879097449385,0.263968838154456,
0.96827790379907));
#41702=CARTESIAN_POINT('Ctrl Pts',(-7.06852116118549,0.000181853424906647,
0.977187330926117));
#41703=CARTESIAN_POINT('Ctrl Pts',(4.59925989935307,-6.4538696437256,-0.494500505560915));
#41704=CARTESIAN_POINT('Ctrl Pts',(5.66986908899888,-5.69091498463918,-0.454898045163208));
#41705=CARTESIAN_POINT('Ctrl Pts',(7.42303180747073,-3.62273711110913,-0.375693124367793));
#41706=CARTESIAN_POINT('Ctrl Pts',(8.25174394586199,0.360891447747451,-0.256885743174671));
#41707=CARTESIAN_POINT('Ctrl Pts',(7.07867717857605,4.25592533320956,-0.138078361981549));
#41708=CARTESIAN_POINT('Ctrl Pts',(4.18833511193785,7.11900471502922,-0.0192709807884262));
#41709=CARTESIAN_POINT('Ctrl Pts',(0.281933833231448,8.25478783325497,0.0995364004046958));
#41710=CARTESIAN_POINT('Ctrl Pts',(-3.69286870555341,7.38813156625243,0.218343781597819));
#41711=CARTESIAN_POINT('Ctrl Pts',(-6.77179622435331,4.7290823432367,0.33715116279094));
#41712=CARTESIAN_POINT('Ctrl Pts',(-8.20791988552602,0.92281499234215,0.455958543984063));
#41713=CARTESIAN_POINT('Ctrl Pts',(-7.65284082860589,-3.10734050142714,
0.574765925177185));
#41714=CARTESIAN_POINT('Ctrl Pts',(-5.24121966776055,-6.38366107966517,
0.693573306370307));
#41715=CARTESIAN_POINT('Ctrl Pts',(-1.55810356768701,-8.11134070632496,
0.81238068756343));
#41716=CARTESIAN_POINT('Ctrl Pts',(2.50300088702735,-7.87124563541711,0.931188068756552));
#41717=CARTESIAN_POINT('Ctrl Pts',(5.95688938266422,-5.72162533208904,1.04999544994967));
#41718=CARTESIAN_POINT('Ctrl Pts',(7.96566506351131,-2.18396555594479,1.1688028311428));
#41719=CARTESIAN_POINT('Ctrl Pts',(8.0420086234621,1.88351347449462,1.28761021233592));
#41720=CARTESIAN_POINT('Ctrl Pts',(6.16739946160646,5.49406133107593,1.40641759352904));
#41721=CARTESIAN_POINT('Ctrl Pts',(2.79660877821874,7.77177618156632,1.52522497472216));
#41722=CARTESIAN_POINT('Ctrl Pts',(-1.2526257813883,8.16409545269238,1.64403235591529));
#41723=CARTESIAN_POINT('Ctrl Pts',(-4.99797933429252,6.57584430815122,1.76283973710841));
#41724=CARTESIAN_POINT('Ctrl Pts',(-7.53084707602691,3.39232488910422,1.88164711830153));
#41725=CARTESIAN_POINT('Ctrl Pts',(-8.23676744172077,-0.614156280905575,
2.00045449949465));
#41726=CARTESIAN_POINT('Ctrl Pts',(-6.94448753724244,-4.4716460803835,2.11926188068778));
#41727=CARTESIAN_POINT('Ctrl Pts',(-3.96750826828504,-7.2443359923163,2.2380692618809));
#41728=CARTESIAN_POINT('Ctrl Pts',(-0.0280305252716536,-8.25958474223567,
2.35687664307402));
#41729=CARTESIAN_POINT('Ctrl Pts',(3.91824728872815,-7.27109785459193,2.47568402426714));
#41730=CARTESIAN_POINT('Ctrl Pts',(6.91397710597332,-4.51867750606856,2.59449140546026));
#41731=CARTESIAN_POINT('Ctrl Pts',(8.23240924307313,-0.670047670383021,
2.71329878665339));
#41732=CARTESIAN_POINT('Ctrl Pts',(7.55369838796778,3.34113251602617,2.83210616784651));
#41733=CARTESIAN_POINT('Ctrl Pts',(5.04249653839076,6.54176998115001,2.95091354903963));
#41734=CARTESIAN_POINT('Ctrl Pts',(1.30800921702632,8.15540542917379,3.06972093023275));
#41735=CARTESIAN_POINT('Ctrl Pts',(-2.74379486597955,7.79057864085904,3.18852831142588));
#41736=CARTESIAN_POINT('Ctrl Pts',(-6.12996747624935,5.53579484501796,3.307335692619));
#41737=CARTESIAN_POINT('Ctrl Pts',(-8.02903938171325,1.9380537745105,3.42614307381212));
#41738=CARTESIAN_POINT('Ctrl Pts',(-7.98030484779208,-2.12984984501333,
3.54495045500524));
#41739=CARTESIAN_POINT('Ctrl Pts',(-5.99558663863968,-5.68106210884581,
3.66375783619837));
#41740=CARTESIAN_POINT('Ctrl Pts',(-2.5563678712721,-7.85407595664345,3.78256521739149));
#41741=CARTESIAN_POINT('Ctrl Pts',(1.50301347898698,-8.12172865269342,3.90137259858461));
#41742=CARTESIAN_POINT('Ctrl Pts',(5.19777096907156,-6.41908893684097,4.02017997977773));
#41743=CARTESIAN_POINT('Ctrl Pts',(7.63157415532434,-3.15920903673424,4.13898736097086));
#41744=CARTESIAN_POINT('Ctrl Pts',(8.21399405950708,0.867079821227378,4.25779474216397));
#41745=CARTESIAN_POINT('Ctrl Pts',(6.80373840668384,4.68301927386732,4.3766021233571));
#41746=CARTESIAN_POINT('Ctrl Pts',(3.74292845335315,7.36288071471193,4.49540950455022));
#41747=CARTESIAN_POINT('Ctrl Pts',(-0.225897988251801,8.25654261327956,
4.61421688574334));
#41748=CARTESIAN_POINT('Ctrl Pts',(-4.13992266152032,7.14720687979774,4.73302426693647));
#41749=CARTESIAN_POINT('Ctrl Pts',(-7.04962195596062,4.30399304182004,4.85183164812958));
#41750=CARTESIAN_POINT('Ctrl Pts',(-8.2491167803214,0.416651137785123,4.97063902932272));
#41751=CARTESIAN_POINT('Ctrl Pts',(-7.44741544408726,-3.57176833363641,
5.08944641051582));
#41752=CARTESIAN_POINT('Ctrl Pts',(-4.83900684573563,-6.69369394078645,
5.20825379170897));
#41753=CARTESIAN_POINT('Ctrl Pts',(-1.05667839891248,-8.19176150698183,
5.32706117290206));
#41754=CARTESIAN_POINT('Ctrl Pts',(2.98199515869051,-7.70254702676615,5.44586855409521));
#41755=CARTESIAN_POINT('Ctrl Pts',(6.29725099517214,-5.34473158631946,5.56467593528831));
#41756=CARTESIAN_POINT('Ctrl Pts',(8.08482394760204,-1.69030990125421,5.68348331648146));
#41757=CARTESIAN_POINT('Ctrl Pts',(7.91105739255604,2.37417285758257,5.80229069767456));
#41758=CARTESIAN_POINT('Ctrl Pts',(5.81810626274495,5.86269266987495,5.92109807886769));
#41759=CARTESIAN_POINT('Ctrl Pts',(2.31371046255249,7.92895136329341,6.0399054600608));
#41760=CARTESIAN_POINT('Ctrl Pts',(-1.75198039718303,8.07168449048177,6.15871284125393));
#41761=CARTESIAN_POINT('Ctrl Pts',(-5.39264921666282,6.25626567946273,6.27752022244705));
#41762=CARTESIAN_POINT('Ctrl Pts',(-7.72508720425954,2.92310682538001,6.39632760364018));
#41763=CARTESIAN_POINT('Ctrl Pts',(-8.18345609268867,-1.11918372264528,
6.51513498483329));
#41764=CARTESIAN_POINT('Ctrl Pts',(-6.6565577883739,-4.88996566818585,6.63394236602643));
#41765=CARTESIAN_POINT('Ctrl Pts',(-3.51481049554077,-7.47446539937364,
6.75274974721954));
#41766=CARTESIAN_POINT('Ctrl Pts',(0.479612963263723,-8.24569567904776,
6.87155712841267));
#41767=CARTESIAN_POINT('Ctrl Pts',(4.35768461784302,-7.01655974088526,6.99036450960579));
#41768=CARTESIAN_POINT('Ctrl Pts',(7.17860288757583,-4.08524006742388,7.10917189079891));
#41769=CARTESIAN_POINT('Ctrl Pts',(8.25802653192982,-0.162860750154332,
7.22797927199203));
#41770=CARTESIAN_POINT('Ctrl Pts',(7.33409255268801,3.79902780387349,7.34678665318516));
#41771=CARTESIAN_POINT('Ctrl Pts',(4.63094290118184,6.83929043629462,7.46559403437828));
#41772=CARTESIAN_POINT('Ctrl Pts',(0.804348716087926,8.22037401636477,7.5844014155714));
#41773=CARTESIAN_POINT('Ctrl Pts',(-3.21737660913659,7.60723429249936,7.70320879676452));
#41774=CARTESIAN_POINT('Ctrl Pts',(-6.45858180246632,5.14861602052904,7.82201617795764));
#41775=CARTESIAN_POINT('Ctrl Pts',(-8.13296603178495,1.44096819945123,7.94082355915076));
#41776=CARTESIAN_POINT('Ctrl Pts',(-7.83433171493839,-2.61625159461166,
8.05963094034389));
#41777=CARTESIAN_POINT('Ctrl Pts',(-5.6351261046702,-6.038781301758,8.17843832153702));
#41778=CARTESIAN_POINT('Ctrl Pts',(-2.0688659326293,-7.99633163261776,8.29724570273012));
#41779=CARTESIAN_POINT('Ctrl Pts',(1.99929119049366,-8.01401026712669,8.41605308392327));
#41780=CARTESIAN_POINT('Ctrl Pts',(5.5824298612325,-6.08752845335585,8.53486046511637));
#41781=CARTESIAN_POINT('Ctrl Pts',(7.81129782607728,-2.68424143815676,8.65366784630951));
#41782=CARTESIAN_POINT('Ctrl Pts',(8.14518240844654,1.37022967386143,8.77247522750261));
#41783=CARTESIAN_POINT('Ctrl Pts',(6.50308481027346,5.09228963987598,8.89128260869575));
#41784=CARTESIAN_POINT('Ctrl Pts',(3.28337003187236,7.57898456653659,9.01008998988886));
#41785=CARTESIAN_POINT('Ctrl Pts',(-0.732874566214402,8.22705419309936,
9.12889737108199));
#41786=CARTESIAN_POINT('Ctrl Pts',(-4.57132731007446,6.87927993689491,9.24770475227511));
#41787=CARTESIAN_POINT('Ctrl Pts',(-7.30079797677848,3.86262536732011,9.36651213346823));
#41788=CARTESIAN_POINT('Ctrl Pts',(-8.25913007562251,-0.09108358768139,
9.48531951466136));
#41789=CARTESIAN_POINT('Ctrl Pts',(-7.2138368364646,-4.02269610123163,9.60412689585447));
#41790=CARTESIAN_POINT('Ctrl Pts',(-4.41850138494165,-6.97842183715385,
9.7229342770476));
#41791=CARTESIAN_POINT('Ctrl Pts',(-0.551258692607032,-8.24121591027825,
9.84174165824072));
#41792=CARTESIAN_POINT('Ctrl Pts',(3.44971671421322,-7.50473053598029,9.96054903943385));
#41793=CARTESIAN_POINT('Ctrl Pts',(6.61380739416247,-4.94763353320742,10.079356420627));
#41794=CARTESIAN_POINT('Ctrl Pts',(8.17342012615973,-1.19026436865481,10.1981638018201));
#41795=CARTESIAN_POINT('Ctrl Pts',(7.75020034274994,2.8558572221355,10.3169711830132));
#41796=CARTESIAN_POINT('Ctrl Pts',(5.44681913324314,6.20916155014182,10.4357785642063));
#41797=CARTESIAN_POINT('Ctrl Pts',(1.82206572993403,8.05615307089917,10.5545859453995));
#41798=CARTESIAN_POINT('Ctrl Pts',(-2.24471207915242,7.94876050134495,10.6733933265926));
#41799=CARTESIAN_POINT('Ctrl Pts',(-5.76693350554978,5.91303676367643,10.7922007077857));
#41800=CARTESIAN_POINT('Ctrl Pts',(-7.89012452694981,2.4428386715046,10.9110080889788));
#41801=CARTESIAN_POINT('Ctrl Pts',(-8.09920918644618,-1.61998036434483,
11.029815470172));
#41802=CARTESIAN_POINT('Ctrl Pts',(-6.34346454837397,-5.28979993459502,
11.148622851365));
#41803=CARTESIAN_POINT('Ctrl Pts',(-3.04882584022707,-7.67633941566181,
11.2674302325582));
#41804=CARTESIAN_POINT('Ctrl Pts',(0.985443392390751,-8.20063577678695,
11.3862376137513));
#41805=CARTESIAN_POINT('Ctrl Pts',(4.78064878394765,-6.73549723709446,11.5050449949444));
#41806=CARTESIAN_POINT('Ctrl Pts',(7.4160917151457,-3.63635937556868,11.6238523761376));
#41807=CARTESIAN_POINT('Ctrl Pts',(8.25242636618214,0.344941823793669,11.7426597573307));
#41808=CARTESIAN_POINT('Ctrl Pts',(7.08676197563969,4.24256179795868,11.8614671385238));
#41809=CARTESIAN_POINT('Ctrl Pts',(4.20188310742518,7.11095661822702,11.9802745197169));
#41810=CARTESIAN_POINT('Ctrl Pts',(0.297647586663742,8.25426749886389,12.09908190091));
#41811=CARTESIAN_POINT('Ctrl Pts',(-3.67879587591356,7.39513262976418,12.2178892821032));
#41812=CARTESIAN_POINT('Ctrl Pts',(-6.76278097843589,4.74197415548668,12.3366966632963));
#41813=CARTESIAN_POINT('Ctrl Pts',(-8.20614810557995,0.938435308045864,
12.4555040444894));
#41814=CARTESIAN_POINT('Ctrl Pts',(-7.65874257797369,-3.09276307173143,
12.5743114256825));
#41815=CARTESIAN_POINT('Ctrl Pts',(-5.25336379582813,-6.37367269401289,
12.6931188068757));
#41816=CARTESIAN_POINT('Ctrl Pts',(-1.573542283851,-8.10835846930099,12.8119261880688));
#41817=CARTESIAN_POINT('Ctrl Pts',(2.48800937090492,-7.87599816595178,12.9307335692619));
#41818=CARTESIAN_POINT('Ctrl Pts',(5.94598906728439,-5.73295302344607,13.049540950455));
#41819=CARTESIAN_POINT('Ctrl Pts',(7.96148627945122,-2.19913167759206,13.1683483316481));
#41820=CARTESIAN_POINT('Ctrl Pts',(8.04559263830003,1.86820941418339,13.2871557128413));
#41821=CARTESIAN_POINT('Ctrl Pts',(6.17782291561185,5.48229084249603,13.4059630940344));
#41822=CARTESIAN_POINT('Ctrl Pts',(2.81144855713387,7.76647514340256,13.5247704752275));
#41823=CARTESIAN_POINT('Ctrl Pts',(-1.23717676555208,8.16639239144963,13.6435778564206));
#41824=CARTESIAN_POINT('Ctrl Pts',(-4.98526003051727,6.5854918732965,13.7623852376137));
#41825=CARTESIAN_POINT('Ctrl Pts',(-7.52478211903276,3.40635867929589,13.8811926188069));
#41826=CARTESIAN_POINT('Ctrl Pts',(-7.9994255260722,0.73696682530501,13.9603975396023));
#41827=CARTESIAN_POINT('Ctrl Pts',(-7.90416902665075,-0.574227305285002,
14.));
#41828=CARTESIAN_POINT('Ctrl Pts',(4.43357047332591,-6.22136746286961,-0.329667003707277));
#41829=CARTESIAN_POINT('Ctrl Pts',(5.46561071361603,-5.48589842588655,-0.29006454330957));
#41830=CARTESIAN_POINT('Ctrl Pts',(7.1556153303688,-3.49222714956696,-0.210859622514155));
#41831=CARTESIAN_POINT('Ctrl Pts',(7.95447291790696,0.347890247957953,-0.0920522413210329));
#41832=CARTESIAN_POINT('Ctrl Pts',(6.82366615845194,4.10260461615829,0.0267551398720893));
#41833=CARTESIAN_POINT('Ctrl Pts',(4.03744934859926,6.8625408858632,0.145562521065212));
#41834=CARTESIAN_POINT('Ctrl Pts',(0.271777100185677,7.95740714853644,0.264369902258334));
#41835=CARTESIAN_POINT('Ctrl Pts',(-3.55983223672874,7.12197237859753,0.383177283451457));
#41836=CARTESIAN_POINT('Ctrl Pts',(-6.52784066321101,4.55871603295351,0.501984664644578));
#41837=CARTESIAN_POINT('Ctrl Pts',(-7.91222762971306,0.889570363911394,
0.620792045837701));
#41838=CARTESIAN_POINT('Ctrl Pts',(-7.37714542714633,-2.99539782468805,
0.739599427030823));
#41839=CARTESIAN_POINT('Ctrl Pts',(-5.05240348919327,-6.15368817894034,
0.858406808223945));
#41840=CARTESIAN_POINT('Ctrl Pts',(-1.50197251802458,-7.81912773829268,
0.977214189417068));
#41841=CARTESIAN_POINT('Ctrl Pts',(2.41282968787957,-7.58768214911912,1.09602157061019));
#41842=CARTESIAN_POINT('Ctrl Pts',(5.74229103329506,-5.51550242580367,1.21482895180331));
#41843=CARTESIAN_POINT('Ctrl Pts',(7.67870009497725,-2.10528768008078,1.33363633299643));
#41844=CARTESIAN_POINT('Ctrl Pts',(7.75229336011844,1.81565945594976,1.45244371418956));
#41845=CARTESIAN_POINT('Ctrl Pts',(5.94521743683818,5.29613647176714,1.57125109538268));
#41846=CARTESIAN_POINT('Ctrl Pts',(2.69586028532517,7.4917961058771,1.6900584765758));
#41847=CARTESIAN_POINT('Ctrl Pts',(-1.20749964125124,7.8699819824408,1.80886585776893));
#41848=CARTESIAN_POINT('Ctrl Pts',(-4.81792594628742,6.33894796115095,1.92767323896204));
#41849=CARTESIAN_POINT('Ctrl Pts',(-7.25954652836689,3.27011558237369,2.04648062015517));
#41850=CARTESIAN_POINT('Ctrl Pts',(-7.94003594587077,-0.592031155580847,
2.16528800134829));
#41851=CARTESIAN_POINT('Ctrl Pts',(-6.69431073069572,-4.31055397237727,
2.28409538254141));
#41852=CARTESIAN_POINT('Ctrl Pts',(-3.82457784423514,-6.9833570742335,2.40290276373453));
#41853=CARTESIAN_POINT('Ctrl Pts',(-0.0270207189669029,-7.96203124773619,
2.52171014492766));
#41854=CARTESIAN_POINT('Ctrl Pts',(3.77709150312162,-7.00915483408896,2.64051752612078));
#41855=CARTESIAN_POINT('Ctrl Pts',(6.66489944493164,-4.3558910798247,2.7593249073139));
#41856=CARTESIAN_POINT('Ctrl Pts',(7.93583475236053,-0.64590904452883,2.87813228850702));
#41857=CARTESIAN_POINT('Ctrl Pts',(7.28157461638861,3.22076742664758,2.99693966970015));
#41858=CARTESIAN_POINT('Ctrl Pts',(4.86083940757555,6.30610116984171,3.11574705089327));
#41859=CARTESIAN_POINT('Ctrl Pts',(1.26088787551702,7.86160501907548,3.23455443208639));
#41860=CARTESIAN_POINT('Ctrl Pts',(-2.64494900676982,7.50992120212525,3.35336181327951));
#41861=CARTESIAN_POINT('Ctrl Pts',(-5.90913394760972,5.33636652599553,3.47216919447264));
#41862=CARTESIAN_POINT('Ctrl Pts',(-7.73979133837202,1.86823492875368,3.59097657566576));
#41863=CARTESIAN_POINT('Ctrl Pts',(-7.69281247756563,-2.05312150043904,
3.70978395685888));
#41864=CARTESIAN_POINT('Ctrl Pts',(-5.77959421146849,-5.47640050227478,
3.828591338052));
#41865=CARTESIAN_POINT('Ctrl Pts',(-2.46427411389061,-7.57113101208551,
3.94739871924512));
#41866=CARTESIAN_POINT('Ctrl Pts',(1.44886706280393,-7.8291414564355,4.06620610043825));
#41867=CARTESIAN_POINT('Ctrl Pts',(5.01052004015424,-6.18783973917938,4.18501348163137));
#41868=CARTESIAN_POINT('Ctrl Pts',(7.3566448908013,-3.04539778373894,4.30382086282449));
#41869=CARTESIAN_POINT('Ctrl Pts',(7.91808298013935,0.835843065522612,4.42262824401762));
#41870=CARTESIAN_POINT('Ctrl Pts',(6.55863212086575,4.51431239655639,4.54143562521073));
#41871=CARTESIAN_POINT('Ctrl Pts',(3.60808857027019,7.09763119495797,4.66024300640386));
#41872=CARTESIAN_POINT('Ctrl Pts',(-0.21775995977915,7.95909871219548,4.77905038759697));
#41873=CARTESIAN_POINT('Ctrl Pts',(-3.99078096816209,6.88972706097348,4.8978577687901));
#41874=CARTESIAN_POINT('Ctrl Pts',(-6.79565765710552,4.14894067419358,5.01666514998322));
#41875=CARTESIAN_POINT('Ctrl Pts',(-7.95194039662654,0.401641181969633,
5.13547253117635));
#41876=CARTESIAN_POINT('Ctrl Pts',(-7.1791205407072,-3.44309453436157,5.25427991236947));
#41877=CARTESIAN_POINT('Ctrl Pts',(-4.66468047924256,-6.4525520328881,5.3730872935626));
#41878=CARTESIAN_POINT('Ctrl Pts',(-1.01861130958887,-7.89665136057889,
5.49189467475571));
#41879=CARTESIAN_POINT('Ctrl Pts',(2.87456807757934,-7.42506094775773,5.61070205594884));
#41880=CARTESIAN_POINT('Ctrl Pts',(6.07039103818519,-5.15218636639589,5.72950943714195));
#41881=CARTESIAN_POINT('Ctrl Pts',(7.79356625207644,-1.62941608714592,5.84831681833509));
#41882=CARTESIAN_POINT('Ctrl Pts',(7.62605967828794,2.28864271867535,5.9671241995282));
#41883=CARTESIAN_POINT('Ctrl Pts',(5.60850760810599,5.65148777937031,6.08593158072133));
#41884=CARTESIAN_POINT('Ctrl Pts',(2.23035849573119,7.64330901449592,6.20473896191444));
#41885=CARTESIAN_POINT('Ctrl Pts',(-1.68886488886813,7.78090014700762,6.32354634310758));
#41886=CARTESIAN_POINT('Ctrl Pts',(-5.19837775276918,6.03088222817104,6.44235372430068));
#41887=CARTESIAN_POINT('Ctrl Pts',(-7.44678911002407,2.81780121040889,6.56116110549382));
#41888=CARTESIAN_POINT('Ctrl Pts',(-7.88864515080064,-1.07886486424589,
6.67996848668693));
#41889=CARTESIAN_POINT('Ctrl Pts',(-6.41675371915234,-4.71380349805753,
6.79877586788007));
#41890=CARTESIAN_POINT('Ctrl Pts',(-3.38818861585914,-7.20519601495458,
6.91758324907317));
#41891=CARTESIAN_POINT('Ctrl Pts',(0.462334792789065,-7.94864254133568,
7.0363906302663));
#41892=CARTESIAN_POINT('Ctrl Pts',(4.2006979984873,-6.76378651615052,7.15519801145943));
#41893=CARTESIAN_POINT('Ctrl Pts',(6.9199920201433,-3.93806832745547,7.27400539265254));
#41894=CARTESIAN_POINT('Ctrl Pts',(7.96052917232528,-0.156993653098285,
7.39281277384567));
#41895=CARTESIAN_POINT('Ctrl Pts',(7.06988013328202,3.66216692841534,7.51162015503879));
#41896=CARTESIAN_POINT('Ctrl Pts',(4.4641120875178,6.59290338019847,7.63042753623192));
#41897=CARTESIAN_POINT('Ctrl Pts',(0.775371863287522,7.92423309754179,7.74923491742504));
#41898=CARTESIAN_POINT('Ctrl Pts',(-3.10146985558348,7.33318187729323,7.86804229861817));
#41899=CARTESIAN_POINT('Ctrl Pts',(-6.22590986497684,4.96313591026265,7.98684967981127));
#41900=CARTESIAN_POINT('Ctrl Pts',(-7.83997400628658,1.38905697914291,8.10565706100441));
#41901=CARTESIAN_POINT('Ctrl Pts',(-7.55209806135921,-2.52200051192882,
8.22446444219752));
#41902=CARTESIAN_POINT('Ctrl Pts',(-5.43211935351772,-5.82123277662844,
8.34327182339065));
#41903=CARTESIAN_POINT('Ctrl Pts',(-1.99433454792699,-7.70826189367614,
8.46207920458377));
#41904=CARTESIAN_POINT('Ctrl Pts',(1.92726625233771,-7.72530365119423,8.58088658577689));
#41905=CARTESIAN_POINT('Ctrl Pts',(5.38132150471746,-5.86822380055671,8.69969396697001));
#41906=CARTESIAN_POINT('Ctrl Pts',(7.52989397379399,-2.58754100527426,8.81850134816314));
#41907=CARTESIAN_POINT('Ctrl Pts',(7.85175028508863,1.32086682567376,8.93730872935625));
#41908=CARTESIAN_POINT('Ctrl Pts',(6.2688096413986,4.90883870079905,9.05611611054938));
#41909=CARTESIAN_POINT('Ctrl Pts',(3.16508584965159,7.30594985439198,9.17492349174251));
#41910=CARTESIAN_POINT('Ctrl Pts',(-0.706472586573508,7.93067261932902,
9.29373087293562));
#41911=CARTESIAN_POINT('Ctrl Pts',(-4.40664416218472,6.63145224957837,9.41253825412875));
#41912=CARTESIAN_POINT('Ctrl Pts',(-7.03778500234691,3.72347337459204,9.53134563532187));
#41913=CARTESIAN_POINT('Ctrl Pts',(-7.96159296059536,-0.0878022798854391,
9.65015301651499));
#41914=CARTESIAN_POINT('Ctrl Pts',(-6.95395665768722,-3.87777752244279,
9.76896039770813));
#41915=CARTESIAN_POINT('Ctrl Pts',(-4.25932382716235,-6.72702253942422,
9.88776777890122));
#41916=CARTESIAN_POINT('Ctrl Pts',(-0.531399467781868,-7.94432415729598,
10.0065751600944));
#41917=CARTESIAN_POINT('Ctrl Pts',(3.32543985340467,-7.23437084285444,10.1253825412875));
#41918=CARTESIAN_POINT('Ctrl Pts',(6.37554341800685,-4.76939386459785,10.2441899224806));
#41919=CARTESIAN_POINT('Ctrl Pts',(7.87897073234035,-1.14738481316572,10.3629973036737));
#41920=CARTESIAN_POINT('Ctrl Pts',(7.47099754175875,2.75297429003208,10.4818046848669));
#41921=CARTESIAN_POINT('Ctrl Pts',(5.25059618528844,5.98547503625344,10.60061206606));
#41922=CARTESIAN_POINT('Ctrl Pts',(1.75642538092503,7.76592825049012,10.7194194472531));
#41923=CARTESIAN_POINT('Ctrl Pts',(-2.16384579541766,7.66240452366244,10.8382268284462));
#41924=CARTESIAN_POINT('Ctrl Pts',(-5.55917836159592,5.70001821528151,10.9570342096394));
#41925=CARTESIAN_POINT('Ctrl Pts',(-7.60588092411773,2.35483483040497,11.0758415908324));
#41926=CARTESIAN_POINT('Ctrl Pts',(-7.80743325928778,-1.56162018844322,
11.1946489720256));
#41927=CARTESIAN_POINT('Ctrl Pts',(-6.1149397371991,-5.09923364042129,11.3134563532187));
#41928=CARTESIAN_POINT('Ctrl Pts',(-2.93899116800185,-7.39979747204398,
11.4322637344118));
#41929=CARTESIAN_POINT('Ctrl Pts',(0.949942561030821,-7.90520593271468,
11.5510711156049));
#41930=CARTESIAN_POINT('Ctrl Pts',(4.60842478043762,-6.49284935555622,11.6698784967981));
#41931=CARTESIAN_POINT('Ctrl Pts',(7.14892525651175,-3.50535866872642,11.7886858779912));
#41932=CARTESIAN_POINT('Ctrl Pts',(7.95513075387362,0.33251521298068,11.9074932591843));
#41933=CARTESIAN_POINT('Ctrl Pts',(6.83145969878857,4.08972250542654,12.0263006403774));
#41934=CARTESIAN_POINT('Ctrl Pts',(4.05050927434379,6.85478272365244,12.1451080215706));
#41935=CARTESIAN_POINT('Ctrl Pts',(0.286924761932817,7.9569055593149,12.2639154027637));
#41936=CARTESIAN_POINT('Ctrl Pts',(-3.54626638410621,7.12872122713987,12.3827227839568));
#41937=CARTESIAN_POINT('Ctrl Pts',(-6.51915019366069,4.57114341461708,12.5015301651499));
#41938=CARTESIAN_POINT('Ctrl Pts',(-7.91051967855875,0.904627954046215,
12.620337546343));
#41939=CARTESIAN_POINT('Ctrl Pts',(-7.38283456459684,-2.98134555034603,
12.7391449275362));
#41940=CARTESIAN_POINT('Ctrl Pts',(-5.06411012217399,-6.14405962724437,
12.8579523087293));
#41941=CARTESIAN_POINT('Ctrl Pts',(-1.51685505078607,-7.81625293706308,
12.9767596899224));
#41942=CARTESIAN_POINT('Ctrl Pts',(2.39837824467233,-7.59226346861687,13.0955670711156));
#41943=CARTESIAN_POINT('Ctrl Pts',(5.73178340435573,-5.52642203439951,13.2143744523086));
#41944=CARTESIAN_POINT('Ctrl Pts',(7.67467185260159,-2.1199074386075,13.3331818335018));
#41945=CARTESIAN_POINT('Ctrl Pts',(7.75574825997389,1.80090672803206,13.4519892146949));
#41946=CARTESIAN_POINT('Ctrl Pts',(5.9552653834469,5.28479001782315,13.570796595888));
#41947=CARTESIAN_POINT('Ctrl Pts',(2.71016545769389,7.48668603886737,13.6896039770812));
#41948=CARTESIAN_POINT('Ctrl Pts',(-1.19260717986564,7.87219617343589,13.8084113582743));
#41949=CARTESIAN_POINT('Ctrl Pts',(-4.80566485843997,6.34824797047931,13.9272187394674));
#41950=CARTESIAN_POINT('Ctrl Pts',(-7.25370006288338,3.28364380195341,14.0460261206605));
#41951=CARTESIAN_POINT('Ctrl Pts',(-7.71124432888689,0.710417421062149,
14.1252310414559));
#41952=CARTESIAN_POINT('Ctrl Pts',(-7.61941946739412,-0.553540630753928,
14.1648335018536));
#41953=CARTESIAN_POINT('Ctrl Pts',(4.26788104729875,-5.98886528201362,-0.16483350185364));
#41954=CARTESIAN_POINT('Ctrl Pts',(5.26135233823317,-5.28088186713393,-0.125231041455932));
#41955=CARTESIAN_POINT('Ctrl Pts',(6.88819885326686,-3.36171718802478,-0.0460261206605175));
#41956=CARTESIAN_POINT('Ctrl Pts',(7.65720188995193,0.334889048168454,0.0727812605326049));
#41957=CARTESIAN_POINT('Ctrl Pts',(6.56865513832785,3.94928389910703,0.191588641725727));
#41958=CARTESIAN_POINT('Ctrl Pts',(3.88656358526067,6.60607705669717,0.310396022918849));
#41959=CARTESIAN_POINT('Ctrl Pts',(0.261620367139915,7.66002646381791,0.429203404111972));
#41960=CARTESIAN_POINT('Ctrl Pts',(-3.42679576790409,6.85581319094263,0.548010785305094));
#41961=CARTESIAN_POINT('Ctrl Pts',(-6.28388510206869,4.38834972267034,0.666818166498216));
#41962=CARTESIAN_POINT('Ctrl Pts',(-7.61653537390012,0.856325735480628,
0.785625547691338));
#41963=CARTESIAN_POINT('Ctrl Pts',(-7.10145002568676,-2.88345514794895,
0.904432928884462));
#41964=CARTESIAN_POINT('Ctrl Pts',(-4.86358731062599,-5.9237152782155,1.02324031007758));
#41965=CARTESIAN_POINT('Ctrl Pts',(-1.44584146836215,-7.52691477026041,
1.14204769127071));
#41966=CARTESIAN_POINT('Ctrl Pts',(2.32265848873178,-7.30411866282113,1.26085507246383));
#41967=CARTESIAN_POINT('Ctrl Pts',(5.5276926839259,-5.30937951951831,1.37966245365695));
#41968=CARTESIAN_POINT('Ctrl Pts',(7.39173512644319,-2.02660980421676,1.49846983485007));
#41969=CARTESIAN_POINT('Ctrl Pts',(7.46257809677478,1.74780543740488,1.6172772160432));
#41970=CARTESIAN_POINT('Ctrl Pts',(5.72303541206989,5.09821161245836,1.73608459723632));
#41971=CARTESIAN_POINT('Ctrl Pts',(2.59511179243159,7.21181603018786,1.85489197842944));
#41972=CARTESIAN_POINT('Ctrl Pts',(-1.16237350111417,7.57586851218925,1.97369935962256));
#41973=CARTESIAN_POINT('Ctrl Pts',(-4.63787255828232,6.10205161415066,2.09250674081568));
#41974=CARTESIAN_POINT('Ctrl Pts',(-6.98824598070687,3.14790627564318,2.21131412200881));
#41975=CARTESIAN_POINT('Ctrl Pts',(-7.64330445002077,-0.569906030256128,
2.33012150320193));
#41976=CARTESIAN_POINT('Ctrl Pts',(-6.44413392414899,-4.14946186437103,
2.44892888439505));
#41977=CARTESIAN_POINT('Ctrl Pts',(-3.68164742018524,-6.72237815615069,
2.56773626558817));
#41978=CARTESIAN_POINT('Ctrl Pts',(-0.0260109126621464,-7.66447775323672,
2.6865436467813));
#41979=CARTESIAN_POINT('Ctrl Pts',(3.63593571751508,-6.74721181358599,2.80535102797442));
#41980=CARTESIAN_POINT('Ctrl Pts',(6.41582178388996,-4.19310465358082,2.92415840916754));
#41981=CARTESIAN_POINT('Ctrl Pts',(7.63926026164792,-0.62177041867464,3.04296579036066));
#41982=CARTESIAN_POINT('Ctrl Pts',(7.00945084480946,3.10040233726899,3.16177317155378));
#41983=CARTESIAN_POINT('Ctrl Pts',(4.67918227676032,6.0704323585334,3.28058055274691));
#41984=CARTESIAN_POINT('Ctrl Pts',(1.21376653400774,7.56780460897718,3.39938793394003));
#41985=CARTESIAN_POINT('Ctrl Pts',(-2.5461031475601,7.22926376339145,3.51819531513315));
#41986=CARTESIAN_POINT('Ctrl Pts',(-5.68830041897008,5.13693820697311,3.63700269632627));
#41987=CARTESIAN_POINT('Ctrl Pts',(-7.45054329503082,1.79841608299685,3.75581007751939));
#41988=CARTESIAN_POINT('Ctrl Pts',(-7.40532010733917,-1.97639315586476,
3.87461745871252));
#41989=CARTESIAN_POINT('Ctrl Pts',(-5.56360178429729,-5.27173889570375,
3.99342483990564));
#41990=CARTESIAN_POINT('Ctrl Pts',(-2.37218035650913,-7.28818606752757,
4.11223222109876));
#41991=CARTESIAN_POINT('Ctrl Pts',(1.39472064662088,-7.53655426017759,4.23103960229189));
#41992=CARTESIAN_POINT('Ctrl Pts',(4.82326911123691,-5.95659054151778,4.34984698348501));
#41993=CARTESIAN_POINT('Ctrl Pts',(7.08171562627826,-2.93158653074365,4.46865436467813));
#41994=CARTESIAN_POINT('Ctrl Pts',(7.62217190077163,0.80460630981784,4.58746174587126));
#41995=CARTESIAN_POINT('Ctrl Pts',(6.31352583504767,4.34560551924548,4.70626912706437));
#41996=CARTESIAN_POINT('Ctrl Pts',(3.47324868718724,6.832381675204,4.8250765082575));
#41997=CARTESIAN_POINT('Ctrl Pts',(-0.209621931306498,7.66165481111141,
4.94388388945061));
#41998=CARTESIAN_POINT('Ctrl Pts',(-3.84163927480386,6.63224724214921,5.06269127064374));
#41999=CARTESIAN_POINT('Ctrl Pts',(-6.54169335825042,3.99388830656712,5.18149865183686));
#42000=CARTESIAN_POINT('Ctrl Pts',(-7.65476401293167,0.38663122615414,5.30030603302999));
#42001=CARTESIAN_POINT('Ctrl Pts',(-6.91082563732715,-3.31442073508673,
5.41911341422311));
#42002=CARTESIAN_POINT('Ctrl Pts',(-4.49035411274948,-6.21141012498974,
5.53792079541623));
#42003=CARTESIAN_POINT('Ctrl Pts',(-0.980544220265259,-7.60154121417596,
5.65672817660935));
#42004=CARTESIAN_POINT('Ctrl Pts',(2.76714099646817,-7.14757486874929,5.77553555780248));
#42005=CARTESIAN_POINT('Ctrl Pts',(5.84353108119824,-4.95964114647233,5.89434293899559));
#42006=CARTESIAN_POINT('Ctrl Pts',(7.50230855655086,-1.56852227303763,6.01315032018873));
#42007=CARTESIAN_POINT('Ctrl Pts',(7.34106196401981,2.20311257976813,6.13195770138183));
#42008=CARTESIAN_POINT('Ctrl Pts',(5.39890895346704,5.44028288886567,6.25076508257497));
#42009=CARTESIAN_POINT('Ctrl Pts',(2.14700652890988,7.35766666569841,6.36957246376809));
#42010=CARTESIAN_POINT('Ctrl Pts',(-1.62574938055321,7.49011580353348,6.48837984496121));
#42011=CARTESIAN_POINT('Ctrl Pts',(-5.00410628887554,5.80549877687935,6.60718722615433));
#42012=CARTESIAN_POINT('Ctrl Pts',(-7.1684910157886,2.71249559543777,6.72599460734745));
#42013=CARTESIAN_POINT('Ctrl Pts',(-7.59383420891262,-1.03854600584651,
6.84480198854057));
#42014=CARTESIAN_POINT('Ctrl Pts',(-6.17694964993078,-4.5376413279292,6.96360936973371));
#42015=CARTESIAN_POINT('Ctrl Pts',(-3.2615667361775,-6.93592663053551,7.08241675092681));
#42016=CARTESIAN_POINT('Ctrl Pts',(0.445056622314409,-7.65158940362362,
7.20122413211994));
#42017=CARTESIAN_POINT('Ctrl Pts',(4.04371137913158,-6.51101329141579,7.32003151331306));
#42018=CARTESIAN_POINT('Ctrl Pts',(6.66138115271077,-3.79089658748706,7.43883889450619));
#42019=CARTESIAN_POINT('Ctrl Pts',(7.66303181272074,-0.151126556042241,
7.55764627569931));
#42020=CARTESIAN_POINT('Ctrl Pts',(6.80566771387603,3.52530605295721,7.67645365689243));
#42021=CARTESIAN_POINT('Ctrl Pts',(4.29728127385376,6.34651632410231,7.79526103808556));
#42022=CARTESIAN_POINT('Ctrl Pts',(0.746395010487117,7.62809217871881,7.91406841927867));
#42023=CARTESIAN_POINT('Ctrl Pts',(-2.98556310203037,7.0591294620871,8.03287580047181));
#42024=CARTESIAN_POINT('Ctrl Pts',(-5.99323792748737,4.77765579999626,8.15168318166491));
#42025=CARTESIAN_POINT('Ctrl Pts',(-7.54698198078821,1.33714575883459,8.27049056285805));
#42026=CARTESIAN_POINT('Ctrl Pts',(-7.26986440778004,-2.42774942924598,
8.38929794405116));
#42027=CARTESIAN_POINT('Ctrl Pts',(-5.22911260236524,-5.60368425149886,
8.50810532524429));
#42028=CARTESIAN_POINT('Ctrl Pts',(-1.91980316322469,-7.42019215473452,
8.6269127064374));
#42029=CARTESIAN_POINT('Ctrl Pts',(1.85524131418177,-7.43659703526178,8.74572008763054));
#42030=CARTESIAN_POINT('Ctrl Pts',(5.1802131482024,-5.64891914775757,8.86452746882365));
#42031=CARTESIAN_POINT('Ctrl Pts',(7.2484901215107,-2.49084057239175,8.98333485001678));
#42032=CARTESIAN_POINT('Ctrl Pts',(7.55831816173071,1.27150397748608,9.10214223120989));
#42033=CARTESIAN_POINT('Ctrl Pts',(6.03453447252376,4.72538776172215,9.22094961240303));
#42034=CARTESIAN_POINT('Ctrl Pts',(3.04680166743081,7.03291514224736,9.33975699359614));
#42035=CARTESIAN_POINT('Ctrl Pts',(-0.68007060693261,7.63429104555869,9.45856437478927));
#42036=CARTESIAN_POINT('Ctrl Pts',(-4.24196101429499,6.38362456226184,9.57737175598239));
#42037=CARTESIAN_POINT('Ctrl Pts',(-6.77477202791534,3.58432138186396,9.69617913717551));
#42038=CARTESIAN_POINT('Ctrl Pts',(-7.6640558455682,-0.084520972089485,
9.81498651836863));
#42039=CARTESIAN_POINT('Ctrl Pts',(-6.69407647890986,-3.73285894365395,
9.93379389956175));
#42040=CARTESIAN_POINT('Ctrl Pts',(-4.10014626938305,-6.47562324169458,
10.0526012807549));
#42041=CARTESIAN_POINT('Ctrl Pts',(-0.511540242956711,-7.64743240431371,
10.171408661948));
#42042=CARTESIAN_POINT('Ctrl Pts',(3.20116299259612,-6.96401114972859,10.2902160431411));
#42043=CARTESIAN_POINT('Ctrl Pts',(6.13727944185122,-4.59115419598828,10.4090234243342));
#42044=CARTESIAN_POINT('Ctrl Pts',(7.58452133852098,-1.10450525767663,10.5278308055274));
#42045=CARTESIAN_POINT('Ctrl Pts',(7.19179474076756,2.65009135792866,10.6466381867205));
#42046=CARTESIAN_POINT('Ctrl Pts',(5.05437323733374,5.76178852236506,10.7654455679136));
#42047=CARTESIAN_POINT('Ctrl Pts',(1.69078503191604,7.47570343008108,10.8842529491067));
#42048=CARTESIAN_POINT('Ctrl Pts',(-2.0829795116829,7.3760485459799,11.0030603302999));
#42049=CARTESIAN_POINT('Ctrl Pts',(-5.35142321764206,5.4869996668866,11.121867711493));
#42050=CARTESIAN_POINT('Ctrl Pts',(-7.32163732128566,2.26683098930532,11.2406750926861));
#42051=CARTESIAN_POINT('Ctrl Pts',(-7.51565733212937,-1.5032600125416,11.3594824738792));
#42052=CARTESIAN_POINT('Ctrl Pts',(-5.88641492602424,-4.90866734624756,
11.4782898550723));
#42053=CARTESIAN_POINT('Ctrl Pts',(-2.82915649577662,-7.12325552842614,
11.5970972362655));
#42054=CARTESIAN_POINT('Ctrl Pts',(0.914441729670889,-7.60977608864241,
11.7159046174586));
#42055=CARTESIAN_POINT('Ctrl Pts',(4.43620077692759,-6.25020147401799,11.8347119986517));
#42056=CARTESIAN_POINT('Ctrl Pts',(6.8817587978778,-3.37435796188414,11.9535193798448));
#42057=CARTESIAN_POINT('Ctrl Pts',(7.6578351415651,0.320088602167681,12.072326761038));
#42058=CARTESIAN_POINT('Ctrl Pts',(6.57615742193745,3.93688321289441,12.1911341422311));
#42059=CARTESIAN_POINT('Ctrl Pts',(3.89913544126241,6.59860882907782,12.3099415234242));
#42060=CARTESIAN_POINT('Ctrl Pts',(0.276201937201886,7.65954361976593,12.4287489046173));
#42061=CARTESIAN_POINT('Ctrl Pts',(-3.41373689229886,6.86230982451555,12.5475562858105));
#42062=CARTESIAN_POINT('Ctrl Pts',(-6.27551940888551,4.40031267374749,12.6663636670036));
#42063=CARTESIAN_POINT('Ctrl Pts',(-7.61489125153754,0.870820600046571,
12.7851710481967));
#42064=CARTESIAN_POINT('Ctrl Pts',(-7.10692655121999,-2.86992802896064,
12.9039784293898));
#42065=CARTESIAN_POINT('Ctrl Pts',(-4.87485644851986,-5.91444656047583,
13.0227858105829));
#42066=CARTESIAN_POINT('Ctrl Pts',(-1.46016781772114,-7.52414740482518,
13.1415931917761));
#42067=CARTESIAN_POINT('Ctrl Pts',(2.30874711843974,-7.30852877128194,13.2604005729692));
#42068=CARTESIAN_POINT('Ctrl Pts',(5.51757774142707,-5.31989104535296,13.3792079541623));
#42069=CARTESIAN_POINT('Ctrl Pts',(7.38785742575197,-2.04068319962294,13.4980153353554));
#42070=CARTESIAN_POINT('Ctrl Pts',(7.46590388164774,1.73360404188074,13.6168227165485));
#42071=CARTESIAN_POINT('Ctrl Pts',(5.73270785128195,5.08728919315028,13.7356300977417));
#42072=CARTESIAN_POINT('Ctrl Pts',(2.60888235825391,7.20689693433218,13.8544374789348));
#42073=CARTESIAN_POINT('Ctrl Pts',(-1.14803759417921,7.57799995542215,13.9732448601279));
#42074=CARTESIAN_POINT('Ctrl Pts',(-4.62606968636267,6.11100406766213,14.092052241321));
#42075=CARTESIAN_POINT('Ctrl Pts',(-6.98261800673401,3.16092892461094,14.2108596225142));
#42076=CARTESIAN_POINT('Ctrl Pts',(-7.42306313170158,0.683868016819283,
14.2900645433096));
#42077=CARTESIAN_POINT('Ctrl Pts',(-7.33466990813749,-0.532853956222854,
14.3296670037073));
#42078=CARTESIAN_POINT('Ctrl Pts',(4.1021916212716,-5.75636310115763,-1.66533453693773E-15));
#42079=CARTESIAN_POINT('Ctrl Pts',(5.05709396285032,-5.0758653083813,0.0396024603977058));
#42080=CARTESIAN_POINT('Ctrl Pts',(6.62078237616492,-3.2312072264826,0.11880738119312));
#42081=CARTESIAN_POINT('Ctrl Pts',(7.35993086199691,0.321887848378951,0.237614762386243));
#42082=CARTESIAN_POINT('Ctrl Pts',(6.31364411820374,3.79596318205578,0.356422143579365));
#42083=CARTESIAN_POINT('Ctrl Pts',(3.73567782192208,6.34961322753113,0.475229524772488));
#42084=CARTESIAN_POINT('Ctrl Pts',(0.25146363409415,7.3626457790994,0.594036905965609));
#42085=CARTESIAN_POINT('Ctrl Pts',(-3.29375929907944,6.58965400328772,0.712844287158733));
#42086=CARTESIAN_POINT('Ctrl Pts',(-6.03992954092638,4.21798341238717,0.831651668351853));
#42087=CARTESIAN_POINT('Ctrl Pts',(-7.32084311808716,0.823081107049866,
0.950459049544977));
#42088=CARTESIAN_POINT('Ctrl Pts',(-6.8257546242272,-2.77151247120985,1.0692664307381));
#42089=CARTESIAN_POINT('Ctrl Pts',(-4.67477113205871,-5.69374237749066,
1.18807381193122));
#42090=CARTESIAN_POINT('Ctrl Pts',(-1.38971041869972,-7.23470180222814,
1.30688119312434));
#42091=CARTESIAN_POINT('Ctrl Pts',(2.23248728958399,-7.02055517652312,1.42568857431747));
#42092=CARTESIAN_POINT('Ctrl Pts',(5.31309433455675,-5.10325661323295,1.54449595551059));
#42093=CARTESIAN_POINT('Ctrl Pts',(7.10477015790912,-1.94793192835274,1.66330333670371));
#42094=CARTESIAN_POINT('Ctrl Pts',(7.17286283343114,1.67995141886001,1.78211071789683));
#42095=CARTESIAN_POINT('Ctrl Pts',(5.50085338730159,4.90028675314958,1.90091809908995));
#42096=CARTESIAN_POINT('Ctrl Pts',(2.49436329953803,6.93183595449864,2.01972548028308));
#42097=CARTESIAN_POINT('Ctrl Pts',(-1.1172473609771,7.28175504193768,2.1385328614762));
#42098=CARTESIAN_POINT('Ctrl Pts',(-4.45781917027722,5.86515526715037,2.25734024266932));
#42099=CARTESIAN_POINT('Ctrl Pts',(-6.71694543304686,3.02569696891267,2.37614762386244));
#42100=CARTESIAN_POINT('Ctrl Pts',(-7.34657295417076,-0.547780904931404,
2.49495500505557));
#42101=CARTESIAN_POINT('Ctrl Pts',(-6.19395711760227,-3.9883697563648,2.61376238624869));
#42102=CARTESIAN_POINT('Ctrl Pts',(-3.53871699613534,-6.46139923806788,
2.73256976744181));
#42103=CARTESIAN_POINT('Ctrl Pts',(-0.0250011063573954,-7.36692425873726,
2.85137714863493));
#42104=CARTESIAN_POINT('Ctrl Pts',(3.49477993190855,-6.48526879308302,2.97018452982806));
#42105=CARTESIAN_POINT('Ctrl Pts',(6.16674412284828,-4.03031822733696,3.08899191102118));
#42106=CARTESIAN_POINT('Ctrl Pts',(7.34268577093533,-0.597631792820449,
3.2077992922143));
#42107=CARTESIAN_POINT('Ctrl Pts',(6.73732707323029,2.98003724789039,3.32660667340742));
#42108=CARTESIAN_POINT('Ctrl Pts',(4.4975251459451,5.83476354722511,3.44541405460054));
#42109=CARTESIAN_POINT('Ctrl Pts',(1.16664519249845,7.27400419887887,3.56422143579367));
#42110=CARTESIAN_POINT('Ctrl Pts',(-2.44725728835037,6.94860632465767,3.68302881698679));
#42111=CARTESIAN_POINT('Ctrl Pts',(-5.46746689033045,4.93750988795068,3.80183619817991));
#42112=CARTESIAN_POINT('Ctrl Pts',(-7.16129525168959,1.72859723724002,3.92064357937304));
#42113=CARTESIAN_POINT('Ctrl Pts',(-7.11782773711273,-1.89966481129048,
4.03945096056615));
#42114=CARTESIAN_POINT('Ctrl Pts',(-5.34760935712609,-5.06707728913272,
4.15825834175928));
#42115=CARTESIAN_POINT('Ctrl Pts',(-2.28008659912764,-7.00524112296964,
4.2770657229524));
#42116=CARTESIAN_POINT('Ctrl Pts',(1.34057423043783,-7.24396706391966,4.39587310414552));
#42117=CARTESIAN_POINT('Ctrl Pts',(4.63601818231957,-5.72534134385619,4.51468048533865));
#42118=CARTESIAN_POINT('Ctrl Pts',(6.80678636175523,-2.81777527774835,4.63348786653177));
#42119=CARTESIAN_POINT('Ctrl Pts',(7.32626082140389,0.773369554113066,4.75229524772489));
#42120=CARTESIAN_POINT('Ctrl Pts',(6.06841954922959,4.17689864193457,4.87110262891801));
#42121=CARTESIAN_POINT('Ctrl Pts',(3.33840880410428,6.56713215545002,4.98991001011114));
#42122=CARTESIAN_POINT('Ctrl Pts',(-0.201483902833845,7.36421091002734,
5.10871739130425));
#42123=CARTESIAN_POINT('Ctrl Pts',(-3.69249758144563,6.37476742332494,5.22752477249739));
#42124=CARTESIAN_POINT('Ctrl Pts',(-6.28772905939532,3.83883593894067,5.34633215369049));
#42125=CARTESIAN_POINT('Ctrl Pts',(-7.35758762923681,0.371621270338646,
5.46513953488363));
#42126=CARTESIAN_POINT('Ctrl Pts',(-6.6425307339471,-3.18574693581189,5.58394691607674));
#42127=CARTESIAN_POINT('Ctrl Pts',(-4.3160277462564,-5.97026821709139,5.70275429726988));
#42128=CARTESIAN_POINT('Ctrl Pts',(-0.942477130941647,-7.30643106777301,
5.82156167846298));
#42129=CARTESIAN_POINT('Ctrl Pts',(2.659713915357,-6.87008878974086,5.94036905965612));
#42130=CARTESIAN_POINT('Ctrl Pts',(5.61667112421129,-4.76709592654876,6.05917644084923));
#42131=CARTESIAN_POINT('Ctrl Pts',(7.21105086102525,-1.50762845892934,6.17798382204236));
#42132=CARTESIAN_POINT('Ctrl Pts',(7.05606424975171,2.11758244086091,6.29679120323547));
#42133=CARTESIAN_POINT('Ctrl Pts',(5.18931029882807,5.22907799836104,6.41559858442861));
#42134=CARTESIAN_POINT('Ctrl Pts',(2.06365456208858,7.0720243169009,6.53440596562172));
#42135=CARTESIAN_POINT('Ctrl Pts',(-1.56263387223831,7.19933146005934,6.65321334681485));
#42136=CARTESIAN_POINT('Ctrl Pts',(-4.80983482498188,5.58011532558766,6.77202072800796));
#42137=CARTESIAN_POINT('Ctrl Pts',(-6.89019292155314,2.60718998046665,6.8908281092011));
#42138=CARTESIAN_POINT('Ctrl Pts',(-7.29902326702459,-0.998227147447127,
7.0096354903942));
#42139=CARTESIAN_POINT('Ctrl Pts',(-5.93714558070924,-4.36147915780088,
7.12844287158734));
#42140=CARTESIAN_POINT('Ctrl Pts',(-3.13494485649586,-6.66665724611644,
7.24725025278046));
#42141=CARTESIAN_POINT('Ctrl Pts',(0.427778451839743,-7.35453626591155,
7.36605763397357));
#42142=CARTESIAN_POINT('Ctrl Pts',(3.88672475977586,-6.25824006668105,7.48486501516671));
#42143=CARTESIAN_POINT('Ctrl Pts',(6.40277028527823,-3.64372484751866,7.60367239635982));
#42144=CARTESIAN_POINT('Ctrl Pts',(7.36553445311621,-0.145259458986194,
7.72247977755295));
#42145=CARTESIAN_POINT('Ctrl Pts',(6.54145529447003,3.38844517749906,7.84128715874606));
#42146=CARTESIAN_POINT('Ctrl Pts',(4.13045046018973,6.10012926800615,7.9600945399392));
#42147=CARTESIAN_POINT('Ctrl Pts',(0.71741815768671,7.33195125989582,8.0789019211323));
#42148=CARTESIAN_POINT('Ctrl Pts',(-2.86965634847726,6.78507704688097,8.19770930232544));
#42149=CARTESIAN_POINT('Ctrl Pts',(-5.76056598999791,4.59217568972987,8.31651668351855));
#42150=CARTESIAN_POINT('Ctrl Pts',(-7.25398995528984,1.28523453852627,8.43532406471168));
#42151=CARTESIAN_POINT('Ctrl Pts',(-6.98763075420087,-2.33349834656314,
8.55413144590481));
#42152=CARTESIAN_POINT('Ctrl Pts',(-5.02610585121275,-5.3861357263693,8.67293882709792));
#42153=CARTESIAN_POINT('Ctrl Pts',(-1.84527177852238,-7.1321224157929,8.79174620829105));
#42154=CARTESIAN_POINT('Ctrl Pts',(1.78321637602583,-7.14789041932932,8.91055358948417));
#42155=CARTESIAN_POINT('Ctrl Pts',(4.97910479168735,-5.42961449495844,9.02936097067729));
#42156=CARTESIAN_POINT('Ctrl Pts',(6.96708626922742,-2.39414013950925,9.14816835187041));
#42157=CARTESIAN_POINT('Ctrl Pts',(7.26488603837279,1.2221411292984,9.26697573306353));
#42158=CARTESIAN_POINT('Ctrl Pts',(5.80025930364893,4.54193682264524,9.38578311425666));
#42159=CARTESIAN_POINT('Ctrl Pts',(2.92851748521003,6.75988043010273,9.50459049544978));
#42160=CARTESIAN_POINT('Ctrl Pts',(-0.653668627291716,7.33790947178836,
9.6233978766429));
#42161=CARTESIAN_POINT('Ctrl Pts',(-4.07727786640525,6.1357968749453,9.74220525783602));
#42162=CARTESIAN_POINT('Ctrl Pts',(-6.51175905348377,3.44516938913589,9.86101263902915));
#42163=CARTESIAN_POINT('Ctrl Pts',(-7.36651873054104,-0.0812396642935325,
9.97982002022226));
#42164=CARTESIAN_POINT('Ctrl Pts',(-6.43419630013248,-3.58794036486512,
10.0986274014154));
#42165=CARTESIAN_POINT('Ctrl Pts',(-3.94096871160376,-6.22422394396494,
10.2174347826085));
#42166=CARTESIAN_POINT('Ctrl Pts',(-0.491681018131546,-7.35054065133146,
10.3362421638016));
#42167=CARTESIAN_POINT('Ctrl Pts',(3.07688613178757,-6.69365145660272,10.4550495449948));
#42168=CARTESIAN_POINT('Ctrl Pts',(5.8990154656956,-4.41291452737873,10.5738569261879));
#42169=CARTESIAN_POINT('Ctrl Pts',(7.2900719447016,-1.06162570218753,10.692664307381));
#42170=CARTESIAN_POINT('Ctrl Pts',(6.91259193977638,2.54720842582524,10.8114716885741));
#42171=CARTESIAN_POINT('Ctrl Pts',(4.85815028937904,5.53810200847668,10.9302790697673));
#42172=CARTESIAN_POINT('Ctrl Pts',(1.62514468290704,7.18547860967203,11.0490864509604));
#42173=CARTESIAN_POINT('Ctrl Pts',(-2.00211322794815,7.08969256829738,11.1678938321535));
#42174=CARTESIAN_POINT('Ctrl Pts',(-5.14366807368819,5.27398111849169,11.2867012133466));
#42175=CARTESIAN_POINT('Ctrl Pts',(-7.03739371845359,2.17882714820567,11.4055085945397));
#42176=CARTESIAN_POINT('Ctrl Pts',(-7.22388140497096,-1.44489983663997,
11.5243159757329));
#42177=CARTESIAN_POINT('Ctrl Pts',(-5.65789011484937,-4.71810105207384,
11.643123356926));
#42178=CARTESIAN_POINT('Ctrl Pts',(-2.71932182355139,-6.84671358480829,
11.7619307381191));
#42179=CARTESIAN_POINT('Ctrl Pts',(0.878940898310958,-7.31434624457016,
11.8807381193122));
#42180=CARTESIAN_POINT('Ctrl Pts',(4.26397677341757,-6.00755359247974,11.9995455005054));
#42181=CARTESIAN_POINT('Ctrl Pts',(6.61459233924385,-3.24335725504188,12.1183528816985));
#42182=CARTESIAN_POINT('Ctrl Pts',(7.36053952925658,0.307661991354685,12.2371602628916));
#42183=CARTESIAN_POINT('Ctrl Pts',(6.32085514508631,3.78404392036229,12.3559676440847));
#42184=CARTESIAN_POINT('Ctrl Pts',(3.74776160818102,6.3424349345032,12.4747750252778));
#42185=CARTESIAN_POINT('Ctrl Pts',(0.265479112470959,7.36218168021696,12.593582406471));
#42186=CARTESIAN_POINT('Ctrl Pts',(-3.28120740049152,6.59589842189123,12.7123897876641));
#42187=CARTESIAN_POINT('Ctrl Pts',(-6.03188862411031,4.22948193287789,12.8311971688572));
#42188=CARTESIAN_POINT('Ctrl Pts',(-7.31926282451633,0.837013246046923,
12.9500045500503));
#42189=CARTESIAN_POINT('Ctrl Pts',(-6.83101853784315,-2.75851050757525,
13.0688119312434));
#42190=CARTESIAN_POINT('Ctrl Pts',(-4.68560277486572,-5.6848334937073,13.1876193124366));
#42191=CARTESIAN_POINT('Ctrl Pts',(-1.40348058465622,-7.23204187258727,
13.3064266936297));
#42192=CARTESIAN_POINT('Ctrl Pts',(2.21911599220716,-7.02479407394702,13.4252340748228));
#42193=CARTESIAN_POINT('Ctrl Pts',(5.30337207849841,-5.11336005630641,13.5440414560159));
#42194=CARTESIAN_POINT('Ctrl Pts',(7.10104299890235,-1.96145896063838,13.6628488372091));
#42195=CARTESIAN_POINT('Ctrl Pts',(7.1760595033216,1.66630135572941,13.7816562184022));
#42196=CARTESIAN_POINT('Ctrl Pts',(5.51015031911699,4.88978836847741,13.9004635995953));
#42197=CARTESIAN_POINT('Ctrl Pts',(2.50759925881393,6.92710782979698,14.0192709807884));
#42198=CARTESIAN_POINT('Ctrl Pts',(-1.10346800849277,7.28380373740842,14.1380783619816));
#42199=CARTESIAN_POINT('Ctrl Pts',(-4.44647451428538,5.87376016484493,14.2568857431747));
#42200=CARTESIAN_POINT('Ctrl Pts',(-6.71153595058463,3.03821404726848,14.3756931243678));
#42201=CARTESIAN_POINT('Ctrl Pts',(-7.13488193451627,0.657318612576422,
14.4548980451632));
#42202=CARTESIAN_POINT('Ctrl Pts',(-7.04992034888086,-0.51216728169178,
14.4945005055609));
#42203=CARTESIAN_POINT('',(-7.90416902665076,-0.57422730528489,14.));
#42204=CARTESIAN_POINT('Ctrl Pts',(2.93403320825969,6.43108807842008,14.));
#42205=CARTESIAN_POINT('Ctrl Pts',(2.76504255556035,6.52067383231118,14.));
#42206=CARTESIAN_POINT('Ctrl Pts',(2.59273860581333,6.60318405968412,14.));
#42207=CARTESIAN_POINT('Ctrl Pts',(2.41754216546193,6.67839186611978,14.));
#42208=CARTESIAN_POINT('Ctrl Pts',(2.24288743377926,6.75336712947054,14.));
#42209=CARTESIAN_POINT('Ctrl Pts',(2.06535765963728,6.82108586425906,14.));
#42210=CARTESIAN_POINT('Ctrl Pts',(1.88543906684595,6.88157091887576,14.));
#42211=CARTESIAN_POINT('Ctrl Pts',(1.70341361000517,6.94276425930731,14.));
#42212=CARTESIAN_POINT('Ctrl Pts',(1.51894244701564,6.99655374698891,14.));
#42213=CARTESIAN_POINT('Ctrl Pts',(1.33250163756747,7.0429170614105,14.));
#42214=CARTESIAN_POINT('Ctrl Pts',(1.14527132784069,7.08947670543268,14.));
#42215=CARTESIAN_POINT('Ctrl Pts',(0.956053975526834,7.12854734578937,14.));
#42216=CARTESIAN_POINT('Ctrl Pts',(0.765314017071225,7.16005711178253,14.));
#42217=CARTESIAN_POINT('Ctrl Pts',(0.611878080828955,7.18540434623241,14.));
#42218=CARTESIAN_POINT('Ctrl Pts',(0.457456382235616,7.2058580443962,14.));
#42219=CARTESIAN_POINT('Ctrl Pts',(0.302286994143537,7.22135648777913,14.));
#42220=CARTESIAN_POINT('Ctrl Pts',(0.281945378131416,7.22338822475997,14.));
#42221=CARTESIAN_POINT('Ctrl Pts',(0.261593030742382,7.22533453564978,14.));
#42222=CARTESIAN_POINT('Ctrl Pts',(0.241239397075081,7.22719456829265,14.));
#42223=CARTESIAN_POINT('Ctrl Pts',(0.0463864417924064,7.24500135715949,
14.));
#42224=CARTESIAN_POINT('Ctrl Pts',(-0.148813863335687,7.25492811071152,
14.));
#42225=CARTESIAN_POINT('Ctrl Pts',(-0.343865896367492,7.25698779731808,
14.));
#42226=CARTESIAN_POINT('Ctrl Pts',(-0.540339607037362,7.25906249638231,
14.));
#42227=CARTESIAN_POINT('Ctrl Pts',(-0.736663568137468,7.25315522583491,
14.));
#42228=CARTESIAN_POINT('Ctrl Pts',(-0.93234903806384,7.23922981278962,14.));
#42229=CARTESIAN_POINT('Ctrl Pts',(-0.986489845986116,7.23537703254381,
14.));
#42230=CARTESIAN_POINT('Ctrl Pts',(-1.04058184869791,7.23091018259324,14.));
#42231=CARTESIAN_POINT('Ctrl Pts',(-1.09461482262646,7.22582780366122,14.));
#42232=CARTESIAN_POINT('Ctrl Pts',(-1.28889696859445,7.20755349051977,14.));
#42233=CARTESIAN_POINT('Ctrl Pts',(-1.48241602611913,7.18132540055054,14.));
#42234=CARTESIAN_POINT('Ctrl Pts',(-1.67474546639368,7.14734789612827,14.));
#42235=CARTESIAN_POINT('Ctrl Pts',(-1.86783518449381,7.11323607871085,14.));
#42236=CARTESIAN_POINT('Ctrl Pts',(-2.05972653856352,7.07131331315291,14.));
#42237=CARTESIAN_POINT('Ctrl Pts',(-2.24998149527249,7.02173429436054,14.));
#42238=CARTESIAN_POINT('Ctrl Pts',(-2.30504373785463,7.0073854857568,14.));
#42239=CARTESIAN_POINT('Ctrl Pts',(-2.35996883893649,6.99239506626978,14.));
#42240=CARTESIAN_POINT('Ctrl Pts',(-2.41474595378691,6.97676600288421,14.));
#42241=CARTESIAN_POINT('Ctrl Pts',(-2.44203939863075,6.96897860881207,14.));
#42242=CARTESIAN_POINT('Ctrl Pts',(-2.46929610147469,6.96103265538078,14.));
#42243=CARTESIAN_POINT('Ctrl Pts',(-2.49651470828259,6.95292847781968,14.));
#42244=CARTESIAN_POINT('Ctrl Pts',(-2.51941719524455,6.94610939915631,14.));
#42245=CARTESIAN_POINT('Ctrl Pts',(-2.54229321057616,6.93917809579522,14.));
#42246=CARTESIAN_POINT('Ctrl Pts',(-2.56512697365784,6.93213951209675,14.));
#42247=CARTESIAN_POINT('Ctrl Pts',(-2.7549248933863,6.87363366971651,14.));
#42248=CARTESIAN_POINT('Ctrl Pts',(-2.94205306639717,6.80764665211765,14.));
#42249=CARTESIAN_POINT('Ctrl Pts',(-3.12608192497131,6.73444312052763,14.));
#42250=CARTESIAN_POINT('Ctrl Pts',(-3.31147248647493,6.66069792680816,14.));
#42251=CARTESIAN_POINT('Ctrl Pts',(-3.49371837629268,6.57962887889023,14.));
#42252=CARTESIAN_POINT('Ctrl Pts',(-3.67237779134679,6.49145335616022,14.));
#42253=CARTESIAN_POINT('Ctrl Pts',(-3.85086973913998,6.40336048518,14.));
#42254=CARTESIAN_POINT('Ctrl Pts',(-4.02578261635796,6.30817424132695,14.));
#42255=CARTESIAN_POINT('Ctrl Pts',(-4.19666301580165,6.20606133279816,14.));
#42256=CARTESIAN_POINT('Ctrl Pts',(-4.31144240408791,6.13747267537916,14.));
#42257=CARTESIAN_POINT('Ctrl Pts',(-4.42440217223988,6.06575786401773,14.));
#42258=CARTESIAN_POINT('Ctrl Pts',(-4.53539929999993,5.99095543969761,14.));
#42259=CARTESIAN_POINT('Ctrl Pts',(-4.6664170622633,5.90266084645836,14.));
#42260=CARTESIAN_POINT('Ctrl Pts',(-4.79470072581212,5.81006464588512,14.));
#42261=CARTESIAN_POINT('Ctrl Pts',(-4.92009686878172,5.71333951420776,14.));
#42262=CARTESIAN_POINT('Ctrl Pts',(-4.94938301419314,5.69074945518235,14.));
#42263=CARTESIAN_POINT('Ctrl Pts',(-4.97851160360603,5.66793411403788,14.));
#42264=CARTESIAN_POINT('Ctrl Pts',(-5.00748057682806,5.64489556783237,14.));
#42265=CARTESIAN_POINT('Ctrl Pts',(-5.02640283917017,5.62984700494612,14.));
#42266=CARTESIAN_POINT('Ctrl Pts',(-5.0452569991305,5.614703208918,14.));
#42267=CARTESIAN_POINT('Ctrl Pts',(-5.06404247259783,5.5994647485729,14.));
#42268=CARTESIAN_POINT('Ctrl Pts',(-5.0845422812029,5.58283564837728,14.));
#42269=CARTESIAN_POINT('Ctrl Pts',(-5.10495401158589,5.56609887849884,14.));
#42270=CARTESIAN_POINT('Ctrl Pts',(-5.12527090278503,5.54926057344536,14.));
#42271=CARTESIAN_POINT('Ctrl Pts',(-5.27876145036398,5.42205013373652,14.));
#42272=CARTESIAN_POINT('Ctrl Pts',(-5.42695161912127,5.28895862038518,14.));
#42273=CARTESIAN_POINT('Ctrl Pts',(-5.56960113735066,5.15042741208114,14.));
#42274=CARTESIAN_POINT('Ctrl Pts',(-5.71675997622002,5.00751706780356,14.));
#42275=CARTESIAN_POINT('Ctrl Pts',(-5.85802295965456,4.85881742447612,14.));
#42276=CARTESIAN_POINT('Ctrl Pts',(-5.99310134761184,4.70476219817552,14.));
#42277=CARTESIAN_POINT('Ctrl Pts',(-6.12679686666241,4.55228411671349,14.));
#42278=CARTESIAN_POINT('Ctrl Pts',(-6.25443422790721,4.39455895812829,14.));
#42279=CARTESIAN_POINT('Ctrl Pts',(-6.37570151960029,4.2319651250009,14.));
#42280=CARTESIAN_POINT('Ctrl Pts',(-6.49885028909018,4.06684862741341,14.));
#42281=CARTESIAN_POINT('Ctrl Pts',(-6.6154304429211,3.89671076483844,14.));
#42282=CARTESIAN_POINT('Ctrl Pts',(-6.72507364482188,3.72191167969025,14.));
#42283=CARTESIAN_POINT('Ctrl Pts',(-6.77989524577227,3.63451213711615,14.));
#42284=CARTESIAN_POINT('Ctrl Pts',(-6.8329819009625,3.54594677032576,14.));
#42285=CARTESIAN_POINT('Ctrl Pts',(-6.88428295688164,3.45625783325501,14.));
#42286=CARTESIAN_POINT('Ctrl Pts',(-6.90360298603292,3.42248088953117,14.));
#42287=CARTESIAN_POINT('Ctrl Pts',(-6.9226697332359,3.38854457515301,14.));
#42288=CARTESIAN_POINT('Ctrl Pts',(-6.94148036875173,3.35445108984207,14.));
#42289=CARTESIAN_POINT('Ctrl Pts',(-6.95472025012042,3.33045436200255,14.));
#42290=CARTESIAN_POINT('Ctrl Pts',(-6.96783370790352,3.30637881270687,14.));
#42291=CARTESIAN_POINT('Ctrl Pts',(-6.98081173224686,3.28224040555493,14.));
#42292=CARTESIAN_POINT('Ctrl Pts',(-6.99835567955093,3.24960963434707,14.));
#42293=CARTESIAN_POINT('Ctrl Pts',(-7.01565566297557,3.2168576748347,14.));
#42294=CARTESIAN_POINT('Ctrl Pts',(-7.03270997223139,3.18398692053127,14.));
#42295=CARTESIAN_POINT('Ctrl Pts',(-7.12613862865058,3.00391100165421,14.));
#42296=CARTESIAN_POINT('Ctrl Pts',(-7.21219748995004,2.82027261069025,14.));
#42297=CARTESIAN_POINT('Ctrl Pts',(-7.29087218921779,2.63356828668566,14.));
#42298=CARTESIAN_POINT('Ctrl Pts',(-7.37042005988303,2.44479182415336,14.));
#42299=CARTESIAN_POINT('Ctrl Pts',(-7.44241921699479,2.25288041051982,14.));
#42300=CARTESIAN_POINT('Ctrl Pts',(-7.50681051535069,2.05831727163918,14.));
#42301=CARTESIAN_POINT('Ctrl Pts',(-7.54180528095381,1.95257796191906,14.));
#42302=CARTESIAN_POINT('Ctrl Pts',(-7.57455220017289,1.84605497185642,14.));
#42303=CARTESIAN_POINT('Ctrl Pts',(-7.60503595657932,1.73882316930943,14.));
#42304=CARTESIAN_POINT('Ctrl Pts',(-7.62917933121202,1.65389473900327,14.));
#42305=CARTESIAN_POINT('Ctrl Pts',(-7.65190299831561,1.56852164701574,14.));
#42306=CARTESIAN_POINT('Ctrl Pts',(-7.6731974479298,1.48274048861856,14.));
#42307=CARTESIAN_POINT('Ctrl Pts',(-7.68040437951521,1.45370856006032,14.));
#42308=CARTESIAN_POINT('Ctrl Pts',(-7.68744763881537,1.42462944784155,14.));
#42309=CARTESIAN_POINT('Ctrl Pts',(-7.69432342715027,1.39551958977078,14.));
#42310=CARTESIAN_POINT('Ctrl Pts',(-7.74209559420721,1.19326772641705,14.));
#42311=CARTESIAN_POINT('Ctrl Pts',(-7.78183126083143,0.989359506012121,
14.));
#42312=CARTESIAN_POINT('Ctrl Pts',(-7.81348695611449,0.784295778626206,
14.));
#42313=CARTESIAN_POINT('Ctrl Pts',(-7.84522934883263,0.578670430368129,
14.));
#42314=CARTESIAN_POINT('Ctrl Pts',(-7.86884766179871,0.371882565380943,
14.));
#42315=CARTESIAN_POINT('Ctrl Pts',(-7.88424943003973,0.164417795820874,
14.));
#42316=CARTESIAN_POINT('Ctrl Pts',(-7.89954884786313,-0.0416682940011354,
14.));
#42317=CARTESIAN_POINT('Ctrl Pts',(-7.90674070299934,-0.248423003209867,
14.));
#42318=CARTESIAN_POINT('Ctrl Pts',(-7.90568392850165,-0.455379271744865,
14.));
#42319=CARTESIAN_POINT('Ctrl Pts',(-7.90548167065186,-0.494988980311862,
14.));
#42320=CARTESIAN_POINT('Ctrl Pts',(-7.90497710617671,-0.534606081175834,
14.));
#42321=CARTESIAN_POINT('Ctrl Pts',(-7.90416902665075,-0.574227305285002,
14.));
#42322=CARTESIAN_POINT('Ctrl Pts',(3.45507168555155,7.13251860299055,1.38777878078145E-16));
#42323=CARTESIAN_POINT('Ctrl Pts',(3.6420087970317,7.02984949182691,9.74215697402965E-17));
#42324=CARTESIAN_POINT('Ctrl Pts',(3.82450583053849,6.9197446466761,9.77074144499948E-16));
#42325=CARTESIAN_POINT('Ctrl Pts',(4.00206481978707,6.8023508547206,7.66747776381749E-16));
#42326=CARTESIAN_POINT('Ctrl Pts',(4.17547768173782,6.68769829038464,5.61332676907285E-16));
#42327=CARTESIAN_POINT('Ctrl Pts',(4.34418082373008,6.56609255773603,6.25535711258445E-17));
#42328=CARTESIAN_POINT('Ctrl Pts',(4.50784061150571,6.43790653945084,1.11022302462516E-16));
#42329=CARTESIAN_POINT('Ctrl Pts',(4.61464463848975,6.3542526184603,1.42652892724929E-16));
#42330=CARTESIAN_POINT('Ctrl Pts',(4.71930009693716,6.26779542334385,5.52961652623665E-16));
#42331=CARTESIAN_POINT('Ctrl Pts',(4.82170530078264,6.17863067064047,5.27355936696949E-16));
#42332=CARTESIAN_POINT('Ctrl Pts',(4.88074840962393,6.12722152343917,5.12592613978494E-16));
#42333=CARTESIAN_POINT('Ctrl Pts',(4.93904333883909,6.07491220743105,5.36534324121204E-16));
#42334=CARTESIAN_POINT('Ctrl Pts',(4.99656940254868,6.02172027598176,4.78783679369599E-16));
#42335=CARTESIAN_POINT('Ctrl Pts',(5.02400664443905,5.99635021247181,4.51239322825865E-16));
#42336=CARTESIAN_POINT('Ctrl Pts',(5.05126896812563,5.97077935983458,2.70409761827241E-16));
#42337=CARTESIAN_POINT('Ctrl Pts',(5.0783540546327,5.94500958145069,2.70616862252382E-16));
#42338=CARTESIAN_POINT('Ctrl Pts',(5.09938650653718,5.92499850914687,2.70777682478303E-16));
#42339=CARTESIAN_POINT('Ctrl Pts',(5.12031166695779,5.90486781053517,5.18028363593499E-16));
#42340=CARTESIAN_POINT('Ctrl Pts',(5.14111885655612,5.88462789262779,5.27355936696949E-16));
#42341=CARTESIAN_POINT('Ctrl Pts',(5.28891173105196,5.74086433277962,5.93609422518019E-16));
#42342=CARTESIAN_POINT('Ctrl Pts',(5.43088438187667,5.59147180641874,1.17436207753861E-15));
#42343=CARTESIAN_POINT('Ctrl Pts',(5.56671584293328,5.43681933615198,1.12410081243297E-15));
#42344=CARTESIAN_POINT('Ctrl Pts',(5.70192563898127,5.28287466972178,1.07406957996898E-15));
#42345=CARTESIAN_POINT('Ctrl Pts',(5.83105073149007,5.12371752674162,1.15095222081023E-15));
#42346=CARTESIAN_POINT('Ctrl Pts',(5.95373293436354,4.95968187186966,1.16573417585641E-15));
#42347=CARTESIAN_POINT('Ctrl Pts',(6.07188941364143,4.80169746172905,1.17997082733635E-15));
#42348=CARTESIAN_POINT('Ctrl Pts',(6.18406970280772,4.63918724659927,6.53710017676321E-16));
#42349=CARTESIAN_POINT('Ctrl Pts',(6.2899117761523,4.47243030721014,6.38378239159465E-16));
#42350=CARTESIAN_POINT('Ctrl Pts',(6.30776551361993,4.44430127947401,6.35792031804469E-16));
#42351=CARTESIAN_POINT('Ctrl Pts',(6.32543880171542,4.41605138142731,4.74985180111043E-16));
#42352=CARTESIAN_POINT('Ctrl Pts',(6.34292977552621,4.38768191358574,4.71844785465692E-16));
#42353=CARTESIAN_POINT('Ctrl Pts',(6.35742061123199,4.36417851680525,4.69243046800403E-16));
#42354=CARTESIAN_POINT('Ctrl Pts',(6.37178685416811,4.34059204937566,4.85771739497528E-16));
#42355=CARTESIAN_POINT('Ctrl Pts',(6.3860185636023,4.31693826780559,4.71844785465692E-16));
#42356=CARTESIAN_POINT('Ctrl Pts',(6.45644594201099,4.19988459739906,4.02925526945434E-16));
#42357=CARTESIAN_POINT('Ctrl Pts',(6.52363145866076,4.08109952203915,7.5220568606171E-16));
#42358=CARTESIAN_POINT('Ctrl Pts',(6.5874832695581,3.96068897350107,6.93889390390723E-16));
#42359=CARTESIAN_POINT('Ctrl Pts',(6.68217425780676,3.7821224821769,6.06284321176324E-16));
#42360=CARTESIAN_POINT('Ctrl Pts',(6.76953599931651,3.59998206678033,1.56378908891375E-15));
#42361=CARTESIAN_POINT('Ctrl Pts',(6.84949791164232,3.414750736673,1.41553435639707E-15));
#42362=CARTESIAN_POINT('Ctrl Pts',(6.92987732361558,3.22855227092865,1.26650555161578E-15));
#42363=CARTESIAN_POINT('Ctrl Pts',(7.00277959908613,3.0392298331746,8.2787151976317E-16));
#42364=CARTESIAN_POINT('Ctrl Pts',(7.06808334347011,2.84725669514074,9.15933995315754E-16));
#42365=CARTESIAN_POINT('Ctrl Pts',(7.13316081883727,2.65594871916779,1.00369134579549E-15));
#42366=CARTESIAN_POINT('Ctrl Pts',(7.19069243071623,2.46200767909707,3.56302599425838E-16));
#42367=CARTESIAN_POINT('Ctrl Pts',(7.24050690007108,2.26589526878088,1.94289029309402E-16));
#42368=CARTESIAN_POINT('Ctrl Pts',(7.28067447006557,2.10776131553028,6.36504517637552E-17));
#42369=CARTESIAN_POINT('Ctrl Pts',(7.315823496763,1.94821528841226,8.453426307217E-16));
#42370=CARTESIAN_POINT('Ctrl Pts',(7.34583909427119,1.78750071388778,9.71445146547012E-16));
#42371=CARTESIAN_POINT('Ctrl Pts',(7.35704804173394,1.72748387691319,1.0185365454246E-15));
#42372=CARTESIAN_POINT('Ctrl Pts',(7.3675408759556,1.66730411324232,2.17326548184769E-16));
#42373=CARTESIAN_POINT('Ctrl Pts',(7.37731078948879,1.60697426365927,1.94289029309402E-16));
#42374=CARTESIAN_POINT('Ctrl Pts',(7.38106886176767,1.5837679236506,1.85427470733132E-16));
#42375=CARTESIAN_POINT('Ctrl Pts',(7.38471928344393,1.56054340131122,4.77709052170576E-16));
#42376=CARTESIAN_POINT('Ctrl Pts',(7.38826041896046,1.53731084403494,4.71844785465692E-16));
#42377=CARTESIAN_POINT('Ctrl Pts',(7.41886472277194,1.3365232046228,4.2116279404502E-16));
#42378=CARTESIAN_POINT('Ctrl Pts',(7.44134458470096,1.13492783993692,6.75143946583213E-16));
#42379=CARTESIAN_POINT('Ctrl Pts',(7.45560296537357,0.933000562371476,6.66133814775094E-16));
#42380=CARTESIAN_POINT('Ctrl Pts',(7.46986134604617,0.73107328480603,6.57123682966975E-16));
#42381=CARTESIAN_POINT('Ctrl Pts',(7.47589835898452,0.528813351042067,7.55757054193326E-16));
#42382=CARTESIAN_POINT('Ctrl Pts',(7.47356156794063,0.326692878441132,7.7715611723761E-16));
#42383=CARTESIAN_POINT('Ctrl Pts',(7.47125585823871,0.127260782939089,7.97159268077648E-16));
#42384=CARTESIAN_POINT('Ctrl Pts',(7.46079730105774,-0.0720362355310806,
1.05905070470954E-15));
#42385=CARTESIAN_POINT('Ctrl Pts',(7.44230228855497,-0.27072027972702,1.16573417585641E-15));
#42386=CARTESIAN_POINT('Ctrl Pts',(7.42387912549052,-0.468632476000395,
1.27200320297528E-15));
#42387=CARTESIAN_POINT('Ctrl Pts',(7.39748157902158,-0.665937128618222,
5.79302131420473E-16));
#42388=CARTESIAN_POINT('Ctrl Pts',(7.36317622914462,-0.862144580575266,
4.9960036108132E-16));
#42389=CARTESIAN_POINT('Ctrl Pts',(7.34534425788565,-0.964133502321923,
4.58171263780931E-16));
#42390=CARTESIAN_POINT('Ctrl Pts',(7.32537487422037,-1.06582562028994,7.21644966006352E-16));
#42391=CARTESIAN_POINT('Ctrl Pts',(7.30327255511682,-1.16714938005994,7.21644966006352E-16));
#42392=CARTESIAN_POINT('Ctrl Pts',(7.29547904052248,-1.20287722367765,7.21644966006352E-16));
#42393=CARTESIAN_POINT('Ctrl Pts',(7.28742029945016,-1.2385592476155,1.5456272759111E-16));
#42394=CARTESIAN_POINT('Ctrl Pts',(7.27909643303922,-1.27419224578704,1.66533453693773E-16));
#42395=CARTESIAN_POINT('Ctrl Pts',(7.27441311892008,-1.29424068424165,1.73268625524415E-16));
#42396=CARTESIAN_POINT('Ctrl Pts',(7.26964620235591,-1.31427208877122,4.46372318945195E-16));
#42397=CARTESIAN_POINT('Ctrl Pts',(7.2647980511884,-1.33427665732707,4.44089209850063E-16));
#42398=CARTESIAN_POINT('Ctrl Pts',(7.21840223365521,-1.52571629699151,4.22240321619022E-16));
#42399=CARTESIAN_POINT('Ctrl Pts',(7.16451638886665,-1.7149352220374,3.12106949810161E-16));
#42400=CARTESIAN_POINT('Ctrl Pts',(7.10329533865964,-1.90148669058875,3.88578058618805E-16));
#42401=CARTESIAN_POINT('Ctrl Pts',(7.04213056723852,-2.08786666763316,4.64978869692518E-16));
#42402=CARTESIAN_POINT('Ctrl Pts',(6.97364382047475,-2.27158476110692,9.69884134728085E-16));
#42403=CARTESIAN_POINT('Ctrl Pts',(6.89794024185636,-2.45217911765423,9.43689570931383E-16));
#42404=CARTESIAN_POINT('Ctrl Pts',(6.82314219117491,-2.63061329580456,9.17808333264654E-16));
#42405=CARTESIAN_POINT('Ctrl Pts',(6.74129861780265,-2.80599860597599,9.09181254042411E-16));
#42406=CARTESIAN_POINT('Ctrl Pts',(6.65246709843858,-2.97786432931071,9.43689570931383E-16));
#42407=CARTESIAN_POINT('Ctrl Pts',(6.61552124306282,-3.04934488265293,9.58041900984587E-16));
#42408=CARTESIAN_POINT('Ctrl Pts',(6.57736610796479,-3.12021626253885,5.33583017232773E-16));
#42409=CARTESIAN_POINT('Ctrl Pts',(6.53800374880911,-3.19044292966702,5.55111512312578E-16));
#42410=CARTESIAN_POINT('Ctrl Pts',(6.46524483331982,-3.32025263234427,5.91589444244136E-16));
#42411=CARTESIAN_POINT('Ctrl Pts',(6.3883617494256,-3.44786031881024,-2.27018868370244E-16));
#42412=CARTESIAN_POINT('Ctrl Pts',(6.30748276302585,-3.57309566094206,-2.22044604925031E-16));
#42413=CARTESIAN_POINT('Ctrl Pts',(6.27209820647596,-3.62788612312473,-2.19868364667751E-16));
#42414=CARTESIAN_POINT('Ctrl Pts',(6.23594866787022,-3.6822223312132,-3.68266482884187E-16));
#42415=CARTESIAN_POINT('Ctrl Pts',(6.19904427211388,-3.73608917380381,-3.88578058618805E-16));
#42416=CARTESIAN_POINT('Ctrl Pts',(6.17970531144325,-3.76431694258207,-3.9922190622124E-16));
#42417=CARTESIAN_POINT('Ctrl Pts',(6.16015905662018,-3.79241581180823,5.43707389881397E-16));
#42418=CARTESIAN_POINT('Ctrl Pts',(6.14040692779842,-3.82038354608065,5.55111512312578E-16));
#42419=CARTESIAN_POINT('Ctrl Pts',(6.12153607086139,-3.8471034564797,5.66006822121118E-16));
#42420=CARTESIAN_POINT('Ctrl Pts',(6.10247388896415,-3.87370824653046,1.02099134177972E-15));
#42421=CARTESIAN_POINT('Ctrl Pts',(6.08324096182102,-3.90016965047398,9.99200722162641E-16));
#42422=CARTESIAN_POINT('Ctrl Pts',(5.96996686583548,-4.05601652640207,8.708628607586E-16));
#42423=CARTESIAN_POINT('Ctrl Pts',(5.8506722262936,-4.20704035147389,-2.21077044790491E-16));
#42424=CARTESIAN_POINT('Ctrl Pts',(5.72571543255065,-4.35294139755716,-1.66533453693773E-16));
#42425=CARTESIAN_POINT('Ctrl Pts',(5.60007830524651,-4.49963680923906,-1.11692897266405E-16));
#42426=CARTESIAN_POINT('Ctrl Pts',(5.46871669315143,-4.6411540157118,-4.73134212314551E-17));
#42427=CARTESIAN_POINT('Ctrl Pts',(5.33195525691958,-4.77715417893452,0.));
#42428=CARTESIAN_POINT('Ctrl Pts',(5.19597017321587,-4.91238231114137,4.70448375195555E-17));
#42429=CARTESIAN_POINT('Ctrl Pts',(5.0546458490692,-5.04215629186066,2.36926123753037E-16));
#42430=CARTESIAN_POINT('Ctrl Pts',(4.90827039206033,-5.16610237423274,2.77555756156289E-16));
#42431=CARTESIAN_POINT('Ctrl Pts',(4.76469954653324,-5.28767360078646,3.17406908779753E-16));
#42432=CARTESIAN_POINT('Ctrl Pts',(4.61626873550147,-5.40363841496088,-2.02048309080252E-16));
#42433=CARTESIAN_POINT('Ctrl Pts',(4.46322798222506,-5.51359971846396,-2.77555756156289E-16));
#42434=CARTESIAN_POINT('Ctrl Pts',(4.34557184220504,-5.59813682537676,-3.35605096449897E-16));
#42435=CARTESIAN_POINT('Ctrl Pts',(4.22519056171548,-5.67912480220418,7.48609313291272E-17));
#42436=CARTESIAN_POINT('Ctrl Pts',(4.10219162127164,-5.7563631011576,5.55111512312578E-17));
#42437=CARTESIAN_POINT('Ctrl Pts',(-7.90416902665075,-0.574227305285002,
14.));
#42438=CARTESIAN_POINT('Ctrl Pts',(-7.91805025518235,-0.383153882615103,
13.9942289417884));
#42439=CARTESIAN_POINT('Ctrl Pts',(-7.92486895290159,-0.191581382856594,
13.9884578835768));
#42440=CARTESIAN_POINT('Ctrl Pts',(-7.92471172241511,-8.01339879119567E-6,
13.9826868253652));
#42441=CARTESIAN_POINT('Origin',(0.,0.,0.));
#42442=CARTESIAN_POINT('Origin',(0.,0.,14.));
#42443=CARTESIAN_POINT('Origin',(0.,0.,-8.));
#42444=CARTESIAN_POINT('',(-7.,-8.57252759403147E-16,-8.));
#42445=CARTESIAN_POINT('Origin',(0.,0.,-8.));
#42446=CARTESIAN_POINT('',(-6.,-7.34788079488412E-16,-8.));
#42447=CARTESIAN_POINT('Origin',(0.,0.,-8.));
#42448=CARTESIAN_POINT('Origin',(0.,0.,-10.));
#42449=CARTESIAN_POINT('',(-7.,-8.57252759403147E-16,-10.));
#42450=CARTESIAN_POINT('Origin',(0.,0.,-10.));
#42451=CARTESIAN_POINT('',(-6.,7.34788079488412E-16,-10.));
#42452=CARTESIAN_POINT('Origin',(0.,0.,-10.));
#42453=CARTESIAN_POINT('Origin',(0.,0.,-10.));
#42454=CARTESIAN_POINT('',(-7.,-8.57252759403147E-16,-10.));
#42455=CARTESIAN_POINT('Origin',(0.,0.,-26.));
#42456=CARTESIAN_POINT('',(-6.,-7.34788079488412E-16,-14.));
#42457=CARTESIAN_POINT('',(-6.,-7.34788079488412E-16,-26.));
#42458=CARTESIAN_POINT('Origin',(0.,0.,-14.));
#42459=CARTESIAN_POINT('Origin',(0.,0.,-14.));
#42460=CARTESIAN_POINT('',(-7.,-8.57252759403147E-16,-14.));
#42461=CARTESIAN_POINT('Origin',(0.,0.,-14.));
#42462=CARTESIAN_POINT('Origin',(0.,0.,-16.));
#42463=CARTESIAN_POINT('',(-7.,-8.57252759403147E-16,-16.));
#42464=CARTESIAN_POINT('Origin',(0.,0.,-16.));
#42465=CARTESIAN_POINT('',(-6.,7.34788079488412E-16,-16.));
#42466=CARTESIAN_POINT('Origin',(0.,0.,-16.));
#42467=CARTESIAN_POINT('Origin',(0.,0.,-16.));
#42468=CARTESIAN_POINT('',(-7.,-8.57252759403147E-16,-16.));
#42469=CARTESIAN_POINT('Origin',(0.,0.,-26.));
#42470=CARTESIAN_POINT('',(-6.,-7.34788079488412E-16,-20.));
#42471=CARTESIAN_POINT('',(-6.,-7.34788079488412E-16,-26.));
#42472=CARTESIAN_POINT('Origin',(0.,0.,-20.));
#42473=CARTESIAN_POINT('Origin',(0.,0.,-20.));
#42474=CARTESIAN_POINT('',(-7.,-8.57252759403147E-16,-20.));
#42475=CARTESIAN_POINT('Origin',(0.,0.,-20.));
#42476=CARTESIAN_POINT('Origin',(0.,0.,-22.));
#42477=CARTESIAN_POINT('',(-7.,-8.57252759403147E-16,-22.));
#42478=CARTESIAN_POINT('Origin',(0.,0.,-22.));
#42479=CARTESIAN_POINT('',(-6.,7.34788079488412E-16,-22.));
#42480=CARTESIAN_POINT('Origin',(0.,0.,-22.));
#42481=CARTESIAN_POINT('Origin',(0.,0.,-22.));
#42482=CARTESIAN_POINT('',(-7.,-8.57252759403147E-16,-22.));
#42483=CARTESIAN_POINT('Origin',(0.,0.,-26.));
#42484=CARTESIAN_POINT('',(-6.,-7.34788079488412E-16,-26.));
#42485=CARTESIAN_POINT('',(-6.,-7.34788079488412E-16,-26.));
#42486=CARTESIAN_POINT('Origin',(0.,0.,-26.));
#42487=CARTESIAN_POINT('Origin',(0.,0.,-26.));
#42488=CARTESIAN_POINT('',(-6.,-7.34788079488412E-16,-6.));
#42489=CARTESIAN_POINT('Origin',(0.,0.,-6.));
#42490=CARTESIAN_POINT('',(-6.,-7.34788079488412E-16,-26.));
#42491=CARTESIAN_POINT('Origin',(0.,0.,-26.));
#42492=CARTESIAN_POINT('',(-4.,-4.89858719658941E-16,-26.));
#42493=CARTESIAN_POINT('Origin',(0.,0.,-26.));
#42494=CARTESIAN_POINT('Origin',(0.,0.,0.));
#42495=CARTESIAN_POINT('',(-12.,-1.46957615897682E-15,0.));
#42496=CARTESIAN_POINT('Origin',(0.,0.,0.));
#42497=CARTESIAN_POINT('Origin',(0.,0.,-6.));
#42498=CARTESIAN_POINT('',(-12.,-1.46957615897682E-15,-6.));
#42499=CARTESIAN_POINT('',(-12.,-1.46957615897682E-15,-6.));
#42500=CARTESIAN_POINT('Origin',(0.,0.,-6.));
#42501=CARTESIAN_POINT('Origin',(0.,0.,-6.));
#42502=CARTESIAN_POINT('Origin',(0.,0.,0.));
#42503=CARTESIAN_POINT('',(-4.,-4.89858719658941E-16,14.));
#42504=CARTESIAN_POINT('Origin',(0.,0.,14.));
#42505=CARTESIAN_POINT('',(-4.,-4.89858719658941E-16,0.));
#42506=CARTESIAN_POINT('Origin',(0.,0.,14.));
#42507=CARTESIAN_POINT('',(0.,0.,0.));
#42508=CARTESIAN_POINT('Origin',(0.,0.,-50.));
#42509=CARTESIAN_POINT('',(-8.5,-1.04094977927525E-15,-48.));
#42510=CARTESIAN_POINT('Origin',(0.,0.,-48.));
#42511=CARTESIAN_POINT('',(-8.5,-1.04094977927525E-15,-50.));
#42512=CARTESIAN_POINT('',(-8.5,-1.04094977927525E-15,-50.));
#42513=CARTESIAN_POINT('Origin',(0.,0.,-50.));
#42514=CARTESIAN_POINT('Origin',(0.,0.,-50.));
#42515=CARTESIAN_POINT('',(-12.,-1.46957615897682E-15,-48.));
#42516=CARTESIAN_POINT('Origin',(0.,0.,-48.));
#42517=CARTESIAN_POINT('',(-12.,-1.46957615897682E-15,-50.));
#42518=CARTESIAN_POINT('',(-12.,-1.46957615897682E-15,-50.));
#42519=CARTESIAN_POINT('Origin',(0.,0.,-50.));
#42520=CARTESIAN_POINT('Origin',(0.,0.,-48.));
#42521=CARTESIAN_POINT('Origin',(0.,0.,-50.));
#42522=CARTESIAN_POINT('',(-24.,0.,0.));
#42523=CARTESIAN_POINT('',(-24.,0.,0.));
#42524=CARTESIAN_POINT('',(-24.,0.,0.));
#42525=CARTESIAN_POINT('',(-8.,-50.,-20.));
#42526=CARTESIAN_POINT('',(10.,0.,0.));
#42527=CARTESIAN_POINT('',(-24.,0.,0.));
#42528=CARTESIAN_POINT('',(-44.,-66.,41.));
#42529=CARTESIAN_POINT('',(-44.,-50.,-46.));
#42530=CARTESIAN_POINT('',(-24.,0.,-50.));
#42531=CARTESIAN_POINT('',(-24.,0.,0.));
#42532=CARTESIAN_POINT('',(324.,0.,0.));
#42533=CARTESIAN_POINT('',(324.,0.,0.));
#42534=CARTESIAN_POINT('',(324.,0.,0.));
#42535=CARTESIAN_POINT('',(-8.,-50.,0.));
#42536=CARTESIAN_POINT('',(-8.,-50.,20.));
#42537=CARTESIAN_POINT('',(-8.,-30.,-20.));
#42538=CARTESIAN_POINT('',(-8.,-30.,0.));
#42539=CARTESIAN_POINT('',(-8.,-30.,20.));
#42540=CARTESIAN_POINT('',(-8.,-10.,-20.));
#42541=CARTESIAN_POINT('',(-8.,-10.,0.));
#42542=CARTESIAN_POINT('',(-8.,-10.,20.));
#42543=CARTESIAN_POINT('',(-8.,10.,-20.));
#42544=CARTESIAN_POINT('',(-8.,10.,0.));
#42545=CARTESIAN_POINT('',(-8.,10.,20.));
#42546=CARTESIAN_POINT('',(-8.,30.,-20.));
#42547=CARTESIAN_POINT('',(-8.,30.,0.));
#42548=CARTESIAN_POINT('',(-8.,30.,20.));
#42549=CARTESIAN_POINT('',(-8.,50.,-20.));
#42550=CARTESIAN_POINT('',(-8.,50.,0.));
#42551=CARTESIAN_POINT('',(-8.,50.,20.));
#42552=CARTESIAN_POINT('',(20.,0.,0.));
#42553=CARTESIAN_POINT('',(30.,0.,0.));
#42554=CARTESIAN_POINT('',(40.,0.,0.));
#42555=CARTESIAN_POINT('',(50.,0.,0.));
#42556=CARTESIAN_POINT('',(60.,0.,0.));
#42557=CARTESIAN_POINT('',(70.,0.,0.));
#42558=CARTESIAN_POINT('',(80.,0.,0.));
#42559=CARTESIAN_POINT('',(90.,0.,0.));
#42560=CARTESIAN_POINT('',(100.,0.,0.));
#42561=CARTESIAN_POINT('',(110.,0.,0.));
#42562=CARTESIAN_POINT('',(120.,0.,0.));
#42563=CARTESIAN_POINT('',(130.,0.,0.));
#42564=CARTESIAN_POINT('',(140.,0.,0.));
#42565=CARTESIAN_POINT('',(150.,0.,0.));
#42566=CARTESIAN_POINT('',(160.,0.,0.));
#42567=CARTESIAN_POINT('',(170.,0.,0.));
#42568=CARTESIAN_POINT('',(180.,0.,0.));
#42569=CARTESIAN_POINT('',(190.,0.,0.));
#42570=CARTESIAN_POINT('',(200.,0.,0.));
#42571=CARTESIAN_POINT('',(210.,0.,0.));
#42572=CARTESIAN_POINT('',(220.,0.,0.));
#42573=CARTESIAN_POINT('',(230.,0.,0.));
#42574=CARTESIAN_POINT('',(240.,0.,0.));
#42575=CARTESIAN_POINT('',(250.,0.,0.));
#42576=CARTESIAN_POINT('',(260.,0.,0.));
#42577=CARTESIAN_POINT('',(270.,0.,0.));
#42578=CARTESIAN_POINT('',(280.,0.,0.));
#42579=CARTESIAN_POINT('',(290.,0.,0.));
#42580=CARTESIAN_POINT('',(324.,0.,0.));
#42581=CARTESIAN_POINT('',(-44.,66.,41.));
#42582=CARTESIAN_POINT('',(-3.99999999999999,-66.,41.));
#42583=CARTESIAN_POINT('',(-4.,66.,41.));
#42584=CARTESIAN_POINT('',(344.,66.,41.));
#42585=CARTESIAN_POINT('',(344.,-66.,41.));
#42586=CARTESIAN_POINT('',(304.,66.,41.));
#42587=CARTESIAN_POINT('',(304.,-66.,41.));
#42588=CARTESIAN_POINT('',(-44.,50.,-46.));
#42589=CARTESIAN_POINT('',(-3.99999999999999,-50.,-46.));
#42590=CARTESIAN_POINT('',(-3.99999999999999,50.,-46.));
#42591=CARTESIAN_POINT('',(344.,50.,-46.));
#42592=CARTESIAN_POINT('',(344.,-50.,-46.));
#42593=CARTESIAN_POINT('',(304.,50.,-46.));
#42594=CARTESIAN_POINT('',(304.,-50.,-46.));
#42595=CARTESIAN_POINT('',(324.,7.105427357601E-14,-50.));
#42596=CARTESIAN_POINT('',(324.,0.,0.));
#42597=UNCERTAINTY_MEASURE_WITH_UNIT(LENGTH_MEASURE(0.01),#42621,
'DISTANCE_ACCURACY_VALUE',
'Maximum model space distance between geometric entities at asserted c
onnectivities');
#42598=UNCERTAINTY_MEASURE_WITH_UNIT(LENGTH_MEASURE(0.01),#42621,
'DISTANCE_ACCURACY_VALUE',
'Maximum model space distance between geometric entities at asserted c
onnectivities');
#42599=UNCERTAINTY_MEASURE_WITH_UNIT(LENGTH_MEASURE(0.01),#42621,
'DISTANCE_ACCURACY_VALUE',
'Maximum model space distance between geometric entities at asserted c
onnectivities');
#42600=UNCERTAINTY_MEASURE_WITH_UNIT(LENGTH_MEASURE(0.01),#42621,
'DISTANCE_ACCURACY_VALUE',
'Maximum model space distance between geometric entities at asserted c
onnectivities');
#42601=UNCERTAINTY_MEASURE_WITH_UNIT(LENGTH_MEASURE(0.01),#42621,
'DISTANCE_ACCURACY_VALUE',
'Maximum model space distance between geometric entities at asserted c
onnectivities');
#42602=UNCERTAINTY_MEASURE_WITH_UNIT(LENGTH_MEASURE(0.01),#42621,
'DISTANCE_ACCURACY_VALUE',
'Maximum model space distance between geometric entities at asserted c
onnectivities');
#42603=UNCERTAINTY_MEASURE_WITH_UNIT(LENGTH_MEASURE(0.01),#42621,
'DISTANCE_ACCURACY_VALUE',
'Maximum model space distance between geometric entities at asserted c
onnectivities');
#42604=UNCERTAINTY_MEASURE_WITH_UNIT(LENGTH_MEASURE(0.01),#42621,
'DISTANCE_ACCURACY_VALUE',
'Maximum model space distance between geometric entities at asserted c
onnectivities');
#42605=UNCERTAINTY_MEASURE_WITH_UNIT(LENGTH_MEASURE(0.01),#42621,
'DISTANCE_ACCURACY_VALUE',
'Maximum model space distance between geometric entities at asserted c
onnectivities');
#42606=UNCERTAINTY_MEASURE_WITH_UNIT(LENGTH_MEASURE(0.01),#42621,
'DISTANCE_ACCURACY_VALUE',
'Maximum model space distance between geometric entities at asserted c
onnectivities');
#42607=UNCERTAINTY_MEASURE_WITH_UNIT(LENGTH_MEASURE(0.01),#42621,
'DISTANCE_ACCURACY_VALUE',
'Maximum model space distance between geometric entities at asserted c
onnectivities');
#42608=UNCERTAINTY_MEASURE_WITH_UNIT(LENGTH_MEASURE(0.01),#42621,
'DISTANCE_ACCURACY_VALUE',
'Maximum model space distance between geometric entities at asserted c
onnectivities');
#42609=(
GEOMETRIC_REPRESENTATION_CONTEXT(3)
GLOBAL_UNCERTAINTY_ASSIGNED_CONTEXT((#42597))
GLOBAL_UNIT_ASSIGNED_CONTEXT((#42621,#42623,#42624))
REPRESENTATION_CONTEXT('','3D')
);
#42610=(
GEOMETRIC_REPRESENTATION_CONTEXT(3)
GLOBAL_UNCERTAINTY_ASSIGNED_CONTEXT((#42598))
GLOBAL_UNIT_ASSIGNED_CONTEXT((#42621,#42623,#42624))
REPRESENTATION_CONTEXT('','3D')
);
#42611=(
GEOMETRIC_REPRESENTATION_CONTEXT(3)
GLOBAL_UNCERTAINTY_ASSIGNED_CONTEXT((#42599))
GLOBAL_UNIT_ASSIGNED_CONTEXT((#42621,#42623,#42624))
REPRESENTATION_CONTEXT('','3D')
);
#42612=(
GEOMETRIC_REPRESENTATION_CONTEXT(3)
GLOBAL_UNCERTAINTY_ASSIGNED_CONTEXT((#42600))
GLOBAL_UNIT_ASSIGNED_CONTEXT((#42621,#42623,#42624))
REPRESENTATION_CONTEXT('','3D')
);
#42613=(
GEOMETRIC_REPRESENTATION_CONTEXT(3)
GLOBAL_UNCERTAINTY_ASSIGNED_CONTEXT((#42601))
GLOBAL_UNIT_ASSIGNED_CONTEXT((#42621,#42623,#42624))
REPRESENTATION_CONTEXT('','3D')
);
#42614=(
GEOMETRIC_REPRESENTATION_CONTEXT(3)
GLOBAL_UNCERTAINTY_ASSIGNED_CONTEXT((#42602))
GLOBAL_UNIT_ASSIGNED_CONTEXT((#42621,#42623,#42624))
REPRESENTATION_CONTEXT('','3D')
);
#42615=(
GEOMETRIC_REPRESENTATION_CONTEXT(3)
GLOBAL_UNCERTAINTY_ASSIGNED_CONTEXT((#42603))
GLOBAL_UNIT_ASSIGNED_CONTEXT((#42621,#42623,#42624))
REPRESENTATION_CONTEXT('','3D')
);
#42616=(
GEOMETRIC_REPRESENTATION_CONTEXT(3)
GLOBAL_UNCERTAINTY_ASSIGNED_CONTEXT((#42604))
GLOBAL_UNIT_ASSIGNED_CONTEXT((#42621,#42623,#42624))
REPRESENTATION_CONTEXT('','3D')
);
#42617=(
GEOMETRIC_REPRESENTATION_CONTEXT(3)
GLOBAL_UNCERTAINTY_ASSIGNED_CONTEXT((#42605))
GLOBAL_UNIT_ASSIGNED_CONTEXT((#42621,#42623,#42624))
REPRESENTATION_CONTEXT('','3D')
);
#42618=(
GEOMETRIC_REPRESENTATION_CONTEXT(3)
GLOBAL_UNCERTAINTY_ASSIGNED_CONTEXT((#42606))
GLOBAL_UNIT_ASSIGNED_CONTEXT((#42621,#42623,#42624))
REPRESENTATION_CONTEXT('','3D')
);
#42619=(
GEOMETRIC_REPRESENTATION_CONTEXT(3)
GLOBAL_UNCERTAINTY_ASSIGNED_CONTEXT((#42607))
GLOBAL_UNIT_ASSIGNED_CONTEXT((#42621,#42623,#42624))
REPRESENTATION_CONTEXT('','3D')
);
#42620=(
GEOMETRIC_REPRESENTATION_CONTEXT(3)
GLOBAL_UNCERTAINTY_ASSIGNED_CONTEXT((#42608))
GLOBAL_UNIT_ASSIGNED_CONTEXT((#42621,#42623,#42624))
REPRESENTATION_CONTEXT('','3D')
);
#42621=(
LENGTH_UNIT()
NAMED_UNIT(*)
SI_UNIT(.MILLI.,.METRE.)
);
#42622=(
LENGTH_UNIT()
NAMED_UNIT(*)
SI_UNIT($,.METRE.)
);
#42623=(
NAMED_UNIT(*)
PLANE_ANGLE_UNIT()
SI_UNIT($,.RADIAN.)
);
#42624=(
NAMED_UNIT(*)
SI_UNIT($,.STERADIAN.)
SOLID_ANGLE_UNIT()
);
#42625=SHAPE_DEFINITION_REPRESENTATION(#42636,#42722);
#42626=SHAPE_DEFINITION_REPRESENTATION(#42637,#42723);
#42627=SHAPE_DEFINITION_REPRESENTATION(#42638,#42724);
#42628=SHAPE_DEFINITION_REPRESENTATION(#42639,#42725);
#42629=SHAPE_DEFINITION_REPRESENTATION(#42640,#42726);
#42630=SHAPE_DEFINITION_REPRESENTATION(#42641,#42727);
#42631=SHAPE_DEFINITION_REPRESENTATION(#42642,#42728);
#42632=SHAPE_DEFINITION_REPRESENTATION(#42643,#42729);
#42633=SHAPE_DEFINITION_REPRESENTATION(#42644,#42730);
#42634=SHAPE_DEFINITION_REPRESENTATION(#42645,#42731);
#42635=SHAPE_DEFINITION_REPRESENTATION(#42646,#42732);
#42636=PRODUCT_DEFINITION_SHAPE('',$,#42734);
#42637=PRODUCT_DEFINITION_SHAPE('',$,#42735);
#42638=PRODUCT_DEFINITION_SHAPE('',$,#42736);
#42639=PRODUCT_DEFINITION_SHAPE('',$,#42737);
#42640=PRODUCT_DEFINITION_SHAPE('',$,#42738);
#42641=PRODUCT_DEFINITION_SHAPE('',$,#42739);
#42642=PRODUCT_DEFINITION_SHAPE('',$,#42740);
#42643=PRODUCT_DEFINITION_SHAPE('',$,#42741);
#42644=PRODUCT_DEFINITION_SHAPE('',$,#42742);
#42645=PRODUCT_DEFINITION_SHAPE('',$,#42743);
#42646=PRODUCT_DEFINITION_SHAPE('',$,#42744);
#42647=PRODUCT_DEFINITION_SHAPE($,$,#236);
#42648=PRODUCT_DEFINITION_SHAPE($,$,#237);
#42649=PRODUCT_DEFINITION_SHAPE($,$,#238);
#42650=PRODUCT_DEFINITION_SHAPE($,$,#239);
#42651=PRODUCT_DEFINITION_SHAPE($,$,#240);
#42652=PRODUCT_DEFINITION_SHAPE($,$,#241);
#42653=PRODUCT_DEFINITION_SHAPE($,$,#242);
#42654=PRODUCT_DEFINITION_SHAPE($,$,#243);
#42655=PRODUCT_DEFINITION_SHAPE($,$,#244);
#42656=PRODUCT_DEFINITION_SHAPE($,$,#245);
#42657=PRODUCT_DEFINITION_SHAPE($,$,#246);
#42658=PRODUCT_DEFINITION_SHAPE($,$,#247);
#42659=PRODUCT_DEFINITION_SHAPE($,$,#248);
#42660=PRODUCT_DEFINITION_SHAPE($,$,#249);
#42661=PRODUCT_DEFINITION_SHAPE($,$,#250);
#42662=PRODUCT_DEFINITION_SHAPE($,$,#251);
#42663=PRODUCT_DEFINITION_SHAPE($,$,#252);
#42664=PRODUCT_DEFINITION_SHAPE($,$,#253);
#42665=PRODUCT_DEFINITION_SHAPE($,$,#254);
#42666=PRODUCT_DEFINITION_SHAPE($,$,#255);
#42667=PRODUCT_DEFINITION_SHAPE($,$,#256);
#42668=PRODUCT_DEFINITION_SHAPE($,$,#257);
#42669=PRODUCT_DEFINITION_SHAPE($,$,#258);
#42670=PRODUCT_DEFINITION_SHAPE($,$,#259);
#42671=PRODUCT_DEFINITION_SHAPE($,$,#260);
#42672=PRODUCT_DEFINITION_SHAPE($,$,#261);
#42673=PRODUCT_DEFINITION_SHAPE($,$,#262);
#42674=PRODUCT_DEFINITION_SHAPE($,$,#263);
#42675=PRODUCT_DEFINITION_SHAPE($,$,#264);
#42676=PRODUCT_DEFINITION_SHAPE($,$,#265);
#42677=PRODUCT_DEFINITION_SHAPE($,$,#266);
#42678=PRODUCT_DEFINITION_SHAPE($,$,#267);
#42679=PRODUCT_DEFINITION_SHAPE($,$,#268);
#42680=PRODUCT_DEFINITION_SHAPE($,$,#269);
#42681=PRODUCT_DEFINITION_SHAPE($,$,#270);
#42682=PRODUCT_DEFINITION_SHAPE($,$,#271);
#42683=PRODUCT_DEFINITION_SHAPE($,$,#272);
#42684=PRODUCT_DEFINITION_SHAPE($,$,#273);
#42685=PRODUCT_DEFINITION_SHAPE($,$,#274);
#42686=PRODUCT_DEFINITION_SHAPE($,$,#275);
#42687=PRODUCT_DEFINITION_SHAPE($,$,#276);
#42688=PRODUCT_DEFINITION_SHAPE($,$,#277);
#42689=PRODUCT_DEFINITION_SHAPE($,$,#278);
#42690=PRODUCT_DEFINITION_SHAPE($,$,#279);
#42691=PRODUCT_DEFINITION_SHAPE($,$,#280);
#42692=PRODUCT_DEFINITION_SHAPE($,$,#281);
#42693=PRODUCT_DEFINITION_SHAPE($,$,#282);
#42694=PRODUCT_DEFINITION_SHAPE($,$,#283);
#42695=PRODUCT_DEFINITION_SHAPE($,$,#284);
#42696=PRODUCT_DEFINITION_SHAPE($,$,#285);
#42697=PRODUCT_DEFINITION_SHAPE($,$,#286);
#42698=PRODUCT_DEFINITION_SHAPE($,$,#287);
#42699=PRODUCT_DEFINITION_SHAPE($,$,#288);
#42700=PRODUCT_DEFINITION_SHAPE($,$,#289);
#42701=PRODUCT_DEFINITION_SHAPE($,$,#290);
#42702=PRODUCT_DEFINITION_SHAPE($,$,#291);
#42703=PRODUCT_DEFINITION_SHAPE($,$,#292);
#42704=PRODUCT_DEFINITION_SHAPE($,$,#293);
#42705=PRODUCT_DEFINITION_SHAPE($,$,#294);
#42706=PRODUCT_DEFINITION_SHAPE($,$,#295);
#42707=PRODUCT_DEFINITION_SHAPE($,$,#296);
#42708=PRODUCT_DEFINITION_SHAPE($,$,#297);
#42709=PRODUCT_DEFINITION_SHAPE($,$,#298);
#42710=PRODUCT_DEFINITION_SHAPE($,$,#299);
#42711=PRODUCT_DEFINITION_SHAPE($,$,#300);
#42712=PRODUCT_DEFINITION_SHAPE($,$,#301);
#42713=PRODUCT_DEFINITION_SHAPE($,$,#302);
#42714=PRODUCT_DEFINITION_SHAPE($,$,#303);
#42715=PRODUCT_DEFINITION_SHAPE($,$,#304);
#42716=PRODUCT_DEFINITION_SHAPE($,$,#305);
#42717=PRODUCT_DEFINITION_SHAPE($,$,#306);
#42718=PRODUCT_DEFINITION_SHAPE($,$,#307);
#42719=PRODUCT_DEFINITION_SHAPE($,$,#308);
#42720=PRODUCT_DEFINITION_SHAPE($,$,#309);
#42721=PRODUCT_DEFINITION_SHAPE($,$,#310);
#42722=SHAPE_REPRESENTATION('',(#10504,#11231,#11232,#11233,#11234,#11235,
#11236,#11237,#11238,#11239,#11240,#11241,#11242,#11243,#11244,#11245,#11246,
#11247,#11248,#11249,#11250,#11251,#11252,#11253,#11254,#11255,#11256,#11257,
#11258,#11259,#11260,#11261,#11262,#11263,#11264,#11265,#11266,#11267,#11268,
#11269,#11270,#11271,#11272,#11273,#11274,#11275,#11276,#11277,#11278,#11279,
#11280,#11281,#11282,#11283,#11284,#11285,#11286,#11287,#11288,#11289,#11290,
#11291,#11292,#11293,#11294,#11295,#11296,#11297,#11298,#11299,#11300,#11301,
#11302,#11303,#11304,#11305),#42609);
#42723=SHAPE_REPRESENTATION('',(#10505),#42610);
#42724=SHAPE_REPRESENTATION('',(#10921),#42611);
#42725=SHAPE_REPRESENTATION('',(#10940),#42612);
#42726=SHAPE_REPRESENTATION('',(#10963),#42613);
#42727=SHAPE_REPRESENTATION('',(#10972),#42614);
#42728=SHAPE_REPRESENTATION('',(#11033),#42615);
#42729=SHAPE_REPRESENTATION('',(#11061),#42616);
#42730=SHAPE_REPRESENTATION('',(#11115),#42617);
#42731=SHAPE_REPRESENTATION('',(#11159),#42618);
#42732=SHAPE_REPRESENTATION('',(#11222),#42619);
#42733=PRODUCT_DEFINITION_CONTEXT('part definition',#42768,'design');
#42734=PRODUCT_DEFINITION('MAS-643','MAS-643',#42745,#42733);
#42735=PRODUCT_DEFINITION('Fluid header','Fluid header',#42746,#42733);
#42736=PRODUCT_DEFINITION('Service cover','Service cover',#42747,#42733);
#42737=PRODUCT_DEFINITION('Cover gasket','Cover gasket',#42748,#42733);
#42738=PRODUCT_DEFINITION('Heat transfer tube','Heat transfer tube',#42749,
#42733);
#42739=PRODUCT_DEFINITION('Heat transfer fin','Heat transfer fin',#42750,
#42733);
#42740=PRODUCT_DEFINITION('Mounting foot','Mounting foot',#42751,#42733);
#42741=PRODUCT_DEFINITION('Socket head cap screw M4x12',
'Socket head cap screw M4x12',#42752,#42733);
#42742=PRODUCT_DEFINITION('Socket head cap screw M6x12',
'Socket head cap screw M6x12',#42753,#42733);
#42743=PRODUCT_DEFINITION('Hose connection','Hose connection',#42754,#42733);
#42744=PRODUCT_DEFINITION('Connection face seal','Connection face seal',
#42755,#42733);
#42745=PRODUCT_DEFINITION_FORMATION('',$,#42770);
#42746=PRODUCT_DEFINITION_FORMATION('',$,#42771);
#42747=PRODUCT_DEFINITION_FORMATION('',$,#42772);
#42748=PRODUCT_DEFINITION_FORMATION('',$,#42773);
#42749=PRODUCT_DEFINITION_FORMATION('',$,#42774);
#42750=PRODUCT_DEFINITION_FORMATION('',$,#42775);
#42751=PRODUCT_DEFINITION_FORMATION('',$,#42776);
#42752=PRODUCT_DEFINITION_FORMATION('',$,#42777);
#42753=PRODUCT_DEFINITION_FORMATION('',$,#42778);
#42754=PRODUCT_DEFINITION_FORMATION('',$,#42779);
#42755=PRODUCT_DEFINITION_FORMATION('',$,#42780);
#42756=PRODUCT_RELATED_PRODUCT_CATEGORY('MAS-643','MAS-643',(#42770));
#42757=PRODUCT_RELATED_PRODUCT_CATEGORY('Fluid header','Fluid header',(#42771));
#42758=PRODUCT_RELATED_PRODUCT_CATEGORY('Service cover','Service cover',
(#42772));
#42759=PRODUCT_RELATED_PRODUCT_CATEGORY('Cover gasket','Cover gasket',(#42773));
#42760=PRODUCT_RELATED_PRODUCT_CATEGORY('Heat transfer tube',
'Heat transfer tube',(#42774));
#42761=PRODUCT_RELATED_PRODUCT_CATEGORY('Heat transfer fin',
'Heat transfer fin',(#42775));
#42762=PRODUCT_RELATED_PRODUCT_CATEGORY('Mounting foot','Mounting foot',
(#42776));
#42763=PRODUCT_RELATED_PRODUCT_CATEGORY('Socket head cap screw M4x12',
'Socket head cap screw M4x12',(#42777));
#42764=PRODUCT_RELATED_PRODUCT_CATEGORY('Socket head cap screw M6x12',
'Socket head cap screw M6x12',(#42778));
#42765=PRODUCT_RELATED_PRODUCT_CATEGORY('Hose connection',
'Hose connection',(#42779));
#42766=PRODUCT_RELATED_PRODUCT_CATEGORY('Connection face seal',
'Connection face seal',(#42780));
#42767=APPLICATION_PROTOCOL_DEFINITION('international standard',
'automotive_design',2009,#42768);
#42768=APPLICATION_CONTEXT(
'Core Data for Automotive Mechanical Design Process');
#42769=PRODUCT_CONTEXT('part definition',#42768,'mechanical');
#42770=PRODUCT('MAS-643','MAS-643',
'Independent eighteen-tube parallel-flow evaporator geometry. Repeated
 machined headers and gasketed service covers, eighteen copper tubes, 
twenty-nine punched fins, threaded hose connections and bolted mountin
g feet. Native editable features and instanced parts. Braze details, w
orking fluid, pressure and thermal ratings require engineering selecti
on.',(#42769));
#42771=PRODUCT('Fluid header','Fluid header',$,(#42769));
#42772=PRODUCT('Service cover','Service cover',$,(#42769));
#42773=PRODUCT('Cover gasket','Cover gasket',$,(#42769));
#42774=PRODUCT('Heat transfer tube','Heat transfer tube',$,(#42769));
#42775=PRODUCT('Heat transfer fin','Heat transfer fin',$,(#42769));
#42776=PRODUCT('Mounting foot','Mounting foot','Mounting foot',(#42769));
#42777=PRODUCT('Socket head cap screw M4x12',
'Socket head cap screw M4x12',$,(#42769));
#42778=PRODUCT('Socket head cap screw M6x12',
'Socket head cap screw M6x12',$,(#42769));
#42779=PRODUCT('Hose connection','Hose connection',$,(#42769));
#42780=PRODUCT('Connection face seal','Connection face seal',$,(#42769));
#42781=PRESENTATION_STYLE_ASSIGNMENT((#42789));
#42782=PRESENTATION_STYLE_ASSIGNMENT((#42790));
#42783=PRESENTATION_STYLE_ASSIGNMENT((#42791));
#42784=PRESENTATION_STYLE_ASSIGNMENT((#42792));
#42785=PRESENTATION_STYLE_ASSIGNMENT((#42793));
#42786=PRESENTATION_STYLE_ASSIGNMENT((#42794));
#42787=PRESENTATION_STYLE_ASSIGNMENT((#42795));
#42788=PRESENTATION_STYLE_ASSIGNMENT((#42796));
#42789=SURFACE_STYLE_USAGE(.BOTH.,#42797);
#42790=SURFACE_STYLE_USAGE(.BOTH.,#42798);
#42791=SURFACE_STYLE_USAGE(.BOTH.,#42799);
#42792=SURFACE_STYLE_USAGE(.BOTH.,#42800);
#42793=SURFACE_STYLE_USAGE(.BOTH.,#42801);
#42794=SURFACE_STYLE_USAGE(.BOTH.,#42802);
#42795=SURFACE_STYLE_USAGE(.BOTH.,#42803);
#42796=SURFACE_STYLE_USAGE(.BOTH.,#42804);
#42797=SURFACE_SIDE_STYLE('',(#42805));
#42798=SURFACE_SIDE_STYLE('',(#42806));
#42799=SURFACE_SIDE_STYLE('',(#42807));
#42800=SURFACE_SIDE_STYLE('',(#42808));
#42801=SURFACE_SIDE_STYLE('',(#42809));
#42802=SURFACE_SIDE_STYLE('',(#42810));
#42803=SURFACE_SIDE_STYLE('',(#42811));
#42804=SURFACE_SIDE_STYLE('',(#42812));
#42805=SURFACE_STYLE_FILL_AREA(#42813);
#42806=SURFACE_STYLE_FILL_AREA(#42814);
#42807=SURFACE_STYLE_FILL_AREA(#42815);
#42808=SURFACE_STYLE_FILL_AREA(#42816);
#42809=SURFACE_STYLE_FILL_AREA(#42817);
#42810=SURFACE_STYLE_FILL_AREA(#42818);
#42811=SURFACE_STYLE_FILL_AREA(#42819);
#42812=SURFACE_STYLE_FILL_AREA(#42820);
#42813=FILL_AREA_STYLE('Steel - Satin',(#42821));
#42814=FILL_AREA_STYLE('Dark blue',(#42822));
#42815=FILL_AREA_STYLE('Sky blue',(#42823));
#42816=FILL_AREA_STYLE('Dark gray',(#42824));
#42817=FILL_AREA_STYLE('Light blue',(#42825));
#42818=FILL_AREA_STYLE('Light gray',(#42826));
#42819=FILL_AREA_STYLE('Gray',(#42827));
#42820=FILL_AREA_STYLE('Black',(#42828));
#42821=FILL_AREA_STYLE_COLOUR('Steel - Satin',#42829);
#42822=FILL_AREA_STYLE_COLOUR('Dark blue',#42830);
#42823=FILL_AREA_STYLE_COLOUR('Sky blue',#42831);
#42824=FILL_AREA_STYLE_COLOUR('Dark gray',#42832);
#42825=FILL_AREA_STYLE_COLOUR('Light blue',#42833);
#42826=FILL_AREA_STYLE_COLOUR('Light gray',#42834);
#42827=FILL_AREA_STYLE_COLOUR('Gray',#42835);
#42828=FILL_AREA_STYLE_COLOUR('Black',#42836);
#42829=COLOUR_RGB('Steel - Satin',0.627450980392157,0.627450980392157,0.627450980392157);
#42830=COLOUR_RGB('Dark blue',0.0901960784313725,0.270588235294118,0.513725490196078);
#42831=COLOUR_RGB('Sky blue',0.317647058823529,0.686274509803922,0.890196078431372);
#42832=COLOUR_RGB('Dark gray',0.250980392156863,0.282352941176471,0.32156862745098);
#42833=COLOUR_RGB('Light blue',0.662745098039216,0.831372549019608,0.949019607843137);
#42834=COLOUR_RGB('Light gray',0.725490196078431,0.752941176470588,0.792156862745098);
#42835=COLOUR_RGB('Gray',0.407843137254902,0.447058823529412,0.498039215686275);
#42836=COLOUR_RGB('Black',0.137254901960784,0.152941176470588,0.176470588235294);
ENDSEC;
END-ISO-10303-21;
